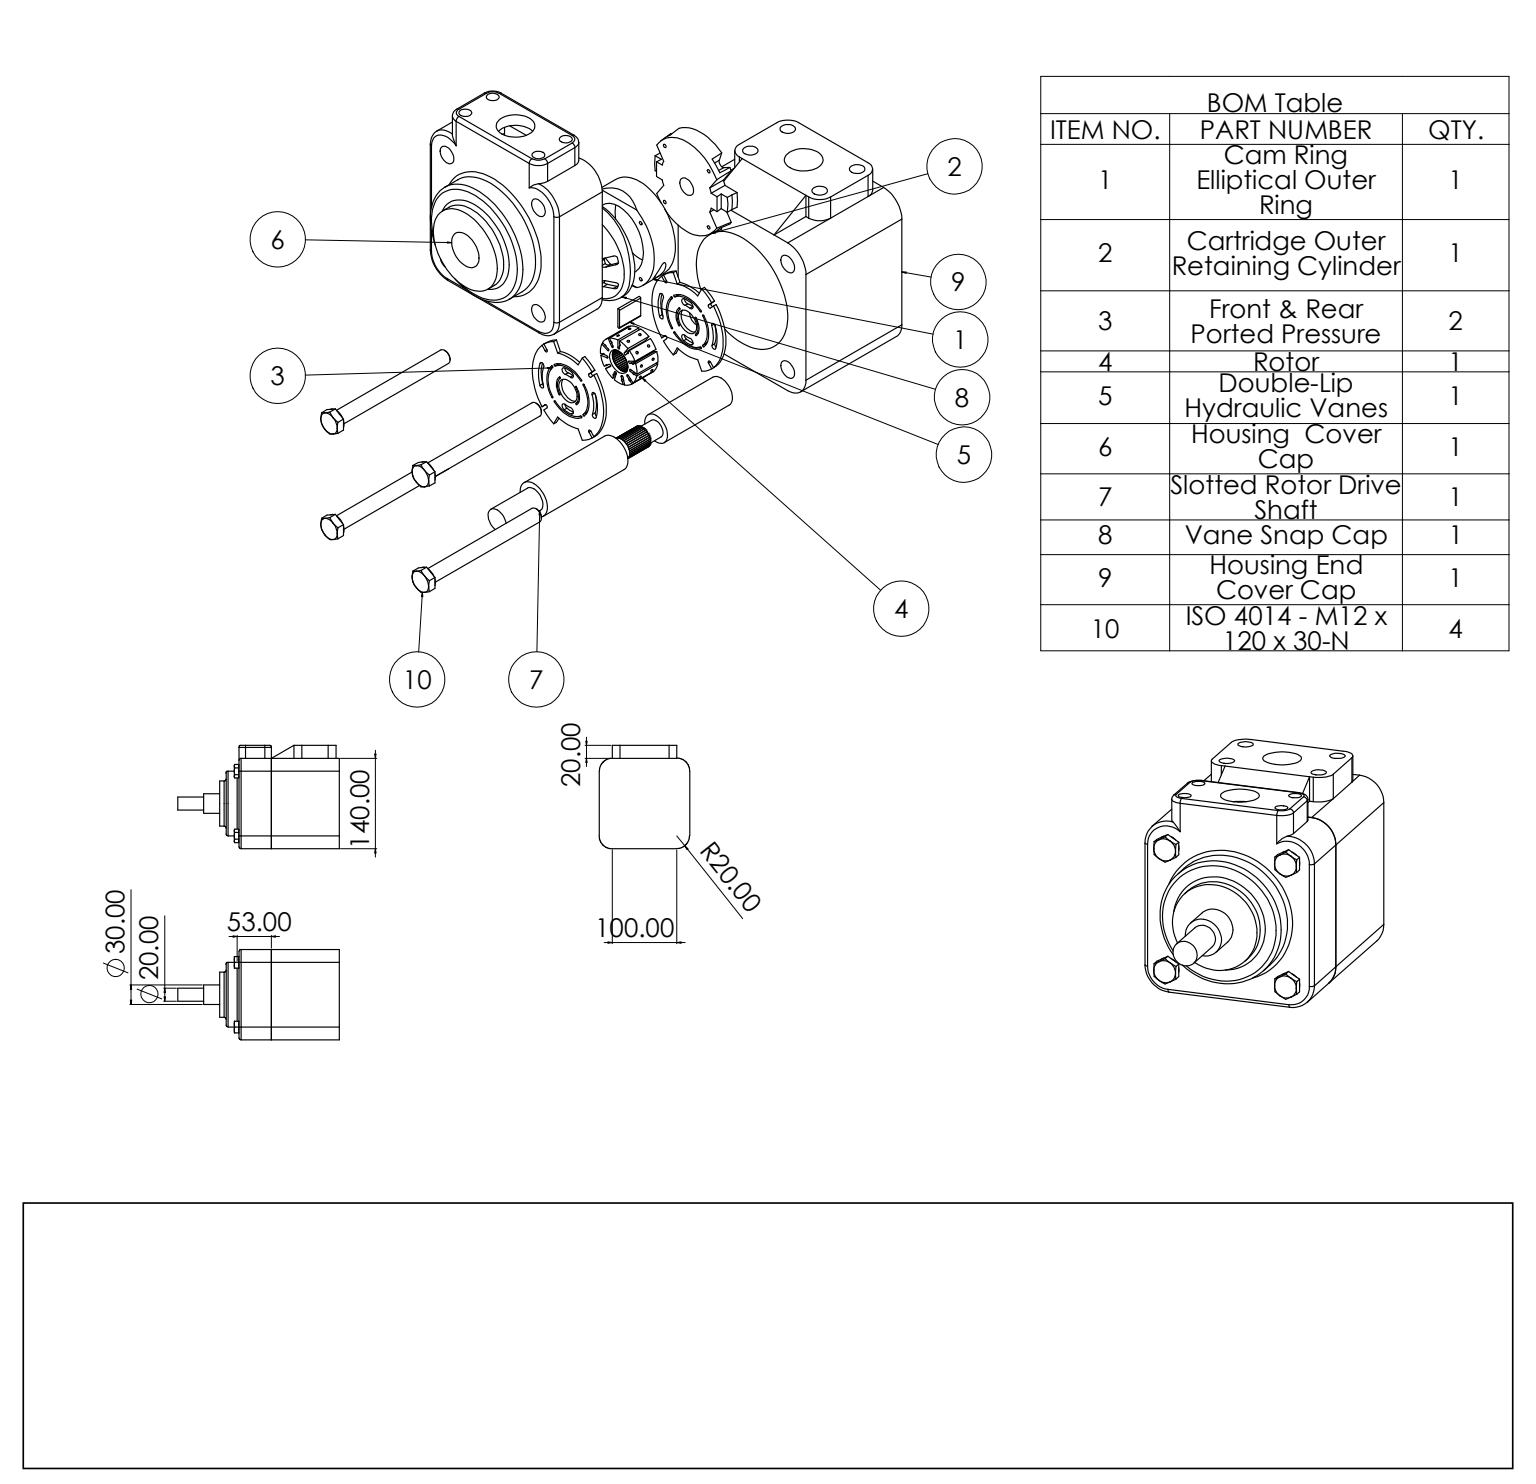
ISO-10303-21;
HEADER;
FILE_DESCRIPTION (('STEP AP214'),
    '1' );
FILE_NAME ('MAS-342',
    '2026-10-18T20:16:25',
    ( '' ),
    ( '' ),
    'SwSTEP 2.0',
    'SolidWorks 2025',
    '' );
FILE_SCHEMA (( 'AUTOMOTIVE_DESIGN' ));
ENDSEC;

DATA;
#1 = FACE_OUTER_BOUND ( 'NONE', #19385, .T. ) ;
#2 = DIRECTION ( 'NONE',  ( 0.000000000000000000, 0.000000000000000000, -1.000000000000000000 ) ) ;
#3 = CARTESIAN_POINT ( 'NONE',  ( 37.16608720827707657, 51.86186943028246787, 12.49999999999999112 ) ) ;
#4 = AXIS2_PLACEMENT_3D ( 'NONE', #28751, #28908, #7543 ) ;
#5 = CARTESIAN_POINT ( 'NONE',  ( -18.15804816958924306, -34.11099862341368549, 27.50000000000000000 ) ) ;
#6 = ADVANCED_FACE ( 'NONE', ( #26858 ), #19364, .F. ) ;
#7 = CARTESIAN_POINT ( 'NONE',  ( -10.18506332983503881, -29.04537757311073065, 24.50000000000000000 ) ) ;
#8 = EDGE_LOOP ( 'NONE', ( #14143, #4167, #13185, #29281 ) ) ;
#9 = CARTESIAN_POINT ( 'NONE',  ( -8.101746394734353984, -38.49011865887880646, 34.49999999999998579 ) ) ;
#10 = DIRECTION ( 'NONE',  ( 1.000000000000000000, 0.000000000000000000, 0.000000000000000000 ) ) ;
#11 = AXIS2_PLACEMENT_3D ( 'NONE', #21550, #14547, #24043 ) ;
#12 = DIRECTION ( 'NONE',  ( 1.000000000000000000, 0.000000000000000000, 0.000000000000000000 ) ) ;
#13 = EDGE_LOOP ( 'NONE', ( #16874, #3981 ) ) ;
#14 = CARTESIAN_POINT ( 'NONE',  ( 0.000000000000000000, 0.000000000000000000, 12.49999999999998401 ) ) ;
#15 = ORIENTED_EDGE ( 'NONE', *, *, #5581, .T. ) ;
#16 = CARTESIAN_POINT ( 'NONE',  ( 6.437793815610356241, -6.974883619896809606, 1.500000000000001332 ) ) ;
#17 = CARTESIAN_POINT ( 'NONE',  ( -9.060903275275968838, 42.96476308719554993, -16.50000000000000000 ) ) ;
#18 = VERTEX_POINT ( 'NONE', #24496 ) ;
#19 = CARTESIAN_POINT ( 'NONE',  ( 24.39344986792568903, -29.07448411189255211, 27.50000000000001066 ) ) ;
#20 = EDGE_CURVE ( 'NONE', #8430, #1741, #30742, .T. ) ;
#21 = CARTESIAN_POINT ( 'NONE',  ( -49.99999999999955236, -4.926614671774132148E-13, 82.49999999999998579 ) ) ;
#22 = EDGE_CURVE ( 'NONE', #25287, #29372, #18804, .T. ) ;
#23 = LINE ( 'NONE', #9535, #4037 ) ;
#24 = CARTESIAN_POINT ( 'NONE',  ( 0.3552109633508558351, -3.484997970623677332, -9.000000000000000000 ) ) ;
#25 = AXIS2_PLACEMENT_3D ( 'NONE', #902, #17278, #15225 ) ;
#26 = CARTESIAN_POINT ( 'NONE',  ( 30.75232512042845556, -9.966982604840845639, 1.500000000000000000 ) ) ;
#27 = ADVANCED_FACE ( 'NONE', ( #781 ), #12350, .T. ) ;
#28 = FACE_OUTER_BOUND ( 'NONE', #21455, .T. ) ;
#29 = ORIENTED_EDGE ( 'NONE', *, *, #10327, .T. ) ;
#30 = EDGE_CURVE ( 'NONE', #13253, #5262, #636, .T. ) ;
#31 = DIRECTION ( 'NONE',  ( 0.000000000000000000, 0.000000000000000000, 1.000000000000000000 ) ) ;
#32 = CARTESIAN_POINT ( 'NONE',  ( -20.65888525914364493, -38.75220717792906555, -19.50000000000000355 ) ) ;
#33 = CARTESIAN_POINT ( 'NONE',  ( -3.912171961292007616, -8.637616862297829101, 1.500000000000001332 ) ) ;
#34 = VERTEX_POINT ( 'NONE', #489 ) ;
#35 = EDGE_CURVE ( 'NONE', #21045, #27073, #21273, .T. ) ;
#36 = DIRECTION ( 'NONE',  ( -0.000000000000000000, -0.000000000000000000, 1.000000000000000000 ) ) ;
#37 = CARTESIAN_POINT ( 'NONE',  ( -14.84326473672822821, -8.425446036094903945, 20.06253562465620632 ) ) ;
#39 = EDGE_CURVE ( 'NONE', #26631, #4645, #16306, .T. ) ;
#38 = CARTESIAN_POINT ( 'NONE',  ( 0.000000000000000000, 0.000000000000000000, 1.500000000000001332 ) ) ;
#40 = CARTESIAN_POINT ( 'NONE',  ( 4.967306913940536361, 16.28142803850090203, 6.973843882838223429 ) ) ;
#41 = CARTESIAN_POINT ( 'NONE',  ( 39.83602371821015709, 11.57901747687536265, -19.50000000000000355 ) ) ;
#42 = EDGE_CURVE ( 'NONE', #19602, #22873, #7666, .T. ) ;
#43 = ORIENTED_EDGE ( 'NONE', *, *, #8838, .F. ) ;
#44 = LINE ( 'NONE', #17187, #10483 ) ;
#45 = EDGE_CURVE ( 'NONE', #5916, #3823, #10340, .T. ) ;
#46 = CARTESIAN_POINT ( 'NONE',  ( -24.03057240117690441, -26.57182937991348481, 26.54355021145563143 ) ) ;
#47 = CARTESIAN_POINT ( 'NONE',  ( 36.14613918203227172, 16.01870328439765601, 34.83083827288849221 ) ) ;
#48 = CARTESIAN_POINT ( 'NONE',  ( -6.228680293130167911, 19.00574304797303782, 5.679672709359373073 ) ) ;
#49 = ORIENTED_EDGE ( 'NONE', *, *, #24996, .T. ) ;
#50 = AXIS2_PLACEMENT_3D ( 'NONE', #18602, #5013, #4398 ) ;
#51 = CARTESIAN_POINT ( 'NONE',  ( 6.812559277181973627, -5.881244434206257310, 21.50000000000000000 ) ) ;
#52 = VERTEX_POINT ( 'NONE', #10007 ) ;
#53 = DIRECTION ( 'NONE',  ( 0.8412535328311813165, -0.5406408174555974444, 0.000000000000000000 ) ) ;
#54 = DIRECTION ( 'NONE',  ( 0.000000000000000000, 0.000000000000000000, 1.000000000000000000 ) ) ;
#55 = ORIENTED_EDGE ( 'NONE', *, *, #18763, .T. ) ;
#56 = ORIENTED_EDGE ( 'NONE', *, *, #27505, .T. ) ;
#57 = DIRECTION ( 'NONE',  ( -0.000000000000000000, -0.000000000000000000, 1.000000000000000000 ) ) ;
#58 =( REPRESENTATION_RELATIONSHIP ('NONE','NONE', #19885, #12322 ) REPRESENTATION_RELATIONSHIP_WITH_TRANSFORMATION ( #695 )SHAPE_REPRESENTATION_RELATIONSHIP( ) );
#59 = ORIENTED_EDGE ( 'NONE', *, *, #6132, .F. ) ;
#60 = ORIENTED_EDGE ( 'NONE', *, *, #10139, .T. ) ;
#61 = CARTESIAN_POINT ( 'NONE',  ( -0.02177409673011774377, -17.02558975896787885, 19.96783386855779341 ) ) ;
#62 = ADVANCED_FACE ( 'NONE', ( #24650 ), #17167, .F. ) ;
#63 = EDGE_CURVE ( 'NONE', #25705, #14162, #9332, .T. ) ;
#64 = CARTESIAN_POINT ( 'NONE',  ( -9.983339604393949074, -17.35078046477759983, 7.441806358946449151 ) ) ;
#65 = FACE_OUTER_BOUND ( 'NONE', #13496, .T. ) ;
#66 = CARTESIAN_POINT ( 'NONE',  ( 1.363408835038997458, -19.97112866468682668, 19.47783254395485031 ) ) ;
#67 = ORIENTED_EDGE ( 'NONE', *, *, #8805, .T. ) ;
#68 = EDGE_CURVE ( 'NONE', #8257, #20089, #6832, .T. ) ;
#69 = CARTESIAN_POINT ( 'NONE',  ( 6.899999999999999467, 5.196152422706624030, 9.000000000000001776 ) ) ;
#70 = CARTESIAN_POINT ( 'NONE',  ( 0.000000000000000000, 13.00000000000001421, 1.500000000000001332 ) ) ;
#71 = CARTESIAN_POINT ( 'NONE',  ( 14.24237608451263171, 14.06627278277045257, 19.69140814234746273 ) ) ;
#72 = LINE ( 'NONE', #9585, #22578 ) ;
#73 = ORIENTED_EDGE ( 'NONE', *, *, #24989, .F. ) ;
#74 = AXIS2_PLACEMENT_3D ( 'NONE', #21270, #28002, #15999 ) ;
#75 = DIRECTION ( 'NONE',  ( 0.000000000000000000, 0.000000000000000000, 1.000000000000000000 ) ) ;
#76 = CARTESIAN_POINT ( 'NONE',  ( -17.59891439103365585, -9.538503746949022144, 6.672349528511551497 ) ) ;
#77 = CARTESIAN_POINT ( 'NONE',  ( -13.11527592942575282, -10.04126165406389326, 1.500000000000000000 ) ) ;
#78 = DIRECTION ( 'NONE',  ( -1.000000000000000000, 0.000000000000000000, 0.000000000000000000 ) ) ;
#79 = CARTESIAN_POINT ( 'NONE',  ( 0.000000000000000000, 0.000000000000000000, 9.000000000000000000 ) ) ;
#80 = EDGE_CURVE ( 'NONE', #24431, #1715, #12846, .T. ) ;
#81 = CARTESIAN_POINT ( 'NONE',  ( -1.073881485057447405, -0.9711784013058452070, 1.500000000000000000 ) ) ;
#82 = CARTESIAN_POINT ( 'NONE',  ( 6.900000000000000355, 0.000000000000000000, 0.000000000000000000 ) ) ;
#83 = EDGE_LOOP ( 'NONE', ( #20575, #9372 ) ) ;
#84 = ORIENTED_EDGE ( 'NONE', *, *, #27745, .T. ) ;
#85 = CARTESIAN_POINT ( 'NONE',  ( -37.98493438988125348, -11.12428508575252728, -1.500000000000000000 ) ) ;
#86 = DIRECTION ( 'NONE',  ( 0.000000000000000000, 0.000000000000000000, -1.000000000000000000 ) ) ;
#88 = DIRECTION ( 'NONE',  ( 1.000000000000000000, 0.000000000000000000, 0.000000000000000000 ) ) ;
#87 = VECTOR ( 'NONE', #19138, 1000.000000000000000 ) ;
#89 = ORIENTED_EDGE ( 'NONE', *, *, #20188, .F. ) ;
#90 = CARTESIAN_POINT ( 'NONE',  ( 15.47797589786116923, -7.092492006142040673, 19.96783386855779341 ) ) ;
#91 = CARTESIAN_POINT ( 'NONE',  ( 6.171684994647412381, 19.04275422834224685, 6.211014596808754007 ) ) ;
#92 = EDGE_CURVE ( 'NONE', #21118, #30725, #17328, .T. ) ;
#93 = ORIENTED_EDGE ( 'NONE', *, *, #3486, .F. ) ;
#94 = DIRECTION ( 'NONE',  ( 1.000000000000000000, 0.000000000000000000, 0.000000000000000000 ) ) ;
#95 = CARTESIAN_POINT ( 'NONE',  ( 11.67645754117908830, 12.46194352177089293, 6.892848776733236704 ) ) ;
#96 = EDGE_CURVE ( 'NONE', #21713, #6692, #24023, .T. ) ;
#97 = FACE_OUTER_BOUND ( 'NONE', #28084, .T. ) ;
#98 = CARTESIAN_POINT ( 'NONE',  ( -37.93368909164158254, 9.961195697873989729, 34.97277436636965575 ) ) ;
#99 = ORIENTED_EDGE ( 'NONE', *, *, #3233, .T. ) ;
#100 = CARTESIAN_POINT ( 'NONE',  ( 0.000000000000000000, 0.000000000000000000, 1.500000000000001332 ) ) ;
#101 = CARTESIAN_POINT ( 'NONE',  ( 0.000000000000000000, 0.000000000000000000, -87.50000000000000000 ) ) ;
#102 = CARTESIAN_POINT ( 'NONE',  ( 22.58267429318970443, -26.57182937991349903, 26.54355021145563143 ) ) ;
#103 = ORIENTED_EDGE ( 'NONE', *, *, #23860, .T. ) ;
#104 = CARTESIAN_POINT ( 'NONE',  ( -18.38748676655956515, -7.913428453147655084, 6.018569869498933578 ) ) ;
#105 = CARTESIAN_POINT ( 'NONE',  ( 14.46116907065692736, 13.81605838820130394, 7.454606537396340826 ) ) ;
#106 = CARTESIAN_POINT ( 'NONE',  ( 0.06889080212831104333, -17.02733034922398758, 5.940635272151477686 ) ) ;
#107 = CYLINDRICAL_SURFACE ( 'NONE', #23715, 10.00000000000003375 ) ;
#108 = LINE ( 'NONE', #21001, #12544 ) ;
#109 = CARTESIAN_POINT ( 'NONE',  ( -19.94989956810792009, 1.646935350084928418, 19.89182036555910571 ) ) ;
#110 = DIRECTION ( 'NONE',  ( 0.000000000000000000, 1.000000000000000000, 0.000000000000000000 ) ) ;
#111 = ORIENTED_EDGE ( 'NONE', *, *, #4642, .T. ) ;
#112 = CARTESIAN_POINT ( 'NONE',  ( 11.47892014274828654, -16.39977715623752275, 20.25542030744407640 ) ) ;
#113 = CIRCLE ( 'NONE', #24448, 0.7500000000000007772 ) ;
#114 = CARTESIAN_POINT ( 'NONE',  ( 57.49999999999998579, -50.00000000000000000, 97.07879600563551037 ) ) ;
#115 = VERTEX_POINT ( 'NONE', #22003 ) ;
#116 = EDGE_LOOP ( 'NONE', ( #16345, #15698, #26338, #11828 ) ) ;
#117 = CARTESIAN_POINT ( 'NONE',  ( 4.695984468547702129, 19.44110619659980799, 20.15039051365864253 ) ) ;
#118 = CARTESIAN_POINT ( 'NONE',  ( -12.19297718786180695, 48.49133510641088662, -63.75033992389879245 ) ) ;
#119 = VERTEX_POINT ( 'NONE', #15443 ) ;
#120 = FACE_OUTER_BOUND ( 'NONE', #29698, .T. ) ;
#121 = VECTOR ( 'NONE', #17231, 1000.000000000000000 ) ;
#122 = CARTESIAN_POINT ( 'NONE',  ( -10.72135862580927146, -16.90494006806149940, 7.632642797338977658 ) ) ;
#123 = ORIENTED_EDGE ( 'NONE', *, *, #26128, .F. ) ;
#124 = AXIS2_PLACEMENT_3D ( 'NONE', #18042, #3695, #8540 ) ;
#125 = CARTESIAN_POINT ( 'NONE',  ( 18.71580048965418541, -7.100988023106708624, 19.03762469184452755 ) ) ;
#126 = CARTESIAN_POINT ( 'NONE',  ( 16.55849529797290032, 4.179294809495488039, 19.14333282897057842 ) ) ;
#127 = EDGE_CURVE ( 'NONE', #8705, #8129, #11228, .T. ) ;
#128 = CARTESIAN_POINT ( 'NONE',  ( 0.000000000000000000, -2.435693370351110282E-15, 21.50000000000000355 ) ) ;
#129 = ORIENTED_EDGE ( 'NONE', *, *, #25599, .F. ) ;
#130 = EDGE_CURVE ( 'NONE', #28271, #10764, #20221, .T. ) ;
#131 = CARTESIAN_POINT ( 'NONE',  ( 23.21352257770656635, -10.78826658734920052, 45.15942333309103418 ) ) ;
#132 = ORIENTED_EDGE ( 'NONE', *, *, #23307, .F. ) ;
#133 = ORIENTED_EDGE ( 'NONE', *, *, #19082, .T. ) ;
#134 = CARTESIAN_POINT ( 'NONE',  ( 7.706848733600953238, 5.524309650260795124, 1.500000000000001332 ) ) ;
#135 = CARTESIAN_POINT ( 'NONE',  ( -12.90456292687989759, 11.10871050118981529, 20.05479082170252525 ) ) ;
#136 = CARTESIAN_POINT ( 'NONE',  ( -9.972083266784119715, -17.35726207598482773, 18.56793045041961321 ) ) ;
#137 = CARTESIAN_POINT ( 'NONE',  ( -15.05112753842527162, -8.020416455032004066, 20.34789198813115263 ) ) ;
#138 = AXIS2_PLACEMENT_3D ( 'NONE', #523, #22041, #27196 ) ;
#139 = CARTESIAN_POINT ( 'NONE',  ( 1.767905995611233072, -16.98559759804142288, 19.61324152429826739 ) ) ;
#140 = CARTESIAN_POINT ( 'NONE',  ( 16.82202058066696537, 2.664153601443035146, 18.49267272388512140 ) ) ;
#141 = ORIENTED_EDGE ( 'NONE', *, *, #9150, .T. ) ;
#142 = AXIS2_PLACEMENT_3D ( 'NONE', #29835, #3468, #10482 ) ;
#143 = CARTESIAN_POINT ( 'NONE',  ( 11.01999061743883956, -16.71182566173002826, 7.652108011868850035 ) ) ;
#144 = CARTESIAN_POINT ( 'NONE',  ( 8.480328572437745294, -4.608906612435629491, 21.50000000000000000 ) ) ;
#145 = LINE ( 'NONE', #9510, #21267 ) ;
#146 = ORIENTED_EDGE ( 'NONE', *, *, #2958, .F. ) ;
#147 = LINE ( 'NONE', #19489, #17289 ) ;
#148 = CARTESIAN_POINT ( 'NONE',  ( -37.16608720827707657, -65.00000000000000000, 57.49999999999999289 ) ) ;
#149 = CARTESIAN_POINT ( 'NONE',  ( 1.000000000000008438, 13.00000000000001421, 1.500000000000001332 ) ) ;
#150 = CARTESIAN_POINT ( 'NONE',  ( 2.878478920843521749, -0.8451976705243363641, 24.50000000000000000 ) ) ;
#151 = CARTESIAN_POINT ( 'NONE',  ( 12.00212711880201510, 12.12705342296112221, 7.545655578832108468 ) ) ;
#152 = CARTESIAN_POINT ( 'NONE',  ( 8.099999999999999645, 0.000000000000000000, 0.000000000000000000 ) ) ;
#153 = CARTESIAN_POINT ( 'NONE',  ( -5.488535287689156661, 19.23255048776057308, 5.775318986477953054 ) ) ;
#154 = VERTEX_POINT ( 'NONE', #22460 ) ;
#155 = CARTESIAN_POINT ( 'NONE',  ( -7.108788511070779137, -38.72574257930638453, 34.49999999999999289 ) ) ;
#156 = DIRECTION ( 'NONE',  ( -0.000000000000000000, 0.000000000000000000, 1.000000000000000000 ) ) ;
#157 = ORIENTED_EDGE ( 'NONE', *, *, #6998, .F. ) ;
#158 = DIRECTION ( 'NONE',  ( 1.000000000000000000, 0.000000000000000000, 0.000000000000000000 ) ) ;
#159 = VECTOR ( 'NONE', #18850, 1000.000000000000000 ) ;
#160 = VERTEX_POINT ( 'NONE', #4060 ) ;
#161 = CARTESIAN_POINT ( 'NONE',  ( 16.17271416092067682, -5.480318835022405466, 6.995624166085161910 ) ) ;
#162 = AXIS2_PLACEMENT_3D ( 'NONE', #23397, #25742, #23542 ) ;
#163 = DIRECTION ( 'NONE',  ( 1.000000000000000000, 0.000000000000000000, -0.000000000000000000 ) ) ;
#164 = DIRECTION ( 'NONE',  ( 1.000000000000000000, -0.000000000000000000, 0.000000000000000000 ) ) ;
#165 = VERTEX_POINT ( 'NONE', #8736 ) ;
#166 = CARTESIAN_POINT ( 'NONE',  ( 22.55938241427807256, 30.80590877286595841, 27.50000000000000355 ) ) ;
#167 = DIRECTION ( 'NONE',  ( 1.000000000000000000, 0.000000000000000000, 0.000000000000000000 ) ) ;
#168 = LINE ( 'NONE', #19198, #17487 ) ;
#169 = CARTESIAN_POINT ( 'NONE',  ( 32.24119435725080507, -26.76047165977712794, -16.50000600000000262 ) ) ;
#170 = DIRECTION ( 'NONE',  ( -0.000000000000000000, -0.000000000000000000, 1.000000000000000000 ) ) ;
#171 = CARTESIAN_POINT ( 'NONE',  ( -30.03865005752669148, 15.52610542268208604, 41.18623755349101856 ) ) ;
#172 = ORIENTED_EDGE ( 'NONE', *, *, #2713, .T. ) ;
#173 = DIRECTION ( 'NONE',  ( 0.000000000000000000, 0.000000000000000000, 1.000000000000000000 ) ) ;
#174 = VECTOR ( 'NONE', #2091, 1000.000000000000000 ) ;
#175 = CARTESIAN_POINT ( 'NONE',  ( -10.64374042650075403, -42.96126232887726815, -19.50000000000000355 ) ) ;
#176 = CARTESIAN_POINT ( 'NONE',  ( 39.70095622563236049, 7.028748154183632302, -13.16666434799647689 ) ) ;
#177 = ORIENTED_EDGE ( 'NONE', *, *, #24246, .F. ) ;
#178 = DIRECTION ( 'NONE',  ( 1.000000000000000000, 0.000000000000000000, 0.000000000000000000 ) ) ;
#179 = CIRCLE ( 'NONE', #30097, 0.5999999999999998668 ) ;
#180 = DIRECTION ( 'NONE',  ( 1.000000000000000000, 0.000000000000000000, 0.000000000000000000 ) ) ;
#181 = CARTESIAN_POINT ( 'NONE',  ( 3.993622308618880901, 8.159193615868410632, 21.50000000000000000 ) ) ;
#182 = AXIS2_PLACEMENT_3D ( 'NONE', #29243, #7886, #17394 ) ;
#183 = CARTESIAN_POINT ( 'NONE',  ( 4.641725321133337800, 16.38498716464899019, 5.848946451764561516 ) ) ;
#184 = CARTESIAN_POINT ( 'NONE',  ( -35.76344986165604212, -22.29344514668547461, -19.50000000000000355 ) ) ;
#185 = ORIENTED_EDGE ( 'NONE', *, *, #19570, .F. ) ;
#186 = SURFACE_STYLE_USAGE ( .BOTH. , #19677 ) ;
#187 = EDGE_CURVE ( 'NONE', #14088, #4162, #7585, .T. ) ;
#188 = CARTESIAN_POINT ( 'NONE',  ( 27.51850911855329329, 30.14776422306135117, 30.03356538881464743 ) ) ;
#189 = EDGE_CURVE ( 'NONE', #1099, #580, #18256, .T. ) ;
#190 = DIRECTION ( 'NONE',  ( -0.6707505147970024284, 0.7416830501633134842, 0.000000000000000000 ) ) ;
#191 = VERTEX_POINT ( 'NONE', #3449 ) ;
#192 = EDGE_CURVE ( 'NONE', #26671, #20986, #30262, .T. ) ;
#193 = CARTESIAN_POINT ( 'NONE',  ( 7.392982946727082449, -5.278755796068694828, -1.500000000000002442 ) ) ;
#194 = VERTEX_POINT ( 'NONE', #13123 ) ;
#195 = DIRECTION ( 'NONE',  ( 0.000000000000000000, 0.000000000000000000, 1.000000000000000000 ) ) ;
#196 = CARTESIAN_POINT ( 'NONE',  ( 39.99999999999998579, 87.00000000000001421, 12.49999999999999112 ) ) ;
#197 = ORIENTED_EDGE ( 'NONE', *, *, #29811, .T. ) ;
#198 = ADVANCED_FACE ( 'NONE', ( #25436 ), #29650, .F. ) ;
#199 = ORIENTED_EDGE ( 'NONE', *, *, #12643, .T. ) ;
#200 = CARTESIAN_POINT ( 'NONE',  ( -9.658933677579515376, -17.51307076256854600, 6.392525840300335105 ) ) ;
#201 = EDGE_CURVE ( 'NONE', #20672, #10252, #28885, .T. ) ;
#202 = PRODUCT_DEFINITION_SHAPE ( 'NONE', 'NONE',  #30865 ) ;
#203 = VERTEX_POINT ( 'NONE', #17802 ) ;
#204 = ORIENTED_EDGE ( 'NONE', *, *, #13604, .T. ) ;
#205 = CARTESIAN_POINT ( 'NONE',  ( -0.1973194101962232605, -20.01708124257648791, 20.19668224736330941 ) ) ;
#206 = CIRCLE ( 'NONE', #4196, 0.7441270634457181066 ) ;
#207 = EDGE_CURVE ( 'NONE', #23407, #26039, #29815, .T. ) ;
#208 = DIRECTION ( 'NONE',  ( 0.000000000000000000, 0.000000000000000000, -1.000000000000000000 ) ) ;
#209 = CARTESIAN_POINT ( 'NONE',  ( 4.045242219987651211, 16.55840560649980731, 18.34798005863078885 ) ) ;
#210 = EDGE_CURVE ( 'NONE', #17431, #24948, #5944, .T. ) ;
#211 = CARTESIAN_POINT ( 'NONE',  ( 0.8978415369256412815, -19.99755156235223552, 18.50655187082627862 ) ) ;
#212 = EDGE_LOOP ( 'NONE', ( #3421, #739, #13868, #11454 ) ) ;
#213 = CARTESIAN_POINT ( 'NONE',  ( -19.54426622602688113, -37.07991288358296345, -1.499999999999999778 ) ) ;
#214 = EDGE_CURVE ( 'NONE', #13827, #7727, #27159, .T. ) ;
#215 = CARTESIAN_POINT ( 'NONE',  ( 24.35970437652574105, 13.37404834226503958, 47.21042702067963859 ) ) ;
#216 = FACE_OUTER_BOUND ( 'NONE', #25286, .T. ) ;
#217 = CARTESIAN_POINT ( 'NONE',  ( 19.49999999999992539, 1.626584906615178899E-14, 62.49999999999999289 ) ) ;
#218 = ORIENTED_EDGE ( 'NONE', *, *, #11268, .F. ) ;
#219 = CARTESIAN_POINT ( 'NONE',  ( 50.00000000000045475, -4.865382331816764069E-13, 79.49999999999998579 ) ) ;
#220 = FACE_OUTER_BOUND ( 'NONE', #17515, .T. ) ;
#221 = CARTESIAN_POINT ( 'NONE',  ( -6.449126838413862473, 15.81136745782587383, 6.995624166085161910 ) ) ;
#222 = DIRECTION ( 'NONE',  ( 0.000000000000000000, -1.132880637372608986E-16, 1.000000000000000000 ) ) ;
#223 = CARTESIAN_POINT ( 'NONE',  ( 0.1482032042127262861, 2.204400401860216796, 9.000000000000001776 ) ) ;
#224 = B_SPLINE_CURVE_WITH_KNOTS ( 'NONE', 3,
 ( #24253, #10067, #7738, #5394 ),
 .UNSPECIFIED., .F., .F.,
 ( 4, 4 ),
 ( 2.143643656977390230E-07, 0.003421830178490235883 ),
 .UNSPECIFIED. ) ;
#225 = CARTESIAN_POINT ( 'NONE',  ( -18.38748676655957937, -7.913428453147655084, 18.71435384576123440 ) ) ;
#226 = CARTESIAN_POINT ( 'NONE',  ( 4.770489558936219510E-15, -42.50000000000000000, -1.500000000000000000 ) ) ;
#227 = ORIENTED_EDGE ( 'NONE', *, *, #29230, .T. ) ;
#228 = VERTEX_POINT ( 'NONE', #15599 ) ;
#229 = DIRECTION ( 'NONE',  ( -0.000000000000000000, -0.000000000000000000, -1.000000000000000000 ) ) ;
#230 = AXIS2_PLACEMENT_3D ( 'NONE', #30774, #53, #30611 ) ;
#231 = CARTESIAN_POINT ( 'NONE',  ( 32.74775157611827581, 27.21557300921217859, -19.50000000000000355 ) ) ;
#232 = EDGE_CURVE ( 'NONE', #24670, #7391, #17304, .T. ) ;
#233 = DIRECTION ( 'NONE',  ( -0.000000000000000000, -0.000000000000000000, 1.000000000000000000 ) ) ;
#234 = ADVANCED_FACE ( 'NONE', ( #15282 ), #1429, .T. ) ;
#235 = CARTESIAN_POINT ( 'NONE',  ( 11.21631477658334042, -16.55933310271405645, 20.34789198813115618 ) ) ;
#236 = ORIENTED_EDGE ( 'NONE', *, *, #10906, .T. ) ;
#237 = SHAPE_DEFINITION_REPRESENTATION ( #26098, #10307 ) ;
#238 = EDGE_CURVE ( 'NONE', #14629, #10409, #29758, .T. ) ;
#239 = CARTESIAN_POINT ( 'NONE',  ( 18.21588581002257001, -8.300927319590597264, 18.39701043959520987 ) ) ;
#240 = CARTESIAN_POINT ( 'NONE',  ( 5.984782097461514461, 19.10229623552459088, 5.940635272151477686 ) ) ;
#241 = EDGE_LOOP ( 'NONE', ( #4483, #26412, #12849, #13561 ) ) ;
#242 = DIRECTION ( 'NONE',  ( 0.000000000000000000, 0.000000000000000000, 1.000000000000000000 ) ) ;
#243 = ADVANCED_FACE ( 'NONE', ( #23525 ), #20886, .F. ) ;
#244 = CIRCLE ( 'NONE', #26653, 0.7441270634457198829 ) ;
#245 = CARTESIAN_POINT ( 'NONE',  ( -0.4564504349075055867, 9.471281197126600659, 13.00000000000000178 ) ) ;
#246 = CARTESIAN_POINT ( 'NONE',  ( -7.856594496258223259, -4.390207617113929039, -1.500000000000002220 ) ) ;
#247 = CARTESIAN_POINT ( 'NONE',  ( -36.79585557548701757, 7.262324983800692912, 37.49999999996946087 ) ) ;
#248 = ORIENTED_EDGE ( 'NONE', *, *, #13418, .T. ) ;
#249 = EDGE_CURVE ( 'NONE', #25840, #22179, #829, .T. ) ;
#250 = CARTESIAN_POINT ( 'NONE',  ( 0.000000000000000000, 0.000000000000000000, 21.50000000000000000 ) ) ;
#251 = EDGE_CURVE ( 'NONE', #24781, #12321, #29562, .T. ) ;
#252 = LINE ( 'NONE', #7437, #4085 ) ;
#253 = CARTESIAN_POINT ( 'NONE',  ( 11.29353189506152511, 42.33618545487009754, -16.50000000000000355 ) ) ;
#254 = VERTEX_POINT ( 'NONE', #21492 ) ;
#255 = CARTESIAN_POINT ( 'NONE',  ( -18.32589276785170185, -8.054604467211150975, 7.429667576816606278 ) ) ;
#256 = AXIS2_PLACEMENT_3D ( 'NONE', #17662, #8160, #8483 ) ;
#257 = DIRECTION ( 'NONE',  ( 0.000000000000000000, 0.000000000000000000, 1.000000000000000000 ) ) ;
#258 = PLANE ( 'NONE',  #5321 ) ;
#259 = CARTESIAN_POINT ( 'NONE',  ( -8.268028093133393597, -3.763133143576407047, 13.22130136205108819 ) ) ;
#260 = DIRECTION ( 'NONE',  ( -0.000000000000000000, 1.132880637372608986E-16, -1.000000000000000000 ) ) ;
#261 = PLANE ( 'NONE',  #7575 ) ;
#262 = CARTESIAN_POINT ( 'NONE',  ( 37.01111991330344608, -13.41299137855487977, 15.98316150592440543 ) ) ;
#263 = DIRECTION ( 'NONE',  ( 0.000000000000000000, 0.000000000000000000, -1.000000000000000000 ) ) ;
#264 = ORIENTED_EDGE ( 'NONE', *, *, #13066, .T. ) ;
#265 = EDGE_CURVE ( 'NONE', #30031, #12516, #9139, .T. ) ;
#266 = EDGE_CURVE ( 'NONE', #6035, #4843, #28573, .T. ) ;
#267 = DIRECTION ( 'NONE',  ( 1.000000000000000000, 0.000000000000000000, 0.000000000000000000 ) ) ;
#268 = CARTESIAN_POINT ( 'NONE',  ( 0.000000000000000000, 1.102182119232617714E-15, -9.000000000000000000 ) ) ;
#269 = ORIENTED_EDGE ( 'NONE', *, *, #9974, .T. ) ;
#270 = ORIENTED_EDGE ( 'NONE', *, *, #22948, .T. ) ;
#271 = LINE ( 'NONE', #18686, #17607 ) ;
#272 = CARTESIAN_POINT ( 'NONE',  ( -14.80496105867816503, 47.75796600471949205, -57.46067695234416561 ) ) ;
#273 = ORIENTED_EDGE ( 'NONE', *, *, #3850, .F. ) ;
#274 = DIRECTION ( 'NONE',  ( -0.000000000000000000, 0.000000000000000000, 1.000000000000000000 ) ) ;
#275 = CIRCLE ( 'NONE', #26685, 10.00000000000003197 ) ;
#276 = FACE_BOUND ( 'NONE', #21490, .T. ) ;
#277 = ORIENTED_EDGE ( 'NONE', *, *, #12266, .F. ) ;
#278 = CARTESIAN_POINT ( 'NONE',  ( 18.65245237681030588, -7.265846841151810231, 19.97651184436794125 ) ) ;
#279 = CARTESIAN_POINT ( 'NONE',  ( 16.55484456677775640, 4.196195780087080607, 19.25672174529527325 ) ) ;
#280 = LINE ( 'NONE', #9800, #11506 ) ;
#281 = VERTEX_POINT ( 'NONE', #19019 ) ;
#282 = DIRECTION ( 'NONE',  ( -0.000000000000000000, -0.000000000000000000, -1.000000000000000000 ) ) ;
#283 = VECTOR ( 'NONE', #6940, 1000.000000000000000 ) ;
#284 = ORIENTED_EDGE ( 'NONE', *, *, #16662, .T. ) ;
#285 = CARTESIAN_POINT ( 'NONE',  ( 31.61046531718064045, -26.43913157134468861, -9.833326303308560057 ) ) ;
#286 = CARTESIAN_POINT ( 'NONE',  ( -14.75808792347767628, 13.52460813173914467, 18.90679857307105749 ) ) ;
#287 = CARTESIAN_POINT ( 'NONE',  ( -7.919226493207297324, -15.11997014267743289, 18.64703902303423178 ) ) ;
#288 = AXIS2_PLACEMENT_3D ( 'NONE', #22323, #7993, #29353 ) ;
#289 = CARTESIAN_POINT ( 'NONE',  ( -32.19782014694307293, -14.25394737442115733, 39.78814634291943264 ) ) ;
#290 = CYLINDRICAL_SURFACE ( 'NONE', #21952, 0.7500000000000006661 ) ;
#291 = PLANE ( 'NONE',  #12367 ) ;
#292 = ORIENTED_EDGE ( 'NONE', *, *, #27712, .F. ) ;
#293 = EDGE_CURVE ( 'NONE', #13653, #26600, #10904, .T. ) ;
#294 = CARTESIAN_POINT ( 'NONE',  ( -19.73562743738982306, 3.350138464993962284, 18.80699882434806369 ) ) ;
#295 = CARTESIAN_POINT ( 'NONE',  ( 25.24511578250132260, -28.23443549260979779, 34.49999999999999289 ) ) ;
#296 = VECTOR ( 'NONE', #25590, 1000.000000000000000 ) ;
#297 = CARTESIAN_POINT ( 'NONE',  ( 14.88222593340886668, 13.36111339922579866, 20.34789198813115263 ) ) ;
#298 = CYLINDRICAL_SURFACE ( 'NONE', #9820, 0.7500000000000004441 ) ;
#299 = ORIENTED_EDGE ( 'NONE', *, *, #13066, .F. ) ;
#300 = ORIENTED_EDGE ( 'NONE', *, *, #15085, .F. ) ;
#301 = CARTESIAN_POINT ( 'NONE',  ( 39.52380524535330153, 7.028748154198969367, -6.500000000000000888 ) ) ;
#302 = DIRECTION ( 'NONE',  ( -0.8412535328311813165, 0.5406408174555974444, 0.000000000000000000 ) ) ;
#303 = DIRECTION ( 'NONE',  ( 0.9329908884337535513, 0.3598999890241665334, 0.000000000000000000 ) ) ;
#304 = CARTESIAN_POINT ( 'NONE',  ( -5.119216485953539397, 16.24645747311530641, 7.557577766377196582 ) ) ;
#305 = CARTESIAN_POINT ( 'NONE',  ( -6.437683520590124608, 6.962021646281596254, 21.50000000000000000 ) ) ;
#306 = CARTESIAN_POINT ( 'NONE',  ( -19.18576292979354392, -22.55620591602727742, 1.500000000000001332 ) ) ;
#307 = ORIENTED_EDGE ( 'NONE', *, *, #24204, .F. ) ;
#308 = ORIENTED_EDGE ( 'NONE', *, *, #27638, .F. ) ;
#309 = CARTESIAN_POINT ( 'NONE',  ( -8.593763153356288598, -38.36129777999322954, 34.49999999999998579 ) ) ;
#310 = CARTESIAN_POINT ( 'NONE',  ( -4.668110441710642711, -19.44758969394387194, 24.50000000000000000 ) ) ;
#311 = CARTESIAN_POINT ( 'NONE',  ( 7.028330626922776325, 10.93629592680536966, 24.50000000000000000 ) ) ;
#312 = ORIENTED_EDGE ( 'NONE', *, *, #28685, .F. ) ;
#313 = AXIS2_PLACEMENT_3D ( 'NONE', #7814, #17164, #27009 ) ;
#314 = CARTESIAN_POINT ( 'NONE',  ( 8.637616862297841536, -3.912171961291982747, 13.00000000000000178 ) ) ;
#315 = VERTEX_POINT ( 'NONE', #30412 ) ;
#316 = CARTESIAN_POINT ( 'NONE',  ( 16.17688602565676348, -5.469326772727310271, 6.341840715582230281 ) ) ;
#317 = AXIS2_PLACEMENT_3D ( 'NONE', #8530, #7913, #10548 ) ;
#318 = CARTESIAN_POINT ( 'NONE',  ( 0.7836604620899298990, -17.02735026737547841, 18.34798005863078885 ) ) ;
#319 = VECTOR ( 'NONE', #818, 1000.000000000000000 ) ;
#320 = DIRECTION ( 'NONE',  ( -1.000000000000000000, 0.000000000000000000, 0.000000000000000000 ) ) ;
#321 = VERTEX_POINT ( 'NONE', #30556 ) ;
#322 = CYLINDRICAL_SURFACE ( 'NONE', #25724, 20.32284676574538906 ) ;
#323 = LINE ( 'NONE', #5317, #8177 ) ;
#324 = DIRECTION ( 'NONE',  ( 1.000000000000000000, 0.000000000000000000, 0.000000000000000000 ) ) ;
#325 = DIRECTION ( 'NONE',  ( 1.000000000000000000, 0.000000000000000000, 0.000000000000000000 ) ) ;
#326 = VECTOR ( 'NONE', #28352, 1000.000000000000000 ) ;
#327 = DIRECTION ( 'NONE',  ( 1.000000000000000000, 0.000000000000000000, 0.000000000000000000 ) ) ;
#328 = CYLINDRICAL_SURFACE ( 'NONE', #23812, 9.482273699623480212 ) ;
#329 = EDGE_LOOP ( 'NONE', ( #2074, #5797, #19024, #28874 ) ) ;
#330 = DIRECTION ( 'NONE',  ( 0.000000000000000000, 1.000000000000000000, -0.000000000000000000 ) ) ;
#331 = AXIS2_PLACEMENT_3D ( 'NONE', #19612, #5728, #15222 ) ;
#332 = EDGE_CURVE ( 'NONE', #21638, #2008, #29122, .T. ) ;
#333 = CARTESIAN_POINT ( 'NONE',  ( -39.00000000000000000, 5.563236990218665134, -1.500000000000000000 ) ) ;
#334 = DIRECTION ( 'NONE',  ( 1.000000000000000000, 0.000000000000000000, 0.000000000000000000 ) ) ;
#335 = ORIENTED_EDGE ( 'NONE', *, *, #27473, .T. ) ;
#336 = CARTESIAN_POINT ( 'NONE',  ( 16.91972452348793610, -3.442972353390052920, 1.500000000000000000 ) ) ;
#337 = VECTOR ( 'NONE', #30659, 1000.000000000000000 ) ;
#338 = CARTESIAN_POINT ( 'NONE',  ( 37.49999999999997158, 1.387778780781445676E-14, 37.50000000000000000 ) ) ;
#339 = FACE_OUTER_BOUND ( 'NONE', #26193, .T. ) ;
#340 = CIRCLE ( 'NONE', #26766, 5.000000000000004441 ) ;
#341 = CARTESIAN_POINT ( 'NONE',  ( 5.015798959889809616, 16.26549279019889127, 6.519181285484532573 ) ) ;
#342 = CARTESIAN_POINT ( 'NONE',  ( -19.64114023396061981, 37.13592150528867109, -1.500000000000000000 ) ) ;
#343 = DIRECTION ( 'NONE',  ( -0.000000000000000000, -0.000000000000000000, 1.000000000000000000 ) ) ;
#344 = CARTESIAN_POINT ( 'NONE',  ( 30.96653510607171711, 25.84892707844779736, 34.59766498189470241 ) ) ;
#345 = CARTESIAN_POINT ( 'NONE',  ( 19.63503467057051566, 3.804509661152916333, 7.454606537396342603 ) ) ;
#346 = VERTEX_POINT ( 'NONE', #26975 ) ;
#347 = CARTESIAN_POINT ( 'NONE',  ( 33.67904611720809527, -24.24635140547922418, -14.83330431372250935 ) ) ;
#348 = ORIENTED_EDGE ( 'NONE', *, *, #25359, .F. ) ;
#349 = AXIS2_PLACEMENT_3D ( 'NONE', #29658, #10628, #8296 ) ;
#350 = DIRECTION ( 'NONE',  ( 1.000000000000000000, -0.000000000000000000, 0.000000000000000000 ) ) ;
#351 = FACE_OUTER_BOUND ( 'NONE', #19038, .T. ) ;
#352 = EDGE_LOOP ( 'NONE', ( #24327, #26757, #11753, #27954 ) ) ;
#353 = VERTEX_POINT ( 'NONE', #24142 ) ;
#354 = CARTESIAN_POINT ( 'NONE',  ( -10.51513057463695233, -17.01270198993486460, 7.652108011868850035 ) ) ;
#355 = ORIENTED_EDGE ( 'NONE', *, *, #15805, .F. ) ;
#356 = CIRCLE ( 'NONE', #4344, 0.7500000000000006661 ) ;
#357 = VERTEX_POINT ( 'NONE', #453 ) ;
#358 = ORIENTED_EDGE ( 'NONE', *, *, #1752, .T. ) ;
#359 = CARTESIAN_POINT ( 'NONE',  ( -0.2073672225646059353, -17.02047435233534145, 19.56050940960062690 ) ) ;
#360 = AXIS2_PLACEMENT_3D ( 'NONE', #13665, #18184, #22851 ) ;
#361 = CARTESIAN_POINT ( 'NONE',  ( -23.13350093726293366, 11.03024450687078861, 49.37167574286524996 ) ) ;
#362 = CARTESIAN_POINT ( 'NONE',  ( -7.796062812047482637, -15.18940472835275202, 6.131018562779544823 ) ) ;
#363 = DIRECTION ( 'NONE',  ( -0.000000000000000000, -0.000000000000000000, 1.000000000000000000 ) ) ;
#364 = CARTESIAN_POINT ( 'NONE',  ( 1.771654956907828593, -16.98531529776322202, 19.58863275299554019 ) ) ;
#365 = ORIENTED_EDGE ( 'NONE', *, *, #16572, .F. ) ;
#366 = EDGE_CURVE ( 'NONE', #13283, #3383, #19165, .T. ) ;
#367 = CARTESIAN_POINT ( 'NONE',  ( 18.44250036706182883, -7.738792361249056562, 5.679672709359370408 ) ) ;
#368 = FACE_OUTER_BOUND ( 'NONE', #3082, .T. ) ;
#369 = CARTESIAN_POINT ( 'NONE',  ( 12.30438418247798538, 11.79938075381829066, 18.34838970509067479 ) ) ;
#370 = FACE_OUTER_BOUND ( 'NONE', #17110, .T. ) ;
#371 = AXIS2_PLACEMENT_3D ( 'NONE', #8358, #11002, #3982 ) ;
#372 = EDGE_LOOP ( 'NONE', ( #10343, #19396, #30364, #16527 ) ) ;
#373 = CIRCLE ( 'NONE', #4356, 0.9999999999999983347 ) ;
#374 = CIRCLE ( 'NONE', #21296, 0.7441270634457181066 ) ;
#375 = DIRECTION ( 'NONE',  ( 0.000000000000000000, 0.000000000000000000, -1.000000000000000000 ) ) ;
#376 = EDGE_CURVE ( 'NONE', #10212, #10205, #7649, .T. ) ;
#377 = CARTESIAN_POINT ( 'NONE',  ( -18.02600256144196322, -8.705149951716492751, 5.652605728828375753 ) ) ;
#378 = CARTESIAN_POINT ( 'NONE',  ( -6.670428619809865900, 18.87372120578243795, 5.951255046771932733 ) ) ;
#379 = CARTESIAN_POINT ( 'NONE',  ( -19.93457197822652205, 1.617270501065028565, 7.161525567826883432 ) ) ;
#380 = DIRECTION ( 'NONE',  ( 0.000000000000000000, 0.000000000000000000, 1.000000000000000000 ) ) ;
#381 = EDGE_CURVE ( 'NONE', #9423, #9573, #2631, .T. ) ;
#382 = CARTESIAN_POINT ( 'NONE',  ( -5.544451647051928944, 16.11829164193971664, 20.34789198813115263 ) ) ;
#383 = LINE ( 'NONE', #24396, #15077 ) ;
#384 = VECTOR ( 'NONE', #1530, 1000.000000000000000 ) ;
#385 = EDGE_LOOP ( 'NONE', ( #18527, #8717, #10000, #7620 ) ) ;
#386 = VERTEX_POINT ( 'NONE', #5599 ) ;
#387 = AXIS2_PLACEMENT_3D ( 'NONE', #10424, #20235, #11043 ) ;
#388 = FACE_OUTER_BOUND ( 'NONE', #26241, .T. ) ;
#389 = CARTESIAN_POINT ( 'NONE',  ( -5.000852292258041842, 19.36469665082833913, 19.47728749465736797 ) ) ;
#390 = CARTESIAN_POINT ( 'NONE',  ( 4.510281037539698445E-13, -4.926614671774132148E-13, 82.49999999999998579 ) ) ;
#391 = DIRECTION ( 'NONE',  ( 0.000000000000000000, 0.000000000000000000, 1.000000000000000000 ) ) ;
#392 = ORIENTED_EDGE ( 'NONE', *, *, #26901, .T. ) ;
#393 = PRODUCT_CONTEXT ( 'NONE', #13759, 'mechanical' ) ;
#394 = DIRECTION ( 'NONE',  ( 1.000000000000000000, 0.000000000000000000, -0.000000000000000000 ) ) ;
#395 = EDGE_CURVE ( 'NONE', #119, #19467, #10261, .T. ) ;
#396 = CYLINDRICAL_SURFACE ( 'NONE', #20666, 0.7500000000000006661 ) ;
#397 = ADVANCED_FACE ( 'NONE', ( #26495 ), #10383, .T. ) ;
#398 = ORIENTED_EDGE ( 'NONE', *, *, #13211, .T. ) ;
#399 = CARTESIAN_POINT ( 'NONE',  ( 5.016833900951455760, 16.26516650762552629, 19.45164628100866722 ) ) ;
#400 = AXIS2_PLACEMENT_3D ( 'NONE', #13486, #9091, #27970 ) ;
#401 = CARTESIAN_POINT ( 'NONE',  ( -33.78553954455730235, -24.40792764007751359, -16.50000000000000000 ) ) ;
#402 = VECTOR ( 'NONE', #2368, 1000.000000000000114 ) ;
#403 = CARTESIAN_POINT ( 'NONE',  ( 29.61203839202722676, 15.40012917324034092, 41.62281023987512185 ) ) ;
#404 = CARTESIAN_POINT ( 'NONE',  ( -34.20659985760524080, -15.57190080006868271, 37.50000000004849454 ) ) ;
#405 = ORIENTED_EDGE ( 'NONE', *, *, #28102, .T. ) ;
#406 = LINE ( 'NONE', #14743, #17330 ) ;
#407 = LINE ( 'NONE', #9924, #2084 ) ;
#408 = DIRECTION ( 'NONE',  ( -1.000000000000000000, 0.000000000000000000, 0.000000000000000000 ) ) ;
#409 = ORIENTED_EDGE ( 'NONE', *, *, #20131, .F. ) ;
#410 = CARTESIAN_POINT ( 'NONE',  ( -18.36135251343596764, -7.973951480934441172, 7.359006845440219102 ) ) ;
#411 = DIRECTION ( 'NONE',  ( 1.000000000000000000, 0.000000000000000000, 0.000000000000000000 ) ) ;
#412 = EDGE_CURVE ( 'NONE', #8092, #2167, #25816, .T. ) ;
#413 = CARTESIAN_POINT ( 'NONE',  ( 14.20332585465778941, 14.08077620357340720, 6.919864475265769421 ) ) ;
#414 = EDGE_CURVE ( 'NONE', #2072, #12805, #10900, .T. ) ;
#415 = CARTESIAN_POINT ( 'NONE',  ( -0.08542884365699662808, -20.01766063302414622, 5.749228751562096562 ) ) ;
#416 = FACE_OUTER_BOUND ( 'NONE', #4200, .T. ) ;
#417 = DIRECTION ( 'NONE',  ( 0.000000000000000000, -0.6368814469962913449, -0.7709617516270896864 ) ) ;
#418 = CARTESIAN_POINT ( 'NONE',  ( 37.99999999999999289, 70.00000000000000000, -40.50000000000000711 ) ) ;
#419 = CARTESIAN_POINT ( 'NONE',  ( -0.6237340761795794331, 8.999114229549594057, -3.621320343559650379 ) ) ;
#420 = ORIENTED_EDGE ( 'NONE', *, *, #14601, .T. ) ;
#421 = AXIS2_PLACEMENT_3D ( 'NONE', #28483, #11956, #16009 ) ;
#422 = ADVANCED_FACE ( 'NONE', ( #3565 ), #20954, .T. ) ;
#423 = AXIS2_PLACEMENT_3D ( 'NONE', #5251, #14749, #10546 ) ;
#424 = CARTESIAN_POINT ( 'NONE',  ( -7.869584159753960861, 10.39565510934976977, 1.500000000000001332 ) ) ;
#425 = CARTESIAN_POINT ( 'NONE',  ( 5.041560023644209743, 19.35451993181656860, 7.626218077512944227 ) ) ;
#426 = CIRCLE ( 'NONE', #4407, 0.7500000000000006661 ) ;
#427 = ORIENTED_EDGE ( 'NONE', *, *, #26367, .F. ) ;
#428 = ORIENTED_EDGE ( 'NONE', *, *, #24835, .F. ) ;
#429 = EDGE_CURVE ( 'NONE', #25490, #7103, #10636, .T. ) ;
#430 = CARTESIAN_POINT ( 'NONE',  ( -5.881244434206279514, -6.812559277181949646, -3.621320343559650379 ) ) ;
#431 = EDGE_CURVE ( 'NONE', #20799, #28201, #20243, .T. ) ;
#432 = PLANE ( 'NONE',  #5430 ) ;
#433 =( LENGTH_UNIT ( ) NAMED_UNIT ( * ) SI_UNIT ( .MILLI., .METRE. ) );
#434 = EDGE_LOOP ( 'NONE', ( #12928, #30003 ) ) ;
#435 = CARTESIAN_POINT ( 'NONE',  ( 15.37106698384762993, 12.82394120857654052, 20.05479082170252525 ) ) ;
#436 = EDGE_CURVE ( 'NONE', #11277, #20672, #12935, .T. ) ;
#437 = CARTESIAN_POINT ( 'NONE',  ( -11.28665222577991578, -16.53262428680031704, 6.211014596808754007 ) ) ;
#438 = VERTEX_POINT ( 'NONE', #18642 ) ;
#439 = CARTESIAN_POINT ( 'NONE',  ( 18.73437065802030332, -7.051821425362959417, 19.25672174529527325 ) ) ;
#440 = CARTESIAN_POINT ( 'NONE',  ( -15.42727847259664564, 12.72856271945105178, 20.34789198813115263 ) ) ;
#441 = CARTESIAN_POINT ( 'NONE',  ( -26.81381729043377504, 6.366069288663346093, 47.44085139292785414 ) ) ;
#442 = ORIENTED_EDGE ( 'NONE', *, *, #12082, .T. ) ;
#443 = DIRECTION ( 'NONE',  ( -0.000000000000000000, -0.000000000000000000, 1.000000000000000000 ) ) ;
#444 = ORIENTED_EDGE ( 'NONE', *, *, #11235, .F. ) ;
#445 = CARTESIAN_POINT ( 'NONE',  ( -50.00000000000000000, -50.00000000000000000, 97.07879600563551037 ) ) ;
#446 = AXIS2_PLACEMENT_3D ( 'NONE', #2104, #16459, #7100 ) ;
#447 = CIRCLE ( 'NONE', #17897, 9.000000000000000000 ) ;
#448 = ORIENTED_EDGE ( 'NONE', *, *, #24131, .T. ) ;
#449 = ADVANCED_FACE ( 'NONE', ( #17752 ), #28148, .F. ) ;
#450 = EDGE_CURVE ( 'NONE', #9427, #25685, #22270, .T. ) ;
#451 = CARTESIAN_POINT ( 'NONE',  ( 5.060094141397912360, 42.14075867279367316, 28.87075318537527835 ) ) ;
#452 = CARTESIAN_POINT ( 'NONE',  ( -6.485206790418931888, 15.79815780198024910, 19.58863275299554019 ) ) ;
#453 = CARTESIAN_POINT ( 'NONE',  ( -10.51100883930069863, -17.01524884273342053, 5.652196082369965069 ) ) ;
#454 = VECTOR ( 'NONE', #3159, 1000.000000000000000 ) ;
#455 = EDGE_CURVE ( 'NONE', #752, #3032, #6774, .T. ) ;
#456 = CARTESIAN_POINT ( 'NONE',  ( -7.857295329535767259, -15.15488436941561368, 18.73743063545763121 ) ) ;
#457 = CARTESIAN_POINT ( 'NONE',  ( -37.32236259411956780, 12.59516552021271885, 31.74041422182562755 ) ) ;
#458 = CARTESIAN_POINT ( 'NONE',  ( 11.23874228076938664, -11.06161525231356713, 24.50000000000000000 ) ) ;
#459 = CYLINDRICAL_SURFACE ( 'NONE', #7899, 0.7499999999999988898 ) ;
#460 = ORIENTED_EDGE ( 'NONE', *, *, #757, .T. ) ;
#461 = CARTESIAN_POINT ( 'NONE',  ( 9.833055564703258256, -13.92194044488497440, 5.651989602109218858 ) ) ;
#462 = CIRCLE ( 'NONE', #19386, 9.000000000000000000 ) ;
#463 = CARTESIAN_POINT ( 'NONE',  ( -28.06941827521502475, 29.50589912660750969, 12.07342606168410093 ) ) ;
#464 = CARTESIAN_POINT ( 'NONE',  ( -13.42620032052775692, 10.50496109755573748, 7.652108011868850035 ) ) ;
#465 = DIRECTION ( 'NONE',  ( 0.000000000000000000, -1.132880637372608986E-16, 1.000000000000000000 ) ) ;
#466 = VERTEX_POINT ( 'NONE', #10733 ) ;
#467 = ORIENTED_EDGE ( 'NONE', *, *, #5596, .F. ) ;
#468 = CYLINDRICAL_SURFACE ( 'NONE', #18787, 2.898871837527149165 ) ;
#469 = CARTESIAN_POINT ( 'NONE',  ( 8.752572334588121450, -2.431858781452763019, 13.22130136205108819 ) ) ;
#470 = CARTESIAN_POINT ( 'NONE',  ( 18.71829317531096137, -7.044536951825319804, 19.48477075383301482 ) ) ;
#471 = DIRECTION ( 'NONE',  ( -0.8910248307962437275, 0.4539545692076742966, 0.000000000000000000 ) ) ;
#472 = CARTESIAN_POINT ( 'NONE',  ( 7.856594496258195726, 4.390207617113981442, -3.621320343559650379 ) ) ;
#473 = ORIENTED_EDGE ( 'NONE', *, *, #21967, .F. ) ;
#474 = FACE_OUTER_BOUND ( 'NONE', #14568, .T. ) ;
#475 = PLANE ( 'NONE',  #11721 ) ;
#476 = CARTESIAN_POINT ( 'NONE',  ( 19.74251403343738076, 3.198927889078825970, 18.34798005863226678 ) ) ;
#477 = VERTEX_POINT ( 'NONE', #3410 ) ;
#478 = DIRECTION ( 'NONE',  ( 0.000000000000000000, 0.000000000000000000, 1.000000000000000000 ) ) ;
#479 = VERTEX_POINT ( 'NONE', #10583 ) ;
#480 = ADVANCED_FACE ( 'NONE', ( #29613 ), #1231, .F. ) ;
#481 = CYLINDRICAL_SURFACE ( 'NONE', #1478, 0.6002263538043648428 ) ;
#482 = EDGE_CURVE ( 'NONE', #4513, #14016, #6055, .T. ) ;
#483 = ADVANCED_FACE ( 'NONE', ( #14572 ), #23758, .T. ) ;
#484 = LINE ( 'NONE', #7511, #24812 ) ;
#485 = LINE ( 'NONE', #28719, #30455 ) ;
#486 = ORIENTED_EDGE ( 'NONE', *, *, #11751, .F. ) ;
#487 = CARTESIAN_POINT ( 'NONE',  ( 0.7220001660362483920, 9.454746441592963180, 21.50000000000000000 ) ) ;
#488 = CARTESIAN_POINT ( 'NONE',  ( -2.431858781452794993, -8.752572334588114344, 13.22130136205108641 ) ) ;
#489 = CARTESIAN_POINT ( 'NONE',  ( -7.749586724479453181, -2.959227181723774525, 21.50000000000000000 ) ) ;
#490 = CARTESIAN_POINT ( 'NONE',  ( 34.70577939417254498, 10.49309206032065944, 34.49999999999999289 ) ) ;
#491 = LINE ( 'NONE', #29032, #2354 ) ;
#492 = CARTESIAN_POINT ( 'NONE',  ( 30.03792366816882975, 15.52577997660843145, 41.18702913624200335 ) ) ;
#493 = ORIENTED_EDGE ( 'NONE', *, *, #4835, .T. ) ;
#494 = FACE_OUTER_BOUND ( 'NONE', #15914, .T. ) ;
#495 = CIRCLE ( 'NONE', #13480, 0.7500000000000006661 ) ;
#496 = CARTESIAN_POINT ( 'NONE',  ( -10.64374042650306862, 42.96126232887723972, -19.50000000000000355 ) ) ;
#497 = CARTESIAN_POINT ( 'NONE',  ( -1.000000000000008438, 19.97498435543819539, 24.50000000000000000 ) ) ;
#498 = VERTEX_POINT ( 'NONE', #7558 ) ;
#499 = CARTESIAN_POINT ( 'NONE',  ( -15.13309390500916862, -7.848982836665745921, 20.34789198813115263 ) ) ;
#500 = FACE_OUTER_BOUND ( 'NONE', #7541, .T. ) ;
#501 = CARTESIAN_POINT ( 'NONE',  ( -24.35970437652574105, -13.37404834226503070, 47.21042702067970254 ) ) ;
#502 = AXIS2_PLACEMENT_3D ( 'NONE', #13971, #30353, #16313 ) ;
#503 = CARTESIAN_POINT ( 'NONE',  ( -5.105024945673440229, 42.22604126506271172, -1.500000000000000000 ) ) ;
#504 = CARTESIAN_POINT ( 'NONE',  ( 3.196529495465388226, 8.413215745755008967, 21.50000000000000000 ) ) ;
#505 = CARTESIAN_POINT ( 'NONE',  ( 34.07302093592694803, 20.85404585400097233, 34.70738523996037372 ) ) ;
#506 = FACE_OUTER_BOUND ( 'NONE', #20914, .T. ) ;
#507 = ORIENTED_EDGE ( 'NONE', *, *, #26727, .T. ) ;
#508 = CARTESIAN_POINT ( 'NONE',  ( 0.000000000000000000, 7.794228634059944483, -4.500000000000004441 ) ) ;
#509 = VERTEX_POINT ( 'NONE', #21581 ) ;
#510 = CARTESIAN_POINT ( 'NONE',  ( -33.78553954455730235, -24.40792764007751359, -16.50000000000000000 ) ) ;
#511 = CARTESIAN_POINT ( 'NONE',  ( 0.8038475772933696417, 10.39230484541327471, -1.336447385876663028E-16 ) ) ;
#512 = ORIENTED_EDGE ( 'NONE', *, *, #14149, .F. ) ;
#513 = EDGE_LOOP ( 'NONE', ( #8393, #2746, #22053, #19738 ) ) ;
#514 = CARTESIAN_POINT ( 'NONE',  ( 9.216505592218814158, -7.781333699927420966, -1.500000000000000000 ) ) ;
#515 = CIRCLE ( 'NONE', #3019, 9.482273699623480212 ) ;
#516 = ORIENTED_EDGE ( 'NONE', *, *, #6379, .T. ) ;
#517 = ORIENTED_EDGE ( 'NONE', *, *, #25356, .F. ) ;
#518 = FACE_OUTER_BOUND ( 'NONE', #7310, .T. ) ;
#519 = CARTESIAN_POINT ( 'NONE',  ( -10.95918588188520282, 37.64010906258869227, 34.49999999999998579 ) ) ;
#520 = CARTESIAN_POINT ( 'NONE',  ( 3.993622308618881789, 8.159193615868410632, 13.22130136205108997 ) ) ;
#521 = ORIENTED_EDGE ( 'NONE', *, *, #17753, .F. ) ;
#522 = CARTESIAN_POINT ( 'NONE',  ( -24.03057240117690441, -26.57182937991348481, -6.499999999999999112 ) ) ;
#523 = CARTESIAN_POINT ( 'NONE',  ( 24.44496207165490276, 7.595930209050162141, -16.55003854064094426 ) ) ;
#524 = CARTESIAN_POINT ( 'NONE',  ( 14.19872765237045442, 14.11031447301239972, 19.36813350477385143 ) ) ;
#525 = DIRECTION ( 'NONE',  ( -0.000000000000000000, -0.000000000000000000, 1.000000000000000000 ) ) ;
#526 = VERTEX_POINT ( 'NONE', #217 ) ;
#527 = DIRECTION ( 'NONE',  ( -1.000000000000000000, 0.000000000000000000, -0.000000000000000000 ) ) ;
#528 = FACE_OUTER_BOUND ( 'NONE', #3439, .T. ) ;
#529 = CARTESIAN_POINT ( 'NONE',  ( -6.227270323482350101, 15.89124769393590952, 7.366751648393900176 ) ) ;
#530 = CARTESIAN_POINT ( 'NONE',  ( -19.85983307072121917, 2.367331911061644867, 7.652108011868850923 ) ) ;
#531 = CARTESIAN_POINT ( 'NONE',  ( -18.41388790264795361, -7.851569931599773788, 18.80699882434806369 ) ) ;
#532 = AXIS2_PLACEMENT_3D ( 'NONE', #23516, #28832, #23662 ) ;
#533 = PLANE ( 'NONE',  #14075 ) ;
#534 = ORIENTED_EDGE ( 'NONE', *, *, #649, .F. ) ;
#535 = EDGE_LOOP ( 'NONE', ( #1765, #22234, #5440, #4015 ) ) ;
#536 = CARTESIAN_POINT ( 'NONE',  ( 7.856594496258195726, 4.390207617113981442, 21.50000000000000000 ) ) ;
#537 = CARTESIAN_POINT ( 'NONE',  ( -5.971396161871752817, 19.08775596758252036, 20.34789198813115263 ) ) ;
#538 = CARTESIAN_POINT ( 'NONE',  ( -14.93957691572895818, 13.32381478560234456, 7.429667576816606278 ) ) ;
#539 = CARTESIAN_POINT ( 'NONE',  ( 0.7788148816922453310, -17.02744011591805062, 7.652108011868850923 ) ) ;
#540 = VERTEX_POINT ( 'NONE', #28613 ) ;
#541 = APPLICATION_PROTOCOL_DEFINITION ( 'draft international standard', 'automotive_design', 1998, #5195 ) ;
#542 = CARTESIAN_POINT ( 'NONE',  ( 18.26182835180409825, -8.199456719779961489, 18.36582235739946611 ) ) ;
#543 = CARTESIAN_POINT ( 'NONE',  ( -3.914781618004754105, -8.197313248159934673, 13.22130136205108641 ) ) ;
#544 = VERTEX_POINT ( 'NONE', #30627 ) ;
#545 = CARTESIAN_POINT ( 'NONE',  ( 5.278755796068665518, 7.392982946727100213, 13.22130136205108819 ) ) ;
#546 = CARTESIAN_POINT ( 'NONE',  ( -33.57242512144540569, -24.08458161880429316, -13.16663720046962816 ) ) ;
#547 = CARTESIAN_POINT ( 'NONE',  ( -42.49999999999998579, -50.00000000000000000, -87.50000000000000000 ) ) ;
#548 = CARTESIAN_POINT ( 'NONE',  ( -32.31395967786516366, -23.80510233529698993, 30.69444703814347264 ) ) ;
#549 = VERTEX_POINT ( 'NONE', #2245 ) ;
#550 = CARTESIAN_POINT ( 'NONE',  ( -18.04156136322729864, -8.631457789788587576, 5.652196082369963293 ) ) ;
#551 = EDGE_CURVE ( 'NONE', #10953, #254, #7134, .T. ) ;
#552 = ADVANCED_FACE ( 'NONE', ( #7235 ), #23923, .F. ) ;
#553 = CIRCLE ( 'NONE', #9509, 9.482273699623480212 ) ;
#554 = CARTESIAN_POINT ( 'NONE',  ( 4.608906612435600181, 7.730328572437758616, 1.500000000000001332 ) ) ;
#555 = FACE_OUTER_BOUND ( 'NONE', #28008, .T. ) ;
#556 = ORIENTED_EDGE ( 'NONE', *, *, #19301, .T. ) ;
#557 = DIRECTION ( 'NONE',  ( 0.000000000000000000, -1.132880637372608986E-16, 1.000000000000000000 ) ) ;
#558 = LINE ( 'NONE', #12121, #27803 ) ;
#559 = FACE_BOUND ( 'NONE', #17141, .T. ) ;
#560 = CARTESIAN_POINT ( 'NONE',  ( -0.2365265214052943432, -17.01953242238517916, 6.641371103590088865 ) ) ;
#561 = CARTESIAN_POINT ( 'NONE',  ( -17.20435420003449423, -1.463329469628170898, -0.6213203435596476032 ) ) ;
#562 = DIRECTION ( 'NONE',  ( 0.000000000000000000, 0.000000000000000000, 1.000000000000000000 ) ) ;
#563 = CARTESIAN_POINT ( 'NONE',  ( -50.00000000000000000, 50.00000000000000000, 12.49999999999999112 ) ) ;
#564 = DIRECTION ( 'NONE',  ( -0.000000000000000000, 1.132880637372608986E-16, -1.000000000000000000 ) ) ;
#565 = ORIENTED_EDGE ( 'NONE', *, *, #7868, .T. ) ;
#566 = AXIS2_PLACEMENT_3D ( 'NONE', #22892, #22733, #8869 ) ;
#567 = DIRECTION ( 'NONE',  ( -0.000000000000000000, -0.000000000000000000, -1.000000000000000000 ) ) ;
#568 = LINE ( 'NONE', #26949, #28027 ) ;
#569 = ORIENTED_EDGE ( 'NONE', *, *, #16803, .T. ) ;
#570 = ORIENTED_EDGE ( 'NONE', *, *, #6962, .T. ) ;
#571 = CARTESIAN_POINT ( 'NONE',  ( 25.47847050916411504, 26.57182937991349903, -6.499999999999999112 ) ) ;
#572 = CARTESIAN_POINT ( 'NONE',  ( -14.87817005273856985, 47.73513060975979982, -56.97185882095643450 ) ) ;
#573 = ORIENTED_EDGE ( 'NONE', *, *, #29979, .F. ) ;
#574 = ADVANCED_BREP_SHAPE_REPRESENTATION ( '', ( #2768, #7396 ), #910 ) ;
#575 = EDGE_CURVE ( 'NONE', #3557, #18473, #9892, .T. ) ;
#576 = CIRCLE ( 'NONE', #3574, 0.7500000000000006661 ) ;
#577 = CARTESIAN_POINT ( 'NONE',  ( 12.83215063165194891, 11.19227874472585782, 20.05479082170252525 ) ) ;
#578 = EDGE_CURVE ( 'NONE', #11969, #7607, #20097, .T. ) ;
#579 = CARTESIAN_POINT ( 'NONE',  ( -11.35279153858833112, -16.48728705952963480, 6.864725433338323413 ) ) ;
#580 = VERTEX_POINT ( 'NONE', #9273 ) ;
#581 = CARTESIAN_POINT ( 'NONE',  ( 18.72830449397920560, -7.068013160879066170, 19.14333282897057842 ) ) ;
#582 = DIRECTION ( 'NONE',  ( -1.000000000000000000, 0.000000000000000000, 0.000000000000000000 ) ) ;
#583 = DIRECTION ( 'NONE',  ( -0.000000000000000000, -0.000000000000000000, 1.000000000000000000 ) ) ;
#584 = VERTEX_POINT ( 'NONE', #5059 ) ;
#585 = DIRECTION ( 'NONE',  ( 0.000000000000000000, 0.000000000000000000, -1.000000000000000000 ) ) ;
#586 = ADVANCED_FACE ( 'NONE', ( #19241 ), #28765, .F. ) ;
#587 = EDGE_CURVE ( 'NONE', #12561, #19716, #26583, .T. ) ;
#588 = AXIS2_PLACEMENT_3D ( 'NONE', #26078, #13640, #11903 ) ;
#589 = ORIENTED_EDGE ( 'NONE', *, *, #10348, .F. ) ;
#590 = EDGE_CURVE ( 'NONE', #23467, #4066, #18123, .T. ) ;
#591 = CARTESIAN_POINT ( 'NONE',  ( 35.02974205252522211, 18.72736911740413746, 31.20071108243496738 ) ) ;
#592 = CARTESIAN_POINT ( 'NONE',  ( -6.227270323482350989, 15.89124769393590597, 20.06253562465620632 ) ) ;
#593 = CARTESIAN_POINT ( 'NONE',  ( -14.83674576813424295, 13.43848929326658492, 18.71435384576123440 ) ) ;
#594 = CIRCLE ( 'NONE', #15544, 9.084132297865673777 ) ;
#595 = ADVANCED_FACE ( 'NONE', ( #370 ), #16451, .F. ) ;
#596 = CARTESIAN_POINT ( 'NONE',  ( -13.00999358272542494, -0.8602714556717691030, 24.50000000000000000 ) ) ;
#597 = ADVANCED_FACE ( 'NONE', ( #17058 ), #18881, .F. ) ;
#598 = CARTESIAN_POINT ( 'NONE',  ( -19.51604255644980412, 36.82188910226315670, 29.35984054749004102 ) ) ;
#599 = CARTESIAN_POINT ( 'NONE',  ( -16.96556290498877573, 1.647560670993253540, 5.652196082368482699 ) ) ;
#600 = PLANE ( 'NONE',  #26319 ) ;
#601 = ORIENTED_EDGE ( 'NONE', *, *, #19478, .T. ) ;
#603 = B_SPLINE_CURVE_WITH_KNOTS ( 'NONE', 3,
 ( #9449, #13968, #2105, #21117 ),
 .UNSPECIFIED., .F., .F.,
 ( 4, 4 ),
 ( 0.002976194933398900420, 0.003711256114093792156 ),
 .UNSPECIFIED. ) ;
#602 = CARTESIAN_POINT ( 'NONE',  ( 11.02326084422093189, -16.70928013427648651, 5.657991946698900598 ) ) ;
#604 = CARTESIAN_POINT ( 'NONE',  ( 0.000000000000000000, -1.324687536737320328E-14, 29.43090101791767665 ) ) ;
#605 = CARTESIAN_POINT ( 'NONE',  ( 9.013259606643902799, -14.43917691233135869, 6.782064869129510676 ) ) ;
#606 = VERTEX_POINT ( 'NONE', #11765 ) ;
#607 = ORIENTED_EDGE ( 'NONE', *, *, #11130, .F. ) ;
#608 = CARTESIAN_POINT ( 'NONE',  ( 0.000000000000000000, -2.435693370351110282E-15, 21.50000000000000355 ) ) ;
#609 = CARTESIAN_POINT ( 'NONE',  ( 10.58932223943305573, -16.96688107778387078, 5.849008070840548079 ) ) ;
#610 = AXIS2_PLACEMENT_3D ( 'NONE', #14293, #4786, #30528 ) ;
#611 = LINE ( 'NONE', #7792, #3910 ) ;
#612 = CARTESIAN_POINT ( 'NONE',  ( -15.57738559309033022, -6.860713375568460393, 6.714907520933425467 ) ) ;
#613 = CARTESIAN_POINT ( 'NONE',  ( -4.100931858250860707, -19.90478481566557534, 1.500000000000000000 ) ) ;
#614 = ADVANCED_FACE ( 'NONE', ( #28465 ), #16596, .F. ) ;
#615 = CARTESIAN_POINT ( 'NONE',  ( 1.000000000000008438, 13.00000000000001421, 1.500000000000001332 ) ) ;
#616 = ORIENTED_EDGE ( 'NONE', *, *, #19676, .F. ) ;
#617 = EDGE_CURVE ( 'NONE', #17587, #16446, #72, .T. ) ;
#618 = CARTESIAN_POINT ( 'NONE',  ( 0.000000000000000000, 0.000000000000000000, 0.000000000000000000 ) ) ;
#619 = CARTESIAN_POINT ( 'NONE',  ( -17.67829152986844932, -9.353438168054493573, 18.73377938172347612 ) ) ;
#620 = EDGE_CURVE ( 'NONE', #21542, #7918, #19871, .T. ) ;
#621 = CARTESIAN_POINT ( 'NONE',  ( 19.77852387640474419, 3.085824932809442700, 5.657991946698900598 ) ) ;
#622 = ORIENTED_EDGE ( 'NONE', *, *, #14546, .F. ) ;
#623 = CARTESIAN_POINT ( 'NONE',  ( 15.53918631077679002, 12.61944498292910488, 6.420335371522007506 ) ) ;
#624 = VERTEX_POINT ( 'NONE', #8174 ) ;
#625 = CARTESIAN_POINT ( 'NONE',  ( 16.02044690728356002, -5.868896442471958963, 7.500147780736496017 ) ) ;
#626 = ADVANCED_FACE ( 'NONE', ( #10658 ), #17680, .F. ) ;
#627 = FACE_OUTER_BOUND ( 'NONE', #19855, .T. ) ;
#628 = CARTESIAN_POINT ( 'NONE',  ( -38.00000000000000711, 80.00000000000000000, 47.91742430504431383 ) ) ;
#629 = ORIENTED_EDGE ( 'NONE', *, *, #8754, .F. ) ;
#630 = VECTOR ( 'NONE', #11453, 1000.000000000000000 ) ;
#631 = VECTOR ( 'NONE', #12349, 1000.000000000000000 ) ;
#632 = ADVANCED_FACE ( 'NONE', ( #17214 ), #5675, .F. ) ;
#633 = LINE ( 'NONE', #12185, #27245 ) ;
#634 = AXIS2_PLACEMENT_3D ( 'NONE', #23126, #15969, #13490 ) ;
#635 = DIRECTION ( 'NONE',  ( -0.000000000000000000, -1.000000000000000000, -0.000000000000000000 ) ) ;
#636 = LINE ( 'NONE', #3142, #22778 ) ;
#637 = CARTESIAN_POINT ( 'NONE',  ( -0.9307681286967850465, 9.436481611552762772, 21.50000000000000000 ) ) ;
#638 = B_SPLINE_CURVE_WITH_KNOTS ( 'NONE', 3,
 ( #10726, #17744, #5592, #22265, #17916, #1379, #29923, #19940, #29760, #20545, #30064, #27580, #15559, #5738, #25226, #3871, #15086, #13394, #22884, #24604 ),
 .UNSPECIFIED., .F., .F.,
 ( 4, 2, 2, 2, 2, 2, 2, 2, 2, 4 ),
 ( 0.000000000000000000, 0.06250000000000163758, 0.1250000000000032752, 0.1875000000000049127, 0.2187500000000050793, 0.2500000000000052180, 0.3125000000000038858, 0.3750000000000024980, 0.4375000000000011657, 0.4999999999999999445 ),
 .UNSPECIFIED. ) ;
#639 = CARTESIAN_POINT ( 'NONE',  ( -34.70577939417217550, -10.49309206032214270, 34.49999999999999289 ) ) ;
#640 = DIRECTION ( 'NONE',  ( 1.000000000000000000, 0.000000000000000000, 4.565061778886335400E-17 ) ) ;
#641 = CARTESIAN_POINT ( 'NONE',  ( 33.50775388423620882, 10.82565592554877121, 39.78708271175815270 ) ) ;
#642 = ORIENTED_EDGE ( 'NONE', *, *, #3488, .T. ) ;
#643 = CARTESIAN_POINT ( 'NONE',  ( 26.12638453225886792, 6.310846377660611850, 48.12226976367801257 ) ) ;
#644 = CARTESIAN_POINT ( 'NONE',  ( -13.66451197432776965, 10.21236830578559918, 18.44527579819791185 ) ) ;
#645 = CARTESIAN_POINT ( 'NONE',  ( -26.80246859415415273, 7.028748154183637631, -1.499999999999999556 ) ) ;
#646 = ORIENTED_EDGE ( 'NONE', *, *, #6616, .F. ) ;
#647 = CARTESIAN_POINT ( 'NONE',  ( 30.67761959283033235, -26.24282937179839337, 17.43639551542309718 ) ) ;
#648 = CARTESIAN_POINT ( 'NONE',  ( -37.16608720827707657, 51.86186943028246787, 57.49999999999999289 ) ) ;
#649 = EDGE_CURVE ( 'NONE', #21864, #12141, #26737, .T. ) ;
#650 = CARTESIAN_POINT ( 'NONE',  ( 0.000000000000000000, 12.49999999999999289, -16.50000000000000000 ) ) ;
#651 = CARTESIAN_POINT ( 'NONE',  ( 8.499586724479435418, 2.959227181723830036, 21.50000000000000000 ) ) ;
#652 = EDGE_CURVE ( 'NONE', #15421, #2309, #4171, .T. ) ;
#653 = CARTESIAN_POINT ( 'NONE',  ( -39.00000000000000000, 5.563236990218665134, -1.500000000000000000 ) ) ;
#654 = CARTESIAN_POINT ( 'NONE',  ( -23.21352257770656990, 10.78826658734919519, 45.15942333309111234 ) ) ;
#655 = AXIS2_PLACEMENT_3D ( 'NONE', #16975, #24609, #740 ) ;
#656 = DIRECTION ( 'NONE',  ( -0.000000000000000000, 1.000000000000000000, -0.000000000000000000 ) ) ;
#658 = CIRCLE ( 'NONE', #6650, 0.7500000000000006661 ) ;
#657 = LINE ( 'NONE', #10172, #27987 ) ;
#659 = ORIENTED_EDGE ( 'NONE', *, *, #21172, .T. ) ;
#660 = FACE_OUTER_BOUND ( 'NONE', #25257, .T. ) ;
#661 = ORIENTED_EDGE ( 'NONE', *, *, #1590, .T. ) ;
#662 = LINE ( 'NONE', #10032, #18671 ) ;
#663 = CARTESIAN_POINT ( 'NONE',  ( -43.34097750826428097, -11.89502811014147987, -1.500000000000000444 ) ) ;
#664 = ORIENTED_EDGE ( 'NONE', *, *, #18976, .F. ) ;
#665 = ORIENTED_EDGE ( 'NONE', *, *, #13448, .F. ) ;
#666 = CARTESIAN_POINT ( 'NONE',  ( -17.26937953831790651, 14.36006998371489551, -1.500000000000000000 ) ) ;
#667 = EDGE_LOOP ( 'NONE', ( #2923, #26532 ) ) ;
#668 = ORIENTED_EDGE ( 'NONE', *, *, #12074, .F. ) ;
#669 = EDGE_LOOP ( 'NONE', ( #23306, #14404 ) ) ;
#670 = CARTESIAN_POINT ( 'NONE',  ( 0.7453234696411419336, -17.02803278171227674, 18.34777357837151968 ) ) ;
#671 = DIRECTION ( 'NONE',  ( 0.000000000000000000, 0.000000000000000000, -1.000000000000000000 ) ) ;
#672 = DIRECTION ( 'NONE',  ( 0.000000000000000000, 0.000000000000000000, 1.000000000000000000 ) ) ;
#673 = AXIS2_PLACEMENT_3D ( 'NONE', #16914, #18794, #7091 ) ;
#674 = CARTESIAN_POINT ( 'NONE',  ( -35.78636641679163688, 16.94032250535760653, 17.18098098232441018 ) ) ;
#675 = DIRECTION ( 'NONE',  ( 0.000000000000000000, 0.000000000000000000, 1.000000000000000000 ) ) ;
#676 = ORIENTED_EDGE ( 'NONE', *, *, #21813, .T. ) ;
#677 = DIRECTION ( 'NONE',  ( 0.000000000000000000, 1.000000000000000000, 0.000000000000000000 ) ) ;
#678 = CARTESIAN_POINT ( 'NONE',  ( 8.884323311075775109, 1.438332125858202692, 1.500000000000001332 ) ) ;
#679 = CARTESIAN_POINT ( 'NONE',  ( 14.74830145734719089, 13.53506178006322891, 20.32367522806703874 ) ) ;
#680 = DIRECTION ( 'NONE',  ( 1.000000000000000000, 0.000000000000000000, -0.000000000000000000 ) ) ;
#681 = VERTEX_POINT ( 'NONE', #999 ) ;
#682 = LINE ( 'NONE', #19245, #27844 ) ;
#683 = DIRECTION ( 'NONE',  ( 1.000000000000000000, 0.000000000000000000, -0.000000000000000000 ) ) ;
#684 = CARTESIAN_POINT ( 'NONE',  ( -6.938992678473721476, 18.77645360485809789, 6.560937769032974209 ) ) ;
#685 = CARTESIAN_POINT ( 'NONE',  ( 11.39819190923272707, -16.45610177916887551, 5.704143890883081269 ) ) ;
#686 = FACE_OUTER_BOUND ( 'NONE', #13708, .T. ) ;
#687 = CARTESIAN_POINT ( 'NONE',  ( 69.99999999999998579, 50.00000000000000000, 12.49999999999999112 ) ) ;
#688 = EDGE_LOOP ( 'NONE', ( #7959, #30091, #6151, #14785 ) ) ;
#689 = ORIENTED_EDGE ( 'NONE', *, *, #21785, .F. ) ;
#690 = LINE ( 'NONE', #10519, #25476 ) ;
#691 = ADVANCED_FACE ( 'NONE', ( #10356 ), #20168, .F. ) ;
#692 = CARTESIAN_POINT ( 'NONE',  ( -14.74940038399478581, 13.53421240139457815, 7.080843742048788414 ) ) ;
#693 = CARTESIAN_POINT ( 'NONE',  ( 35.00000000000000000, 90.00000000000001421, -22.50000000000002487 ) ) ;
#694 = EDGE_LOOP ( 'NONE', ( #14179, #5997 ) ) ;
#695 = ITEM_DEFINED_TRANSFORMATION ( 'NONE', 'NONE', #421,  #7396 ) ;
#696 = DIRECTION ( 'NONE',  ( -0.9096319953545185522, 0.4154150130018859355, 0.000000000000000000 ) ) ;
#697 = CARTESIAN_POINT ( 'NONE',  ( 4.045241160018716364, 16.55840174602107595, 5.652196082367002106 ) ) ;
#698 = AXIS2_PLACEMENT_3D ( 'NONE', #25372, #25055, #15689 ) ;
#699 = VERTEX_POINT ( 'NONE', #22362 ) ;
#700 = B_SPLINE_CURVE_WITH_KNOTS ( 'NONE', 3,
 ( #539, #9908, #28941, #10375, #29405, #8043, #19573, #24706, #22379, #17544, #10211, #12880, #15348, #17078, #3348, #1015, #7576, #26756, #29090, #24878 ),
 .UNSPECIFIED., .F., .F.,
 ( 4, 2, 2, 2, 2, 2, 2, 2, 2, 4 ),
 ( 0.000000000000000000, 0.06249999999999977102, 0.1249999999999995420, 0.1874999999999993061, 0.2187499999999992228, 0.2499999999999990841, 0.3124999999999992228, 0.3749999999999993894, 0.4374999999999995559, 0.4999999999999997224 ),
 .UNSPECIFIED. ) ;
#701 = CARTESIAN_POINT ( 'NONE',  ( -1.073881485057738949, 0.9711784013061123266, -1.500000000000000000 ) ) ;
#702 = FACE_OUTER_BOUND ( 'NONE', #5275, .T. ) ;
#703 = CARTESIAN_POINT ( 'NONE',  ( 26.36764545593177544, -31.31467416275353344, -1.500000000000000000 ) ) ;
#704 = CARTESIAN_POINT ( 'NONE',  ( -23.18616900178304974, -34.18096212676299217, 29.62072393548881877 ) ) ;
#705 = ORIENTED_EDGE ( 'NONE', *, *, #22488, .F. ) ;
#706 = CARTESIAN_POINT ( 'NONE',  ( 24.03057240117691862, -26.57182937991349903, 1.500000000000000000 ) ) ;
#707 = PLANE ( 'NONE',  #25288 ) ;
#708 = DIRECTION ( 'NONE',  ( 1.000000000000000000, 0.000000000000000000, 0.000000000000000000 ) ) ;
#709 = ORIENTED_EDGE ( 'NONE', *, *, #2670, .T. ) ;
#710 = CARTESIAN_POINT ( 'NONE',  ( 0.8750451464062524165, 9.041888939645138734, 13.22130136205108997 ) ) ;
#711 = B_SPLINE_SURFACE_WITH_KNOTS ( 'NONE', 3, 1, ( 
 ( #29500, #24966 ),
 ( #10153, #22316 ),
 ( #12970, #26861 ),
 ( #19658, #19825 ),
 ( #29347, #17492 ),
 ( #14986, #8137 ),
 ( #24498, #17804 ),
 ( #8288, #19982 ),
 ( #27013, #3144 ),
 ( #22160, #10468 ),
 ( #22462, #1109 ),
 ( #3602, #784 ),
 ( #13124, #18259 ),
 ( #11231, #13728 ),
 ( #25438, #4063 ),
 ( #25586, #13590 ),
 ( #6246, #3761 ),
 ( #8739, #20888 ),
 ( #1268, #1716 ),
 ( #28075, #25729 ),
 ( #13882, #4358 ),
 ( #11397, #10776 ),
 ( #4204, #20290 ),
 ( #29817, #23067 ),
 ( #8905, #23219 ),
 ( #1579, #27470 ),
 ( #11086, #8459 ),
 ( #17959, #22774 ),
 ( #15601, #25119 ),
 ( #18429, #1873 ),
 ( #8599, #18107 ),
 ( #30107, #3924 ),
 ( #27622, #15755 ),
 ( #25276, #20582 ) ),
 .UNSPECIFIED., .F., .F., .F.,
 ( 4, 2, 2, 2, 2, 2, 2, 2, 2, 2, 2, 2, 2, 2, 2, 2, 4 ),
 ( 2, 2 ),
 ( 0.000000000000000000, 0.06250000000000008327, 0.1250000000000001388, 0.1875000000000001943, 0.2500000000000002220, 0.3125000000000002220, 0.3750000000000002776, 0.4375000000000002776, 0.5000000000000003331, 0.5625000000000003331, 0.6250000000000002220, 0.6875000000000002220, 0.7500000000000002220, 0.8125000000000002220, 0.8750000000000001110, 0.9375000000000001110, 1.000000000000000000 ),
 ( 0.000000000000000000, 1.000000000000000000 ),
 .UNSPECIFIED. ) ;
#712 = DIRECTION ( 'NONE',  ( 0.000000000000000000, -0.000000000000000000, 1.000000000000000000 ) ) ;
#713 = CARTESIAN_POINT ( 'NONE',  ( 0.000000000000000000, 0.000000000000000000, -87.50000000000000000 ) ) ;
#714 = LINE ( 'NONE', #29114, #23280 ) ;
#715 = VECTOR ( 'NONE', #27913, 1000.000000000000000 ) ;
#716 = CARTESIAN_POINT ( 'NONE',  ( 32.98805937973595093, -22.67054169308931222, 8.000000000000003553 ) ) ;
#717 = DIRECTION ( 'NONE',  ( -0.000000000000000000, -0.000000000000000000, -1.000000000000000000 ) ) ;
#718 = ORIENTED_EDGE ( 'NONE', *, *, #23326, .F. ) ;
#719 = DIRECTION ( 'NONE',  ( -1.000000000000000000, 1.224646799147308341E-16, 0.000000000000000000 ) ) ;
#720 = CARTESIAN_POINT ( 'NONE',  ( 5.296161872597630271, 19.28602264385381204, 7.652108011868850035 ) ) ;
#721 = ADVANCED_FACE ( 'NONE', ( #3498 ), #3184, .T. ) ;
#722 = EDGE_LOOP ( 'NONE', ( #5355, #17765, #14254, #19084 ) ) ;
#723 = ORIENTED_EDGE ( 'NONE', *, *, #19288, .F. ) ;
#724 = DIRECTION ( 'NONE',  ( -1.000000000000000000, 0.000000000000000000, 0.000000000000000000 ) ) ;
#725 = CARTESIAN_POINT ( 'NONE',  ( -1.687027447297492211, -8.840471615930066918, 1.500000000000001332 ) ) ;
#726 = ORIENTED_EDGE ( 'NONE', *, *, #23506, .T. ) ;
#727 = CARTESIAN_POINT ( 'NONE',  ( -1.248051566150084613, -39.49999999999997158, 27.49999999999999289 ) ) ;
#728 = CARTESIAN_POINT ( 'NONE',  ( 15.04472583903954153, 13.20536594261729491, 18.36582235739946611 ) ) ;
#729 = ORIENTED_EDGE ( 'NONE', *, *, #10664, .F. ) ;
#730 = PLANE ( 'NONE',  #331 ) ;
#731 = PLANE ( 'NONE',  #2299 ) ;
#732 = CARTESIAN_POINT ( 'NONE',  ( 40.35867887216814864, 4.697862823546318012, -16.50000000000000000 ) ) ;
#733 =( BOUNDED_CURVE ( )  B_SPLINE_CURVE ( 3, ( #29605, #26969, #8239, #8560 ),
 .UNSPECIFIED., .F., .T. ) 
 B_SPLINE_CURVE_WITH_KNOTS ( ( 4, 4 ),
 ( 3.955359442064654285, 5.469418518704724619 ),
 .UNSPECIFIED. ) 
 CURVE ( )  GEOMETRIC_REPRESENTATION_ITEM ( )  RATIONAL_B_SPLINE_CURVE ( ( 1.000000000000000000, 0.8179194830933629312, 0.8179194830933629312, 1.000000000000000000 ) ) 
 REPRESENTATION_ITEM ( '' )  );
#734 = ORIENTED_EDGE ( 'NONE', *, *, #10715, .F. ) ;
#735 = CARTESIAN_POINT ( 'NONE',  ( -4.163336342344337027E-14, 1.387778780781445676E-14, 24.50000000000000000 ) ) ;
#736 = AXIS2_PLACEMENT_3D ( 'NONE', #3166, #5043, #14695 ) ;
#737 = ORIENTED_EDGE ( 'NONE', *, *, #28020, .T. ) ;
#738 = CARTESIAN_POINT ( 'NONE',  ( 0.000000000000000000, 39.50000000000000000, 27.50000000000000355 ) ) ;
#739 = ORIENTED_EDGE ( 'NONE', *, *, #127, .T. ) ;
#740 = DIRECTION ( 'NONE',  ( 0.000000000000000000, 0.000000000000000000, -1.000000000000000000 ) ) ;
#741 = CARTESIAN_POINT ( 'NONE',  ( 16.55484456677776706, 4.196195780087079719, 6.560937769032974209 ) ) ;
#742 = CARTESIAN_POINT ( 'NONE',  ( -6.974883619896829146, -5.687793815610328707, 21.50000000000000000 ) ) ;
#743 = DIRECTION ( 'NONE',  ( 0.000000000000000000, -1.132880637372608986E-16, 1.000000000000000000 ) ) ;
#744 = CARTESIAN_POINT ( 'NONE',  ( -27.80440265630350538, 29.80991922482741785, 30.06891749665959779 ) ) ;
#745 = CARTESIAN_POINT ( 'NONE',  ( 77.99999999999998579, 42.50000000000000711, 27.50000000000000711 ) ) ;
#746 = FACE_OUTER_BOUND ( 'NONE', #4867, .T. ) ;
#747 = ORIENTED_EDGE ( 'NONE', *, *, #23123, .T. ) ;
#748 = CARTESIAN_POINT ( 'NONE',  ( 9.027514758752763768, -14.43064536408543219, 6.864725433338323413 ) ) ;
#749 = CARTESIAN_POINT ( 'NONE',  ( 27.81206575847386375, -25.09777039261014053, 34.50000000000000711 ) ) ;
#750 = FACE_OUTER_BOUND ( 'NONE', #9838, .T. ) ;
#751 = ADVANCED_FACE ( 'NONE', ( #22199 ), #1146, .F. ) ;
#752 = VERTEX_POINT ( 'NONE', #835 ) ;
#753 = ORIENTED_EDGE ( 'NONE', *, *, #1735, .F. ) ;
#754 = AXIS2_PLACEMENT_3D ( 'NONE', #13903, #20910, #9218 ) ;
#755 = DIRECTION ( 'NONE',  ( -0.9096319953545185522, 0.4154150130018859355, 0.000000000000000000 ) ) ;
#756 = DIRECTION ( 'NONE',  ( 0.000000000000000000, 0.000000000000000000, -1.000000000000000000 ) ) ;
#757 = EDGE_CURVE ( 'NONE', #25122, #2838, #4153, .T. ) ;
#758 = DIRECTION ( 'NONE',  ( 0.000000000000000000, 0.000000000000000000, -1.000000000000000000 ) ) ;
#759 = ORIENTED_EDGE ( 'NONE', *, *, #25056, .T. ) ;
#760 = CARTESIAN_POINT ( 'NONE',  ( 12.35846533491531041, 11.73919094685904696, 7.652108011868850923 ) ) ;
#761 = CARTESIAN_POINT ( 'NONE',  ( -67.00000000000000000, -50.00000000000000000, 62.49999999999999289 ) ) ;
#762 = CARTESIAN_POINT ( 'NONE',  ( -31.45274955327688460, -26.35877938677512233, -8.166661938620272565 ) ) ;
#763 = ORIENTED_EDGE ( 'NONE', *, *, #27893, .T. ) ;
#764 = CARTESIAN_POINT ( 'NONE',  ( -9.636724589035640776, -17.52522580332708557, 19.48477075383299706 ) ) ;
#765 = ADVANCED_FACE ( 'NONE', ( #29389 ), #24224, .F. ) ;
#766 = PRESENTATION_LAYER_ASSIGNMENT (  '', '', ( #27682 ) ) ;
#767 = DIRECTION ( 'NONE',  ( 0.000000000000000000, 1.132880637372608986E-16, -1.000000000000000000 ) ) ;
#768 = FACE_OUTER_BOUND ( 'NONE', #4197, .T. ) ;
#769 = ORIENTED_EDGE ( 'NONE', *, *, #21940, .F. ) ;
#770 = EDGE_CURVE ( 'NONE', #13440, #321, #29228, .T. ) ;
#771 = CARTESIAN_POINT ( 'NONE',  ( 12.95659581195171484, 11.04149104205339782, 7.080843742048788414 ) ) ;
#772 = EDGE_LOOP ( 'NONE', ( #4852, #18862, #30452, #1067 ) ) ;
#773 = CARTESIAN_POINT ( 'NONE',  ( 18.72830449397920560, -7.068013160879066170, 6.447548852708279377 ) ) ;
#774 = PRODUCT_DEFINITION_CONTEXT ( 'detailed design', #23710, 'design' ) ;
#775 = CARTESIAN_POINT ( 'NONE',  ( 13.93942108199810193, -16.65122935894600076, 1.500000000000000000 ) ) ;
#776 = CARTESIAN_POINT ( 'NONE',  ( 24.35970437652574105, 13.37404834226503958, -16.55003854064094426 ) ) ;
#777 = ORIENTED_EDGE ( 'NONE', *, *, #17280, .T. ) ;
#778 = VECTOR ( 'NONE', #21130, 1000.000000000000000 ) ;
#779 = CARTESIAN_POINT ( 'NONE',  ( 49.75074519532149964, 69.99854282640310998, 54.74199497519533253 ) ) ;
#780 = CARTESIAN_POINT ( 'NONE',  ( -8.743977807160097981, -3.668292057955969021, 1.500000000000001332 ) ) ;
#781 = FACE_OUTER_BOUND ( 'NONE', #26889, .T. ) ;
#782 = CARTESIAN_POINT ( 'NONE',  ( -24.03057240117690441, -26.57182937991348481, 1.500000000000001332 ) ) ;
#783 = CIRCLE ( 'NONE', #24698, 0.7500000000000003331 ) ;
#784 = CARTESIAN_POINT ( 'NONE',  ( -31.18890335284658732, 19.89223002944919116, 27.50000000000001066 ) ) ;
#785 = CARTESIAN_POINT ( 'NONE',  ( 9.085188746210622668, -14.39608436040015960, 19.77662771831109367 ) ) ;
#786 = CARTESIAN_POINT ( 'NONE',  ( 30.86161751192252822, 15.46691422980913266, 40.47962024281689963 ) ) ;
#787 = ADVANCED_FACE ( 'NONE', ( #2872, #12396, #22043, #15022, #21896, #10048 ), #19557, .T. ) ;
#788 = EDGE_LOOP ( 'NONE', ( #7005, #12290, #10451, #7760 ) ) ;
#789 = EDGE_CURVE ( 'NONE', #27491, #28009, #15615, .T. ) ;
#790 = CARTESIAN_POINT ( 'NONE',  ( 26.58938213246210580, 6.321715805855840031, 47.66948656093867243 ) ) ;
#791 = ADVANCED_FACE ( 'NONE', ( #25481 ), #27968, .F. ) ;
#792 = CARTESIAN_POINT ( 'NONE',  ( 4.336808689942017736E-16, 42.50000000000000000, -1.500000000000000000 ) ) ;
#793 = CIRCLE ( 'NONE', #3294, 2.061368542273053883 ) ;
#794 = CARTESIAN_POINT ( 'NONE',  ( 46.83962869229247872, 69.75107682583961832, 59.80789731659786668 ) ) ;
#795 = ADVANCED_FACE ( 'NONE', ( #1471 ), #25006, .F. ) ;
#796 = ORIENTED_EDGE ( 'NONE', *, *, #17613, .F. ) ;
#797 = CARTESIAN_POINT ( 'NONE',  ( 0.000000000000000000, 0.000000000000000000, -1.500000000000000000 ) ) ;
#798 = DIRECTION ( 'NONE',  ( -0.000000000000000000, 1.132880637372608986E-16, -1.000000000000000000 ) ) ;
#799 = EDGE_CURVE ( 'NONE', #24988, #12790, #28615, .T. ) ;
#800 = FACE_OUTER_BOUND ( 'NONE', #27813, .T. ) ;
#801 = CARTESIAN_POINT ( 'NONE',  ( -4.163336342344337027E-14, -1.387778780781445676E-14, 1.500000000000000000 ) ) ;
#802 = CARTESIAN_POINT ( 'NONE',  ( 10.11202017158399968, 41.14070756921128691, -1.500000000000000000 ) ) ;
#803 = EDGE_CURVE ( 'NONE', #26662, #24952, #7407, .T. ) ;
#804 = FACE_OUTER_BOUND ( 'NONE', #18026, .T. ) ;
#805 = AXIS2_PLACEMENT_3D ( 'NONE', #19527, #29041, #19830 ) ;
#806 = CARTESIAN_POINT ( 'NONE',  ( 0.000000000000000000, -14.99999999999997158, -40.00000000000000711 ) ) ;
#807 = EDGE_CURVE ( 'NONE', #6797, #17083, #20091, .T. ) ;
#808 = DIRECTION ( 'NONE',  ( -0.000000000000000000, 1.132880637372608986E-16, -1.000000000000000000 ) ) ;
#809 = ORIENTED_EDGE ( 'NONE', *, *, #12803, .T. ) ;
#810 = AXIS2_PLACEMENT_3D ( 'NONE', #29533, #8170, #12389 ) ;
#811 = VECTOR ( 'NONE', #29749, 1000.000000000000000 ) ;
#812 = CARTESIAN_POINT ( 'NONE',  ( 32.82330813384209023, -22.94799032726822929, -1.500000000000000000 ) ) ;
#813 = CARTESIAN_POINT ( 'NONE',  ( 32.98805937973593672, 0.000000000000000000, 18.00000000000000000 ) ) ;
#814 = CARTESIAN_POINT ( 'NONE',  ( 32.51029041841470502, 26.37763988598561937, -16.50000000000000000 ) ) ;
#815 =( REPRESENTATION_RELATIONSHIP ('NONE','NONE', #19885, #16871 ) REPRESENTATION_RELATIONSHIP_WITH_TRANSFORMATION ( #16768 )SHAPE_REPRESENTATION_RELATIONSHIP( ) );
#816 = EDGE_LOOP ( 'NONE', ( #10122, #28506 ) ) ;
#817 = ORIENTED_EDGE ( 'NONE', *, *, #19707, .F. ) ;
#818 = DIRECTION ( 'NONE',  ( 1.000000000000000000, 0.000000000000000000, -1.369518533665900312E-16 ) ) ;
#819 = AXIS2_PLACEMENT_3D ( 'NONE', #4409, #15801, #25484 ) ;
#820 = EDGE_LOOP ( 'NONE', ( #21441, #11766, #4890, #26992 ) ) ;
#821 = CARTESIAN_POINT ( 'NONE',  ( 0.000000000000000000, 0.000000000000000000, -1.500000000000000000 ) ) ;
#822 = CIRCLE ( 'NONE', #25229, 3.000000000000002665 ) ;
#823 = EDGE_CURVE ( 'NONE', #12314, #11064, #25600, .T. ) ;
#824 = CARTESIAN_POINT ( 'NONE',  ( -15.61095767114878541, 35.65786817450091206, 34.50000000000000000 ) ) ;
#825 = CARTESIAN_POINT ( 'NONE',  ( 0.000000000000000000, 0.000000000000000000, 21.50000000000000000 ) ) ;
#826 = CARTESIAN_POINT ( 'NONE',  ( -37.62287076735433544, 11.19774653192125591, 14.88367311033162821 ) ) ;
#827 = AXIS2_PLACEMENT_3D ( 'NONE', #20012, #14867, #17674 ) ;
#828 = CARTESIAN_POINT ( 'NONE',  ( -20.71335220384823117, 27.86167394782616213, -16.50000600000000262 ) ) ;
#829 = B_SPLINE_CURVE_WITH_KNOTS ( 'NONE', 3,
 ( #14168, #27929, #2173, #18565, #16516, #23839, #2018, #21343, #6847, #30856, #9500, #11688, #18868, #16207, #16370, #4814, #25727, #4355, #28382, #13880 ),
 .UNSPECIFIED., .F., .F.,
 ( 4, 2, 2, 2, 2, 2, 2, 2, 2, 4 ),
 ( 0.000000000000000000, 0.06250000000000092981, 0.1250000000000018596, 0.1875000000000027756, 0.2187500000000024980, 0.2500000000000022204, 0.3125000000000016653, 0.3750000000000010547, 0.4375000000000004996, 0.4999999999999998890 ),
 .UNSPECIFIED. ) ;
#830 = EDGE_LOOP ( 'NONE', ( #15023, #29937 ) ) ;
#831 = CIRCLE ( 'NONE', #11309, 7.500000000000007105 ) ;
#832 = CARTESIAN_POINT ( 'NONE',  ( 10.50506478158603230, 13.32952022457704544, -0.6213203435596476032 ) ) ;
#833 = CARTESIAN_POINT ( 'NONE',  ( -7.075845757273814415E-16, 65.00000000000000000, 15.49999999999998757 ) ) ;
#834 = CARTESIAN_POINT ( 'NONE',  ( 12.35846532919128116, 11.73919094318043221, 20.34789198813115263 ) ) ;
#835 = CARTESIAN_POINT ( 'NONE',  ( -33.16313691975489064, 7.028748154183637631, -1.500000000000000000 ) ) ;
#836 = EDGE_CURVE ( 'NONE', #12567, #28720, #7238, .T. ) ;
#837 = EDGE_LOOP ( 'NONE', ( #26502, #26520, #16395, #29491 ) ) ;
#838 = EDGE_CURVE ( 'NONE', #18044, #17963, #995, .T. ) ;
#839 = VECTOR ( 'NONE', #15202, 1000.000000000000000 ) ;
#840 = AXIS2_PLACEMENT_3D ( 'NONE', #28772, #2576, #21589 ) ;
#841 = CARTESIAN_POINT ( 'NONE',  ( -17.99620775894062064, -8.766556869501982874, 7.643931100913408550 ) ) ;
#842 = LINE ( 'NONE', #3035, #21019 ) ;
#843 = CARTESIAN_POINT ( 'NONE',  ( 10.52132926683980685, -13.44281371605820752, 6.041646659195333058 ) ) ;
#844 = CARTESIAN_POINT ( 'NONE',  ( 5.105024945674004222, 42.22604126506330857, -1.500000000000000000 ) ) ;
#845 = DIRECTION ( 'NONE',  ( 1.000000000000000000, 0.000000000000000000, 0.000000000000000000 ) ) ;
#846 = VECTOR ( 'NONE', #2060, 1000.000000000000000 ) ;
#847 = ORIENTED_EDGE ( 'NONE', *, *, #7863, .T. ) ;
#848 = ORIENTED_EDGE ( 'NONE', *, *, #26955, .T. ) ;
#849 = CARTESIAN_POINT ( 'NONE',  ( -23.21352257770656990, -10.78826658734919519, 45.15942333309109813 ) ) ;
#850 = CARTESIAN_POINT ( 'NONE',  ( -1.438332125858111432, 8.884323311075791096, 1.500000000000001332 ) ) ;
#851 = CARTESIAN_POINT ( 'NONE',  ( -14.94322542805485554, 13.31996107294430765, 5.862424720655265098 ) ) ;
#852 = PLANE ( 'NONE',  #17635 ) ;
#853 = ORIENTED_EDGE ( 'NONE', *, *, #25955, .F. ) ;
#854 = DIRECTION ( 'NONE',  ( 1.000000000000000000, 0.000000000000000000, 0.000000000000000000 ) ) ;
#855 = CIRCLE ( 'NONE', #18782, 1.447898107987198646 ) ;
#856 = CYLINDRICAL_SURFACE ( 'NONE', #7221, 0.7499999999999997780 ) ;
#857 = VECTOR ( 'NONE', #15365, 1000.000000000000000 ) ;
#858 = ORIENTED_EDGE ( 'NONE', *, *, #7497, .F. ) ;
#859 = CARTESIAN_POINT ( 'NONE',  ( 37.99999999999999289, 90.00000000000001421, -34.50000000000000000 ) ) ;
#860 = VECTOR ( 'NONE', #3364, 1000.000000000000000 ) ;
#861 = CARTESIAN_POINT ( 'NONE',  ( 1.000000000000008438, 13.00000000000001421, 43.10779406592839536 ) ) ;
#862 = CARTESIAN_POINT ( 'NONE',  ( -34.80856967755993736, -19.21184172954434999, 31.15481810886020497 ) ) ;
#863 = VERTEX_POINT ( 'NONE', #2675 ) ;
#864 = DIRECTION ( 'NONE',  ( -1.000000000000000000, 0.000000000000000000, 0.000000000000000000 ) ) ;
#865 = EDGE_CURVE ( 'NONE', #4126, #15180, #12302, .T. ) ;
#866 = CARTESIAN_POINT ( 'NONE',  ( 0.3518703668723790479, -19.99690444156084013, 20.34789198813115263 ) ) ;
#867 = VECTOR ( 'NONE', #15137, 1000.000000000000000 ) ;
#868 = EDGE_CURVE ( 'NONE', #29154, #3530, #21387, .T. ) ;
#869 = DIRECTION ( 'NONE',  ( 0.000000000000000000, -0.000000000000000000, 1.000000000000000000 ) ) ;
#870 = CARTESIAN_POINT ( 'NONE',  ( -19.71440049134194084, 3.368233808196385404, 18.84056766331481825 ) ) ;
#871 = AXIS2_PLACEMENT_3D ( 'NONE', #23570, #30756, #18919 ) ;
#872 = ORIENTED_EDGE ( 'NONE', *, *, #18796, .T. ) ;
#873 = DIRECTION ( 'NONE',  ( 0.000000000000000000, 0.000000000000000000, 1.000000000000000000 ) ) ;
#874 = FILL_AREA_STYLE_COLOUR ( '', #12747 ) ;
#875 = VECTOR ( 'NONE', #3921, 1000.000000000000000 ) ;
#876 = CARTESIAN_POINT ( 'NONE',  ( 8.419710366748642372, 7.777014463793876509, 1.500000000000000000 ) ) ;
#877 = AXIS2_PLACEMENT_3D ( 'NONE', #2661, #478, #28713 ) ;
#878 = DIRECTION ( 'NONE',  ( -1.000000000000000000, -0.000000000000000000, -0.000000000000000000 ) ) ;
#879 = PLANE ( 'NONE',  #17324 ) ;
#880 = CARTESIAN_POINT ( 'NONE',  ( -8.268028093133395373, -3.763133143576407935, 21.50000000000000000 ) ) ;
#881 = DIRECTION ( 'NONE',  ( -1.000000000000000000, 0.000000000000000000, 0.000000000000000000 ) ) ;
#882 = ORIENTED_EDGE ( 'NONE', *, *, #25559, .F. ) ;
#883 = CARTESIAN_POINT ( 'NONE',  ( 7.730328572437743517, -4.608906612435629491, 1.500000000000001332 ) ) ;
#884 = AXIS2_PLACEMENT_3D ( 'NONE', #30746, #18912, #29927 ) ;
#885 = DIRECTION ( 'NONE',  ( -0.8412535328311804284, 0.5406408174555987767, 0.000000000000000000 ) ) ;
#886 = VERTEX_POINT ( 'NONE', #23419 ) ;
#887 = EDGE_LOOP ( 'NONE', ( #3868, #22327 ) ) ;
#888 = CARTESIAN_POINT ( 'NONE',  ( -12.17697269691152329, 40.41958668078866879, 21.44088211123782983 ) ) ;
#889 = VECTOR ( 'NONE', #15046, 1000.000000000000000 ) ;
#890 = CARTESIAN_POINT ( 'NONE',  ( 8.884323311075775109, 1.438332125858202692, -1.500000000000001776 ) ) ;
#891 =( LENGTH_UNIT ( ) NAMED_UNIT ( * ) SI_UNIT ( .MILLI., .METRE. ) );
#892 = AXIS2_PLACEMENT_3D ( 'NONE', #11854, #12161, #21660 ) ;
#893 = CARTESIAN_POINT ( 'NONE',  ( 9.634323311075775109, 1.438332125858202692, 1.500000000000001332 ) ) ;
#894 = CIRCLE ( 'NONE', #1872, 0.7500000000000006661 ) ;
#895 = CARTESIAN_POINT ( 'NONE',  ( 14.97043017101258577, 13.28903844302880266, 18.35377592296120497 ) ) ;
#896 = B_SPLINE_CURVE_WITH_KNOTS ( 'NONE', 3,
 ( #27424, #24449, #15392, #24916, #17910, #27106, #10419, #1219, #17442, #15223, #5729, #19935, #10719, #3089, #7769, #29600, #22103, #29450 ),
 .UNSPECIFIED., .F., .F.,
 ( 4, 2, 2, 2, 2, 2, 2, 2, 4 ),
 ( 0.003174295595554312618, 0.003570702171545548417, 0.003967108747536783782, 0.004363515323528019581, 0.004759921899519255380, 0.005156328475510491179, 0.005552735051501726977, 0.005949141627492962776, 0.006345548203484198575 ),
 .UNSPECIFIED. ) ;
#897 = VERTEX_POINT ( 'NONE', #21221 ) ;
#898 = EDGE_LOOP ( 'NONE', ( #12196, #14932, #9204, #16861 ) ) ;
#899 = CARTESIAN_POINT ( 'NONE',  ( 15.98415658701446773, -5.958736450466529000, 20.25542030744407640 ) ) ;
#900 = CARTESIAN_POINT ( 'NONE',  ( 16.68770897235364714, 3.522277800415037685, 20.29915277494337644 ) ) ;
#901 = CIRCLE ( 'NONE', #26810, 0.7499999999999997780 ) ;
#902 = CARTESIAN_POINT ( 'NONE',  ( -4.163336342344337027E-14, -1.387778780781445676E-14, 1.500000000000000000 ) ) ;
#903 = ORIENTED_EDGE ( 'NONE', *, *, #17740, .F. ) ;
#904 = CIRCLE ( 'NONE', #7825, 9.482273699623480212 ) ;
#905 = CARTESIAN_POINT ( 'NONE',  ( -37.99999999999999289, 209.2686044187655909, -34.49999999999999289 ) ) ;
#906 = CARTESIAN_POINT ( 'NONE',  ( 27.03074382657074537, 6.449748410230989215, -16.55003854064094426 ) ) ;
#907 = EDGE_CURVE ( 'NONE', #20436, #24781, #5018, .T. ) ;
#908 = ORIENTED_EDGE ( 'NONE', *, *, #23214, .F. ) ;
#909 = CARTESIAN_POINT ( 'NONE',  ( 22.58267429318971864, 26.57182937991349903, 26.54355021145562787 ) ) ;
#910 =( GEOMETRIC_REPRESENTATION_CONTEXT ( 3 ) GLOBAL_UNCERTAINTY_ASSIGNED_CONTEXT ( ( #13624 ) ) GLOBAL_UNIT_ASSIGNED_CONTEXT ( ( #14769, #3081, #22254 ) ) REPRESENTATION_CONTEXT ( 'NONE', 'WORKASPACE' ) );
#911 = CARTESIAN_POINT ( 'NONE',  ( 31.45274955338841494, -26.35877938683194088, -8.166661939779828572 ) ) ;
#912 = B_SPLINE_SURFACE_WITH_KNOTS ( 'NONE', 3, 1, ( 
 ( #20892, #1721 ),
 ( #25123, #18111 ),
 ( #30417, #8743 ),
 ( #8909, #16074 ),
 ( #27626, #4067 ),
 ( #9055, #4210 ),
 ( #8463, #13733 ),
 ( #23223, #11236 ),
 ( #22779, #13284 ),
 ( #18433, #10949 ),
 ( #17965, #27323 ),
 ( #6250, #1583 ),
 ( #15450, #27934 ),
 ( #27474, #6562 ),
 ( #1877, #13128 ),
 ( #2491, #21500 ),
 ( #14491, #28223 ),
 ( #28389, #7014 ),
 ( #30705, #26190 ),
 ( #294, #21040 ),
 ( #9355, #7330 ),
 ( #6855, #16840 ),
 ( #2640, #30562 ),
 ( #25890, #19171 ),
 ( #23680, #21832 ),
 ( #16216, #18713 ),
 ( #28692, #2023 ),
 ( #12159, #28538 ),
 ( #6701, #11852 ),
 ( #4821, #23533 ),
 ( #16375, #4519 ) ),
 .UNSPECIFIED., .F., .F., .F.,
 ( 4, 3, 3, 3, 3, 3, 3, 3, 3, 3, 4 ),
 ( 2, 2 ),
 ( 0.000000000000000000, 0.05425176834609614362, 0.1085332949128348518, 0.1623767749169379715, 0.2157504826133058717, 0.2688657508888169789, 0.3218907763505471364, 0.3749548578363334772, 0.4282048033836237666, 0.4818374082110496448, 0.4999999999131650164 ),
 ( 0.000000000000000000, 1.000000000000000000 ),
 .UNSPECIFIED. ) ;
#913 = CARTESIAN_POINT ( 'NONE',  ( 19.59419491516168321, 4.095680178559270246, 7.098451512883313441 ) ) ;
#914 = CARTESIAN_POINT ( 'NONE',  ( -15.07239450771860056, 13.17334274624126422, 18.44501272782439827 ) ) ;
#915 = AXIS2_PLACEMENT_3D ( 'NONE', #16296, #11613, #18792 ) ;
#916 = AXIS2_PLACEMENT_3D ( 'NONE', #10436, #27126, #12313 ) ;
#917 = CARTESIAN_POINT ( 'NONE',  ( -7.809214384344184801, -15.18204291278971496, 19.89182036555910571 ) ) ;
#918 = CARTESIAN_POINT ( 'NONE',  ( -38.56714466680799802, -6.442804806652034699, 32.09716166004417914 ) ) ;
#919 = DIRECTION ( 'NONE',  ( 0.000000000000000000, 1.000000000000000000, 0.000000000000000000 ) ) ;
#920 = FACE_OUTER_BOUND ( 'NONE', #25459, .T. ) ;
#921 = ORIENTED_EDGE ( 'NONE', *, *, #28797, .F. ) ;
#922 = CARTESIAN_POINT ( 'NONE',  ( 9.054000795813635705, -14.41483084819681615, 6.310736198168394928 ) ) ;
#923 = CARTESIAN_POINT ( 'NONE',  ( -29.80493885133978083, 27.41358096823880786, 9.131458560479140729 ) ) ;
#924 = AXIS2_PLACEMENT_3D ( 'NONE', #17670, #19692, #8017 ) ;
#925 = CARTESIAN_POINT ( 'NONE',  ( 12.86767874445214055, -1.850092897552706894, 1.500000000000001332 ) ) ;
#926 = ORIENTED_EDGE ( 'NONE', *, *, #14035, .F. ) ;
#927 = ORIENTED_EDGE ( 'NONE', *, *, #27710, .F. ) ;
#928 = DIRECTION ( 'NONE',  ( 0.000000000000000000, 1.000000000000000000, 0.000000000000000000 ) ) ;
#929 = LINE ( 'NONE', #17619, #19604 ) ;
#930 = DIRECTION ( 'NONE',  ( -0.000000000000000000, -0.000000000000000000, -1.000000000000000000 ) ) ;
#931 = ORIENTED_EDGE ( 'NONE', *, *, #11263, .T. ) ;
#932 = LINE ( 'NONE', #24944, #23092 ) ;
#933 = DIRECTION ( 'NONE',  ( 1.000000000000000000, 0.000000000000000000, 0.000000000000000000 ) ) ;
#934 = CARTESIAN_POINT ( 'NONE',  ( 6.237549684377459158, 19.00251437819605371, 6.913388067999410858 ) ) ;
#935 = PRODUCT_DEFINITION_FORMATION_WITH_SPECIFIED_SOURCE ( 'ANY', '', #4681, .NOT_KNOWN. ) ;
#936 = EDGE_LOOP ( 'NONE', ( #6511, #6269, #30437, #7742 ) ) ;
#937 = AXIS2_PLACEMENT_3D ( 'NONE', #4742, #527, #19100 ) ;
#938 = DIRECTION ( 'NONE',  ( -1.000000000000000000, 0.000000000000000000, 0.000000000000000000 ) ) ;
#939 = CIRCLE ( 'NONE', #18392, 15.00000000000003375 ) ;
#940 = CARTESIAN_POINT ( 'NONE',  ( -5.881244434206279514, -6.812559277181949646, 1.500000000000001332 ) ) ;
#941 = AXIS2_PLACEMENT_3D ( 'NONE', #27026, #2189, #4376 ) ;
#942 = EDGE_CURVE ( 'NONE', #28122, #2953, #17667, .T. ) ;
#943 = CARTESIAN_POINT ( 'NONE',  ( 19.84141769772507402, 2.653416696629036675, 7.500898271101006820 ) ) ;
#944 = ORIENTED_EDGE ( 'NONE', *, *, #30481, .F. ) ;
#945 = DIRECTION ( 'NONE',  ( -1.000000000000000000, 0.000000000000000000, 0.000000000000000000 ) ) ;
#946 = VERTEX_POINT ( 'NONE', #18914 ) ;
#947 = CARTESIAN_POINT ( 'NONE',  ( 10.18506332983505303, 29.04537757311072710, 24.50000000000000000 ) ) ;
#948 = CARTESIAN_POINT ( 'NONE',  ( 31.89304216768362821, -14.79375299452194170, 35.60059606544044186 ) ) ;
#949 = CIRCLE ( 'NONE', #4929, 0.7500000000000003331 ) ;
#950 = VERTEX_POINT ( 'NONE', #12191 ) ;
#951 = ADVANCED_FACE ( 'NONE', ( #21689 ), #328, .F. ) ;
#952 = CARTESIAN_POINT ( 'NONE',  ( 4.316117848019423775, 19.54676362458759087, 6.672349528511551497 ) ) ;
#953 = EDGE_CURVE ( 'NONE', #29550, #14341, #3391, .T. ) ;
#954 = CARTESIAN_POINT ( 'NONE',  ( 24.44496207165490276, 7.595930209050162141, 49.40206402021032517 ) ) ;
#955 = CARTESIAN_POINT ( 'NONE',  ( -4.163336342344337027E-14, -1.387778780781445676E-14, -1.500000000000000000 ) ) ;
#956 = CARTESIAN_POINT ( 'NONE',  ( 16.53285166946374929, 35.10262665635723778, 34.50000000000000000 ) ) ;
#957 = B_SPLINE_CURVE_WITH_KNOTS ( 'NONE', 3,
 ( #20118, #27608, #5770, #27144, #14969, #24482, #12648, #27299, #19967, #764, #10288, #19803, #8121, #29331, #15263, #7972, #17476, #17627 ),
 .UNSPECIFIED., .F., .F.,
 ( 4, 2, 2, 2, 2, 2, 2, 2, 4 ),
 ( 0.000000000000000000, 0.0003967869494442840357, 0.0007935738988885680713, 0.001190360848332851999, 0.001587147797777136143, 0.001983934747221420287, 0.002380721696665703997, 0.002777508646109988141, 0.003174295595554272285 ),
 .UNSPECIFIED. ) ;
#958 = CARTESIAN_POINT ( 'NONE',  ( -15.57266529552203416, -38.96488032230103471, 1.500000000000000000 ) ) ;
#959 = CARTESIAN_POINT ( 'NONE',  ( 10.26079415706018771, -17.18817258638080148, 19.45164628100866722 ) ) ;
#960 = CARTESIAN_POINT ( 'NONE',  ( 30.74147208807243103, 15.49548351932574874, 40.57409041152969564 ) ) ;
#961 = ORIENTED_EDGE ( 'NONE', *, *, #13499, .F. ) ;
#962 = DIRECTION ( 'NONE',  ( 1.000000000000000000, 0.000000000000000000, 0.000000000000000000 ) ) ;
#963 = VECTOR ( 'NONE', #30345, 1000.000000000000000 ) ;
#964 = CARTESIAN_POINT ( 'NONE',  ( -13.78503626495110446, 10.05991541429405522, 18.56793045041961321 ) ) ;
#965 = CARTESIAN_POINT ( 'NONE',  ( 33.50775388423620882, 10.82565592554877121, 35.54444202463886882 ) ) ;
#966 = CARTESIAN_POINT ( 'NONE',  ( -13.00999358272542494, -0.8602714556717691030, 24.50000000000000000 ) ) ;
#967 = ORIENTED_EDGE ( 'NONE', *, *, #11204, .F. ) ;
#968 = EDGE_CURVE ( 'NONE', #15364, #12485, #28729, .T. ) ;
#969 = CARTESIAN_POINT ( 'NONE',  ( 30.16810946264573445, -26.93506237724814412, 17.13185035612489315 ) ) ;
#970 = CARTESIAN_POINT ( 'NONE',  ( -16.96496224101209194, 1.652369717150043549, 20.34789198813115263 ) ) ;
#971 = CARTESIAN_POINT ( 'NONE',  ( 12.69259498021937382, 11.35795912679306063, 7.526951045817046548 ) ) ;
#972 = DIRECTION ( 'NONE',  ( 0.000000000000000000, 0.000000000000000000, 1.000000000000000000 ) ) ;
#973 = CARTESIAN_POINT ( 'NONE',  ( -17.26937953831790651, 14.36006998371489551, 1.500000000000000000 ) ) ;
#974 = VECTOR ( 'NONE', #27914, 1000.000000000000000 ) ;
#975 = CARTESIAN_POINT ( 'NONE',  ( 77.99999999999998579, -42.50000000000001421, 27.50000000000000711 ) ) ;
#976 = CARTESIAN_POINT ( 'NONE',  ( 7.864568376310370645, 41.74085412114251881, 28.90542812248210325 ) ) ;
#977 = VERTEX_POINT ( 'NONE', #7367 ) ;
#978 = ADVANCED_FACE ( 'NONE', ( #28 ), #7045, .T. ) ;
#979 = CARTESIAN_POINT ( 'NONE',  ( 26.12638453225886792, 6.310846377660614515, 43.87962907655873579 ) ) ;
#980 = CARTESIAN_POINT ( 'NONE',  ( 37.99999999999999289, 80.00000000000000000, 0.000000000000000000 ) ) ;
#981 = DIRECTION ( 'NONE',  ( -0.8910248307962436165, -0.4539545692076747407, -0.000000000000000000 ) ) ;
#982 = ORIENTED_EDGE ( 'NONE', *, *, #8425, .T. ) ;
#983 = EDGE_CURVE ( 'NONE', #14509, #24952, #16713, .T. ) ;
#984 = VERTEX_POINT ( 'NONE', #21071 ) ;
#985 = EDGE_CURVE ( 'NONE', #23990, #4772, #30594, .T. ) ;
#986 = CARTESIAN_POINT ( 'NONE',  ( -11.46182693247433804, -1.387778780781445676E-14, 1.500000000000000000 ) ) ;
#987 = ORIENTED_EDGE ( 'NONE', *, *, #11268, .T. ) ;
#988 = DIRECTION ( 'NONE',  ( -0.000000000000000000, -0.000000000000000000, -1.000000000000000000 ) ) ;
#989 = CARTESIAN_POINT ( 'NONE',  ( -33.70208146031188789, 13.89198562565741923, 34.49999999999999289 ) ) ;
#990 = EDGE_CURVE ( 'NONE', #6958, #27304, #16554, .T. ) ;
#991 = LINE ( 'NONE', #7551, #25468 ) ;
#992 = CARTESIAN_POINT ( 'NONE',  ( -33.31304828179383293, 22.10896115714093924, 8.000000000000005329 ) ) ;
#993 = AXIS2_PLACEMENT_3D ( 'NONE', #30844, #28672, #23658 ) ;
#995 = B_SPLINE_CURVE_WITH_KNOTS ( 'NONE', 3,
 ( #11129, #20628, #30146, #15962, #30750, #9393, #21536, #24028, #23883, #14206, #14058, #171, #16252, #4861 ),
 .UNSPECIFIED., .F., .F.,
 ( 4, 2, 2, 2, 2, 2, 4 ),
 ( 2.111077618484504239E-07, 0.0004668847438969890226, 0.0009335583800321295943, 0.001400232016167270166, 0.001866905652302410738, 0.002800252924572703590, 0.003733600196842996443 ),
 .UNSPECIFIED. ) ;
#994 = CARTESIAN_POINT ( 'NONE',  ( -23.17581250239728519, -34.50630206824673252, 1.499999999999999778 ) ) ;
#996 = DIRECTION ( 'NONE',  ( -1.000000000000000000, 0.000000000000000000, 0.000000000000000000 ) ) ;
#997 = LINE ( 'NONE', #10507, #28045 ) ;
#998 = CARTESIAN_POINT ( 'NONE',  ( 1.121436987360518778, -17.01878714021720285, 5.704143890883081269 ) ) ;
#999 = CARTESIAN_POINT ( 'NONE',  ( -5.971396161871753705, 19.08775596758252391, 7.652108011868850035 ) ) ;
#1000 = EDGE_CURVE ( 'NONE', #203, #4677, #25923, .T. ) ;
#1001 = VERTEX_POINT ( 'NONE', #4552 ) ;
#1002 = EDGE_CURVE ( 'NONE', #25635, #16019, #6828, .T. ) ;
#1003 = CARTESIAN_POINT ( 'NONE',  ( -9.310272263096074141, -14.25176022191445036, 18.90679857307105749 ) ) ;
#1004 = DIRECTION ( 'NONE',  ( 0.000000000000000000, 0.000000000000000000, 1.000000000000000000 ) ) ;
#1005 = CARTESIAN_POINT ( 'NONE',  ( -5.615427697021304176, 16.09608755218563303, 7.652108011868850035 ) ) ;
#1006 = EDGE_CURVE ( 'NONE', #20257, #22873, #4629, .T. ) ;
#1007 = CARTESIAN_POINT ( 'NONE',  ( 10.65192122195201740, -13.34697535456212236, 6.341840715582230281 ) ) ;
#1008 = DIRECTION ( 'NONE',  ( 0.000000000000000000, 1.000000000000000000, -0.000000000000000000 ) ) ;
#1009 = CARTESIAN_POINT ( 'NONE',  ( -15.34307810681595896, 12.82926163924266660, 20.34789198813115263 ) ) ;
#1010 = ORIENTED_EDGE ( 'NONE', *, *, #24861, .F. ) ;
#1011 = ORIENTED_EDGE ( 'NONE', *, *, #6998, .T. ) ;
#1012 = CARTESIAN_POINT ( 'NONE',  ( -4.622016212553093695, -12.19167610014704906, 1.500000000000001332 ) ) ;
#1013 = CARTESIAN_POINT ( 'NONE',  ( -39.83602371821029919, -11.57901747687044924, -19.50000000000000355 ) ) ;
#1014 = CARTESIAN_POINT ( 'NONE',  ( -13.30790957887532677, 10.64596135573641789, 5.657991946698900598 ) ) ;
#1015 = CARTESIAN_POINT ( 'NONE',  ( 0.1624814966347698231, -17.02900520012292773, 5.848946451764563292 ) ) ;
#1016 = ORIENTED_EDGE ( 'NONE', *, *, #28061, .F. ) ;
#1017 = AXIS2_PLACEMENT_3D ( 'NONE', #1740, #20609, #28248 ) ;
#1018 = CYLINDRICAL_SURFACE ( 'NONE', #7276, 9.482273699623480212 ) ;
#1019 = LINE ( 'NONE', #10529, #11195 ) ;
#1020 = ADVANCED_FACE ( 'NONE', ( #2831 ), #21857, .F. ) ;
#1021 = ORIENTED_EDGE ( 'NONE', *, *, #620, .T. ) ;
#1022 = CARTESIAN_POINT ( 'NONE',  ( 5.069257791428380955, -7.538175180318438251, -1.500000000000002665 ) ) ;
#1023 = EDGE_CURVE ( 'NONE', #4256, #10933, #14676, .T. ) ;
#1024 = LINE ( 'NONE', #9918, #9861 ) ;
#1025 = EDGE_CURVE ( 'NONE', #30101, #30448, #12431, .T. ) ;
#1026 = CARTESIAN_POINT ( 'NONE',  ( -28.50858587296695745, -29.13344744256045615, 30.13847653714394070 ) ) ;
#1027 = ORIENTED_EDGE ( 'NONE', *, *, #5345, .F. ) ;
#1028 = CYLINDRICAL_SURFACE ( 'NONE', #9384, 0.7441270634457198829 ) ;
#1029 = EDGE_CURVE ( 'NONE', #14253, #23209, #26965, .T. ) ;
#1030 = CARTESIAN_POINT ( 'NONE',  ( 39.99999999999998579, 90.00000000000001421, 22.49999999999999289 ) ) ;
#1031 = DIRECTION ( 'NONE',  ( -0.9329908884337535513, 0.3598999890241665334, 0.000000000000000000 ) ) ;
#1032 = CARTESIAN_POINT ( 'NONE',  ( -2.185336383880142730, 8.817355867515834333, -1.500000000000000666 ) ) ;
#1033 = VERTEX_POINT ( 'NONE', #5324 ) ;
#1034 = CARTESIAN_POINT ( 'NONE',  ( 39.99999999999998579, 90.00000000000001421, 52.49999999999999289 ) ) ;
#1035 = DIRECTION ( 'NONE',  ( -0.000000000000000000, 0.000000000000000000, -1.000000000000000000 ) ) ;
#1036 = EDGE_CURVE ( 'NONE', #3590, #15421, #14834, .T. ) ;
#1037 = DIRECTION ( 'NONE',  ( -1.000000000000000000, 0.000000000000000000, 0.000000000000000000 ) ) ;
#1038 = B_SPLINE_CURVE_WITH_KNOTS ( 'NONE', 3,
 ( #18272, #27795, #6420, #16082, #4219, #6712, #9365, #28701, #30717, #14183 ),
 .UNSPECIFIED., .F., .F.,
 ( 4, 2, 2, 2, 4 ),
 ( 0.000000000000000000, 0.005347349928980100683, 0.01069469985796020657, 0.01604204978694031072, 0.02138939971592041661 ),
 .UNSPECIFIED. ) ;
#1039 = CIRCLE ( 'NONE', #2525, 19.49999999999996447 ) ;
#1040 = B_SPLINE_CURVE_WITH_KNOTS ( 'NONE', 3,
 ( #16024, #18829, #21137, #6657, #4166, #1985, #30215, #28346, #16174, #11647, #6973, #9156, #11797, #18669, #13992, #27731, #11507, #18382 ),
 .UNSPECIFIED., .F., .F.,
 ( 4, 2, 2, 2, 2, 2, 2, 2, 4 ),
 ( 0.003174295595554314786, 0.003570702171545546248, 0.003967108747536777710, 0.004363515323528009172, 0.004759921899519240635, 0.005156328475510472097, 0.005552735051501703559, 0.005949141627492935021, 0.006345548203484166483 ),
 .UNSPECIFIED. ) ;
#1041 = CARTESIAN_POINT ( 'NONE',  ( -43.34097750826428097, -11.89502811014148342, -1.500000000000000444 ) ) ;
#1042 = DIRECTION ( 'NONE',  ( -0.000000000000000000, -1.000000000000000000, -0.000000000000000000 ) ) ;
#1043 = CARTESIAN_POINT ( 'NONE',  ( -34.99999999999933920, 0.000000000000000000, 92.49999999999998579 ) ) ;
#1044 = DIRECTION ( 'NONE',  ( 0.000000000000000000, 0.000000000000000000, 1.000000000000000000 ) ) ;
#1045 = EDGE_LOOP ( 'NONE', ( #21010, #23392 ) ) ;
#1046 = DIRECTION ( 'NONE',  ( -0.000000000000000000, -0.000000000000000000, -1.000000000000000000 ) ) ;
#1047 = CARTESIAN_POINT ( 'NONE',  ( 4.307942169702170254, 19.53053083060024164, 6.523620417364449864 ) ) ;
#1048 = VERTEX_POINT ( 'NONE', #5486 ) ;
#1049 = ORIENTED_EDGE ( 'NONE', *, *, #3733, .T. ) ;
#1050 = CARTESIAN_POINT ( 'NONE',  ( 0.3567158762617958501, -19.99681059701335073, 5.652196082369963293 ) ) ;
#1051 = FACE_OUTER_BOUND ( 'NONE', #29406, .T. ) ;
#1052 = EDGE_CURVE ( 'NONE', #4045, #16098, #4383, .T. ) ;
#1053 = CARTESIAN_POINT ( 'NONE',  ( -9.159357180470966142, 49.16077613269642654, -66.91880493524543283 ) ) ;
#1054 =( NAMED_UNIT ( * ) PLANE_ANGLE_UNIT ( ) SI_UNIT ( $, .RADIAN. ) );
#1055 = ADVANCED_FACE ( 'NONE', ( #7822 ), #17334, .F. ) ;
#1056 = DIRECTION ( 'NONE',  ( 1.000000000000000000, 0.000000000000000000, -0.000000000000000000 ) ) ;
#1057 = CARTESIAN_POINT ( 'NONE',  ( 15.43499236066653779, -3.229500095980124996, -0.6213203435596476032 ) ) ;
#1058 = EDGE_LOOP ( 'NONE', ( #9791, #10369, #20213, #24260 ) ) ;
#1059 = ORIENTED_EDGE ( 'NONE', *, *, #26955, .F. ) ;
#1060 = CARTESIAN_POINT ( 'NONE',  ( -16.88948989945504664, 2.193765388987378717, 7.500898271101006820 ) ) ;
#1061 = TOROIDAL_SURFACE ( 'NONE', #28508, 47.00000000000000000, 3.000000000000000000 ) ;
#1062 = LINE ( 'NONE', #25066, #29718 ) ;
#1063 = AXIS2_PLACEMENT_3D ( 'NONE', #16979, #17133, #5749 ) ;
#1064 = LINE ( 'NONE', #19936, #27451 ) ;
#1065 = ORIENTED_EDGE ( 'NONE', *, *, #20188, .T. ) ;
#1066 = CARTESIAN_POINT ( 'NONE',  ( -5.419526071899103847, 16.15737324489262150, 20.34789198813115974 ) ) ;
#1067 = ORIENTED_EDGE ( 'NONE', *, *, #3732, .F. ) ;
#1068 = FACE_OUTER_BOUND ( 'NONE', #20155, .T. ) ;
#1069 = ORIENTED_EDGE ( 'NONE', *, *, #15299, .F. ) ;
#1070 = FILL_AREA_STYLE ('',( #3405 ) ) ;
#1071 = CARTESIAN_POINT ( 'NONE',  ( 25.56256718580103637, -32.12586005794658206, 29.82918954436054193 ) ) ;
#1072 = CARTESIAN_POINT ( 'NONE',  ( 19.66823596311669675, 3.724077645907917677, 7.500147780736496017 ) ) ;
#1073 = CARTESIAN_POINT ( 'NONE',  ( -28.79137815760242702, -9.331429872129930914, 1.500000000000000000 ) ) ;
#1074 = LINE ( 'NONE', #29616, #14019 ) ;
#1075 = CARTESIAN_POINT ( 'NONE',  ( -9.228184491630887720, -14.30775539772383098, 7.267659094423555288 ) ) ;
#1076 = FACE_BOUND ( 'NONE', #3866, .T. ) ;
#1077 = EDGE_LOOP ( 'NONE', ( #13664, #21788, #28119, #28909 ) ) ;
#1078 = CARTESIAN_POINT ( 'NONE',  ( 15.57266529552203416, -38.96488032230103471, -1.500000000000000000 ) ) ;
#1079 = CARTESIAN_POINT ( 'NONE',  ( 11.83189508704695392, -16.14673651688228873, 18.82680253904184298 ) ) ;
#1080 = AXIS2_PLACEMENT_3D ( 'NONE', #18598, #6587, #14049 ) ;
#1081 = CARTESIAN_POINT ( 'NONE',  ( 0.000000000000000000, 13.00000000000001421, 43.10779406592839536 ) ) ;
#1082 = ORIENTED_EDGE ( 'NONE', *, *, #23253, .T. ) ;
#1083 = ORIENTED_EDGE ( 'NONE', *, *, #14308, .T. ) ;
#1084 = CARTESIAN_POINT ( 'NONE',  ( -8.728722367416567707, 2.516121109503271835, -1.500000000000001554 ) ) ;
#1085 = FACE_OUTER_BOUND ( 'NONE', #15743, .T. ) ;
#1086 = CARTESIAN_POINT ( 'NONE',  ( 49.99999999999998579, -50.00000000000000000, 12.49999999999999112 ) ) ;
#1087 = ORIENTED_EDGE ( 'NONE', *, *, #30330, .F. ) ;
#1088 = CYLINDRICAL_SURFACE ( 'NONE', #4116, 1.000000000000007772 ) ;
#1089 = EDGE_CURVE ( 'NONE', #3823, #5916, #13380, .T. ) ;
#1090 = DIRECTION ( 'NONE',  ( -0.000000000000000000, -0.000000000000000000, -1.000000000000000000 ) ) ;
#1091 = ADVANCED_FACE ( 'NONE', ( #18261 ), #27781, .F. ) ;
#1092 = CARTESIAN_POINT ( 'NONE',  ( 6.236311564447694522, 19.00292092786887110, 6.386539667786099272 ) ) ;
#1093 = ORIENTED_EDGE ( 'NONE', *, *, #990, .F. ) ;
#1094 = VECTOR ( 'NONE', #9657, 1000.000000000000000 ) ;
#1095 = B_SPLINE_CURVE_WITH_KNOTS ( 'NONE', 3,
 ( #4359, #13883, #26037, #23676 ),
 .UNSPECIFIED., .F., .F.,
 ( 4, 4 ),
 ( 0.000000000000000000, 0.1536962897835600916 ),
 .UNSPECIFIED. ) ;
#1096 = CARTESIAN_POINT ( 'NONE',  ( 8.099999999999999645, 0.000000000000000000, 0.000000000000000000 ) ) ;
#1097 = CARTESIAN_POINT ( 'NONE',  ( 14.29853178503251954, 14.00938365128603280, 6.131018562779544823 ) ) ;
#1098 = CARTESIAN_POINT ( 'NONE',  ( 16.87995935610571507, 2.188012981718273853, 6.641371103590088865 ) ) ;
#1099 = VERTEX_POINT ( 'NONE', #8461 ) ;
#1100 = CARTESIAN_POINT ( 'NONE',  ( 16.09518941752841670, 6.251081041772567737, -0.6213203435596476032 ) ) ;
#1101 = ORIENTED_EDGE ( 'NONE', *, *, #29627, .F. ) ;
#1102 = CARTESIAN_POINT ( 'NONE',  ( -13.38160118231794371, 10.55829203257429860, 18.34798005863078885 ) ) ;
#1103 = CARTESIAN_POINT ( 'NONE',  ( -33.01877980957529957, 12.12572312222180493, 39.84356070656661331 ) ) ;
#1104 = CIRCLE ( 'NONE', #15024, 9.084132297865673777 ) ;
#1105 = VERTEX_POINT ( 'NONE', #15603 ) ;
#1106 = DIRECTION ( 'NONE',  ( -1.000000000000000000, 0.000000000000000000, 0.000000000000000000 ) ) ;
#1107 = DIRECTION ( 'NONE',  ( 0.000000000000000000, 0.000000000000000000, -1.000000000000000000 ) ) ;
#1108 = DIRECTION ( 'NONE',  ( 1.000000000000000000, 0.000000000000000000, 0.000000000000000000 ) ) ;
#1109 = CARTESIAN_POINT ( 'NONE',  ( -28.55068628633582861, 24.19494186940698199, 27.50000000000001066 ) ) ;
#1110 = CARTESIAN_POINT ( 'NONE',  ( 6.899999999999999467, 10.39230484541327471, 0.000000000000000000 ) ) ;
#1111 = CARTESIAN_POINT ( 'NONE',  ( 29.15452456067735199, 29.11038375076175555, -6.500000000000000888 ) ) ;
#1112 = EDGE_LOOP ( 'NONE', ( #7316, #18014, #2350, #6079, #17115, #6493 ) ) ;
#1113 = AXIS2_PLACEMENT_3D ( 'NONE', #20021, #3967, #25158 ) ;
#1114 = DIRECTION ( 'NONE',  ( -1.000000000000000000, 0.000000000000000000, 0.000000000000000000 ) ) ;
#1115 = CARTESIAN_POINT ( 'NONE',  ( -19.64114023396061981, 37.13592150528867109, -1.500000000000000000 ) ) ;
#1116 = FACE_OUTER_BOUND ( 'NONE', #26170, .T. ) ;
#1117 = LINE ( 'NONE', #9899, #29855 ) ;
#1118 = ORIENTED_EDGE ( 'NONE', *, *, #29975, .T. ) ;
#1119 = CARTESIAN_POINT ( 'NONE',  ( 29.78864511397301484, -27.43196031439082461, 9.154089586762928832 ) ) ;
#1120 = CARTESIAN_POINT ( 'NONE',  ( -41.02681369128806210, 65.11862996399604242, 62.46341648537969604 ) ) ;
#1121 = CARTESIAN_POINT ( 'NONE',  ( -14.93932203929705871, 13.29757777824903897, 20.14992337338002670 ) ) ;
#1122 = DIRECTION ( 'NONE',  ( 1.000000000000000000, 0.000000000000000000, 0.000000000000000000 ) ) ;
#1123 = CARTESIAN_POINT ( 'NONE',  ( 24.03057240117691862, -26.57182937991349903, -1.500000000000000000 ) ) ;
#1124 = DIRECTION ( 'NONE',  ( -0.000000000000000000, 1.132880637372608986E-16, -1.000000000000000000 ) ) ;
#1125 = CARTESIAN_POINT ( 'NONE',  ( 13.29126524260693998, 35.08562276291469573, 37.49999999993516298 ) ) ;
#1126 = ORIENTED_EDGE ( 'NONE', *, *, #17165, .T. ) ;
#1127 = CARTESIAN_POINT ( 'NONE',  ( 24.44496207165490276, 7.595930209050162141, 45.15942333309104129 ) ) ;
#1128 = DIRECTION ( 'NONE',  ( -0.000000000000000000, -0.000000000000000000, 1.000000000000000000 ) ) ;
#1129 = DIRECTION ( 'NONE',  ( 1.000000000000000000, 0.000000000000000000, 0.000000000000000000 ) ) ;
#1130 = VERTEX_POINT ( 'NONE', #6559 ) ;
#1131 = AXIS2_PLACEMENT_3D ( 'NONE', #15422, #3582, #8431 ) ;
#1132 = AXIS2_PLACEMENT_3D ( 'NONE', #11394, #25726, #23672 ) ;
#1133 = ORIENTED_EDGE ( 'NONE', *, *, #18687, .F. ) ;
#1134 = DIRECTION ( 'NONE',  ( 1.000000000000000000, 0.000000000000000000, 0.000000000000000000 ) ) ;
#1135 = VECTOR ( 'NONE', #24120, 1000.000000000000000 ) ;
#1136 = CARTESIAN_POINT ( 'NONE',  ( -19.94474618696874302, 1.485631111656367853, 19.48477075383299706 ) ) ;
#1137 = EDGE_LOOP ( 'NONE', ( #14626, #9572, #10175, #26189 ) ) ;
#1138 = CARTESIAN_POINT ( 'NONE',  ( -24.03057240117691862, -26.57182937991349903, 1.500000000000000000 ) ) ;
#1139 = CARTESIAN_POINT ( 'NONE',  ( 13.00588823433103158, 48.28207767711727882, -62.53610571320827916 ) ) ;
#1140 = CARTESIAN_POINT ( 'NONE',  ( 10.18506332983505303, 29.04537757311072710, 1.500000000000000000 ) ) ;
#1141 = CARTESIAN_POINT ( 'NONE',  ( -34.21431199717225979, 20.40874709909905604, 8.143388502677929353 ) ) ;
#1142 = DIRECTION ( 'NONE',  ( 0.000000000000000000, 0.000000000000000000, 1.000000000000000000 ) ) ;
#1143 = CARTESIAN_POINT ( 'NONE',  ( 6.899999999999999467, 9.000000000000000000, 0.000000000000000000 ) ) ;
#1144 = FACE_OUTER_BOUND ( 'NONE', #21557, .T. ) ;
#1145 = CARTESIAN_POINT ( 'NONE',  ( 14.84769773172387985, 13.42619037096054591, 20.34789198813115263 ) ) ;
#1146 = CYLINDRICAL_SURFACE ( 'NONE', #13138, 0.7441270634457181066 ) ;
#1147 = VERTEX_POINT ( 'NONE', #6092 ) ;
#1148 = CARTESIAN_POINT ( 'NONE',  ( -11.13550902248300467, -16.63501148641496030, 20.05479082170252525 ) ) ;
#1149 = CARTESIAN_POINT ( 'NONE',  ( -17.77905984561984098, -9.199004478715986366, 7.441806358946449151 ) ) ;
#1150 = CARTESIAN_POINT ( 'NONE',  ( -5.423201226159623189, 16.15625638772824502, 5.651492010659114662 ) ) ;
#1151 = AXIS2_PLACEMENT_3D ( 'NONE', #10819, #20330, #13767 ) ;
#1152 = CARTESIAN_POINT ( 'NONE',  ( 11.93399590641349306, -16.07127689286907213, 6.447548852708279377 ) ) ;
#1153 = EDGE_CURVE ( 'NONE', #11716, #4151, #9442, .T. ) ;
#1154 = ADVANCED_FACE ( 'NONE', ( #1718 ), #25121, .F. ) ;
#1155 = AXIS2_PLACEMENT_3D ( 'NONE', #1770, #15808, #13644 ) ;
#1156 = CARTESIAN_POINT ( 'NONE',  ( -35.76344986165608475, 22.29344514668535027, -19.50000000000000355 ) ) ;
#1157 = DIRECTION ( 'NONE',  ( -1.000000000000000000, 0.000000000000000000, 0.000000000000000000 ) ) ;
#1158 = ORIENTED_EDGE ( 'NONE', *, *, #15067, .F. ) ;
#1159 = ADVANCED_FACE ( 'NONE', ( #13126 ), #5948, .F. ) ;
#1160 = ORIENTED_EDGE ( 'NONE', *, *, #25599, .T. ) ;
#1161 = DIRECTION ( 'NONE',  ( -0.000000000000000000, -0.000000000000000000, 1.000000000000000000 ) ) ;
#1162 = CARTESIAN_POINT ( 'NONE',  ( 10.11202017158399968, 41.14070756921128691, -1.500000000000000000 ) ) ;
#1163 = CIRCLE ( 'NONE', #17097, 9.084132297865673777 ) ;
#1164 = CARTESIAN_POINT ( 'NONE',  ( -14.72475726066618407, 13.56098618572340442, 6.310736198168394928 ) ) ;
#1165 = ADVANCED_FACE ( 'NONE', ( #8741 ), #16133, .T. ) ;
#1166 = DIRECTION ( 'NONE',  ( 1.000000000000000000, 0.000000000000000000, 0.000000000000000000 ) ) ;
#1167 = ORIENTED_EDGE ( 'NONE', *, *, #6161, .F. ) ;
#1168 = CONTEXT_DEPENDENT_SHAPE_REPRESENTATION ( #14408, #17146 ) ;
#1169 = CARTESIAN_POINT ( 'NONE',  ( 24.35970437652574105, 13.37404834226503958, 42.96778633356035471 ) ) ;
#1170 = CARTESIAN_POINT ( 'NONE',  ( 5.374868878255610660, 44.10336124695606230, -19.50000000000000355 ) ) ;
#1171 = CARTESIAN_POINT ( 'NONE',  ( -9.356685943497543789, -14.22000274044912160, 6.974106381145714018 ) ) ;
#1172 = EDGE_CURVE ( 'NONE', #27927, #23361, #4939, .T. ) ;
#1173 = ORIENTED_EDGE ( 'NONE', *, *, #8480, .F. ) ;
#1174 = CARTESIAN_POINT ( 'NONE',  ( -10.82521593960875528, 5.400395169024524655, 1.500000000000001332 ) ) ;
#1175 = B_SPLINE_SURFACE_WITH_KNOTS ( 'NONE', 3, 1, ( 
 ( #26290, #11788 ),
 ( #9611, #5083 ),
 ( #21293, #28788 ),
 ( #7428, #21129 ),
 ( #7116, #16935 ),
 ( #16774, #4761 ),
 ( #21451, #26453 ),
 ( #16628, #14594 ),
 ( #28338, #9915 ),
 ( #12256, #12109 ),
 ( #19428, #24098 ),
 ( #25990, #4926 ),
 ( #21759, #2119 ),
 ( #26133, #399 ),
 ( #14443, #17084 ),
 ( #26611, #2439 ),
 ( #5238, #23945 ),
 ( #30648, #16474 ),
 ( #4619, #14268 ),
 ( #23787, #11960 ),
 ( #2591, #10382 ),
 ( #12886, #2903 ),
 ( #17403, #13035 ),
 ( #12725, #22065 ),
 ( #22525, #19727 ),
 ( #20039, #19896 ),
 ( #12421, #29097 ),
 ( #5542, #24409 ),
 ( #15044, #18287 ),
 ( #10531, #27808 ),
 ( #29413, #17551 ) ),
 .UNSPECIFIED., .F., .F., .F.,
 ( 4, 3, 3, 3, 3, 3, 3, 3, 3, 3, 4 ),
 ( 2, 2 ),
 ( 0.000000000000000000, 0.05425176834609614362, 0.1085332949128348518, 0.1623767749169379715, 0.2157504826133058717, 0.2688657508888169789, 0.3218907763505471364, 0.3749548578363334772, 0.4282048033836237666, 0.4818374082110496448, 0.4999999999131652384 ),
 ( 0.000000000000000000, 1.000000000000000000 ),
 .UNSPECIFIED. ) ;
#1176 = AXIS2_PLACEMENT_3D ( 'NONE', #4448, #24929, #1953 ) ;
#1177 = ADVANCED_FACE ( 'NONE', ( #4517, #28690, #28535, #7328, #20890, #16837, #14027, #23530, #16679, #2176, #11399, #13884 ), #7011, .F. ) ;
#1178 = CARTESIAN_POINT ( 'NONE',  ( 0.000000000000000000, 0.000000000000000000, 1.500000000000001332 ) ) ;
#1179 = CARTESIAN_POINT ( 'NONE',  ( -15.55309275218070830, -34.20504001467671884, 37.49999999988268229 ) ) ;
#1180 = ORIENTED_EDGE ( 'NONE', *, *, #8394, .T. ) ;
#1181 = DIRECTION ( 'NONE',  ( 0.000000000000000000, 0.000000000000000000, -1.000000000000000000 ) ) ;
#1182 = EDGE_CURVE ( 'NONE', #25305, #3669, #9352, .T. ) ;
#1183 = VECTOR ( 'NONE', #12787, 1000.000000000000000 ) ;
#1184 = AXIS2_PLACEMENT_3D ( 'NONE', #30275, #2035, #11412 ) ;
#1185 = LINE ( 'NONE', #5548, #28491 ) ;
#1186 = CARTESIAN_POINT ( 'NONE',  ( 16.74250988114177474, 3.198928528055117404, 18.34798005863078885 ) ) ;
#1187 = DIRECTION ( 'NONE',  ( 1.000000000000000000, 0.000000000000000000, 0.000000000000000000 ) ) ;
#1188 = VERTEX_POINT ( 'NONE', #2021 ) ;
#1189 = CYLINDRICAL_SURFACE ( 'NONE', #21253, 10.00000000000000178 ) ;
#1190 = DIRECTION ( 'NONE',  ( 0.000000000000000000, 0.000000000000000000, 1.000000000000000000 ) ) ;
#1191 = FACE_OUTER_BOUND ( 'NONE', #19568, .T. ) ;
#1192 = DIRECTION ( 'NONE',  ( -0.000000000000000000, 1.132880637372608986E-16, -1.000000000000000000 ) ) ;
#1193 = DIRECTION ( 'NONE',  ( 0.000000000000000000, 1.000000000000000000, 0.000000000000000000 ) ) ;
#1194 = DIRECTION ( 'NONE',  ( -0.000000000000000000, 1.132880637372608986E-16, -1.000000000000000000 ) ) ;
#1195 = CARTESIAN_POINT ( 'NONE',  ( -1.687027447297492211, -8.840471615930066918, -3.621320343559650379 ) ) ;
#1196 = DIRECTION ( 'NONE',  ( 1.000000000000000000, 0.000000000000000000, 0.000000000000000000 ) ) ;
#1197 = ORIENTED_EDGE ( 'NONE', *, *, #17988, .F. ) ;
#1198 = ADVANCED_FACE ( 'NONE', ( #30415 ), #16212, .F. ) ;
#1199 = EDGE_CURVE ( 'NONE', #24108, #2130, #15785, .T. ) ;
#1200 = ADVANCED_FACE ( 'NONE', ( #23844 ), #2488, .F. ) ;
#1201 = CARTESIAN_POINT ( 'NONE',  ( 33.26787633654601706, -9.290711110048576415, 40.45924760685198862 ) ) ;
#1202 = FACE_OUTER_BOUND ( 'NONE', #13290, .T. ) ;
#1203 = VERTEX_POINT ( 'NONE', #29467 ) ;
#1204 = ADVANCED_FACE ( 'NONE', ( #746 ), #459, .F. ) ;
#1205 = ORIENTED_EDGE ( 'NONE', *, *, #1997, .F. ) ;
#1206 = FACE_OUTER_BOUND ( 'NONE', #15379, .T. ) ;
#1207 = CIRCLE ( 'NONE', #5672, 0.7500000000000011102 ) ;
#1208 = CARTESIAN_POINT ( 'NONE',  ( 25.19442432473618254, -35.44676296258426618, -19.50000000000000355 ) ) ;
#1209 = CARTESIAN_POINT ( 'NONE',  ( -8.795879380940579750, -2.270234684139648795, 13.22130136205108819 ) ) ;
#1210 = EDGE_CURVE ( 'NONE', #27501, #29565, #30630, .T. ) ;
#1211 = ORIENTED_EDGE ( 'NONE', *, *, #13206, .F. ) ;
#1212 = DIRECTION ( 'NONE',  ( 1.000000000000000000, 0.000000000000000000, 0.000000000000000000 ) ) ;
#1213 = CARTESIAN_POINT ( 'NONE',  ( 9.031466002702407181, -14.42835478804157390, 19.08155846658118904 ) ) ;
#1214 = ADVANCED_FACE ( 'NONE', ( #7629 ), #12629, .T. ) ;
#1215 = ADVANCED_FACE ( 'NONE', ( #8102 ), #291, .T. ) ;
#1216 = ORIENTED_EDGE ( 'NONE', *, *, #25747, .F. ) ;
#1217 = ORIENTED_EDGE ( 'NONE', *, *, #11109, .T. ) ;
#1218 = CARTESIAN_POINT ( 'NONE',  ( -4.163336342344337027E-14, 1.387778780781445676E-14, 37.50000000000000000 ) ) ;
#1219 = CARTESIAN_POINT ( 'NONE',  ( 17.92140030663551187, -8.878400182913017247, 6.913388067999403752 ) ) ;
#1220 = CARTESIAN_POINT ( 'NONE',  ( -5.881244434206279514, -6.812559277181949646, -1.500000000000002665 ) ) ;
#1221 = FACE_BOUND ( 'NONE', #816, .T. ) ;
#1222 = VERTEX_POINT ( 'NONE', #12775 ) ;
#1223 = CARTESIAN_POINT ( 'NONE',  ( -4.573988094335678767, 16.39521158297133852, 19.41069149716888020 ) ) ;
#1224 = EDGE_LOOP ( 'NONE', ( #18742, #29323, #2067, #24627 ) ) ;
#1225 = ORIENTED_EDGE ( 'NONE', *, *, #15509, .T. ) ;
#1226 = AXIS2_PLACEMENT_3D ( 'NONE', #23821, #14627, #4503 ) ;
#1227 = LINE ( 'NONE', #6051, #29164 ) ;
#1228 = ADVANCED_FACE ( 'NONE', ( #29312 ), #600, .F. ) ;
#1229 = CARTESIAN_POINT ( 'NONE',  ( -24.35970437652574105, 13.37404834226503247, 42.96778633356043287 ) ) ;
#1230 = CARTESIAN_POINT ( 'NONE',  ( 16.70510464924394967, 3.421819763545496773, 5.678370764302467677 ) ) ;
#1231 = PLANE ( 'NONE',  #10135 ) ;
#1232 = EDGE_CURVE ( 'NONE', #6203, #13370, #19780, .T. ) ;
#1233 = DIRECTION ( 'NONE',  ( 1.000000000000000000, 0.000000000000000000, 0.000000000000000000 ) ) ;
#1234 = CARTESIAN_POINT ( 'NONE',  ( -19.64177907938615064, -36.71644397333972876, 24.50000000000000000 ) ) ;
#1235 = DIRECTION ( 'NONE',  ( 1.000000000000000000, 0.000000000000000000, 0.000000000000000000 ) ) ;
#1236 = FACE_OUTER_BOUND ( 'NONE', #7384, .T. ) ;
#1237 = ORIENTED_EDGE ( 'NONE', *, *, #20788, .T. ) ;
#1238 = CARTESIAN_POINT ( 'NONE',  ( 0.000000000000000000, 0.000000000000000000, 82.49999999999998579 ) ) ;
#1239 = FACE_OUTER_BOUND ( 'NONE', #5088, .T. ) ;
#1240 = DIRECTION ( 'NONE',  ( 0.000000000000000000, 0.000000000000000000, 1.000000000000000000 ) ) ;
#1241 = ORIENTED_EDGE ( 'NONE', *, *, #23033, .F. ) ;
#1242 = VERTEX_POINT ( 'NONE', #7485 ) ;
#1243 = CARTESIAN_POINT ( 'NONE',  ( 49.45745851869548204, 69.99439104891119712, 19.18218888609259665 ) ) ;
#1244 = FACE_OUTER_BOUND ( 'NONE', #9042, .T. ) ;
#1245 = CARTESIAN_POINT ( 'NONE',  ( -4.718303904200451981, 16.35736724179926682, 7.176035686813569292 ) ) ;
#1246 = ORIENTED_EDGE ( 'NONE', *, *, #13192, .F. ) ;
#1247 = DIRECTION ( 'NONE',  ( 0.000000000000000000, 1.132880637372608986E-16, -1.000000000000000000 ) ) ;
#1248 = FACE_OUTER_BOUND ( 'NONE', #28914, .T. ) ;
#1249 = AXIS2_PLACEMENT_3D ( 'NONE', #11598, #19076, #21091 ) ;
#1250 = CARTESIAN_POINT ( 'NONE',  ( 0.8038475772933646457, 5.196152422706634688, -9.000000000000001776 ) ) ;
#1251 = EDGE_LOOP ( 'NONE', ( #20084, #3933, #13079, #18206 ) ) ;
#1252 = LINE ( 'NONE', #3268, #8766 ) ;
#1253 = CARTESIAN_POINT ( 'NONE',  ( 11.67039530559479843, 12.46804495696167692, 6.447548852708279377 ) ) ;
#1254 = CARTESIAN_POINT ( 'NONE',  ( 16.82340201860978368, 2.653416696629036675, 7.500898271101006820 ) ) ;
#1255 = VERTEX_POINT ( 'NONE', #2637 ) ;
#1256 = CARTESIAN_POINT ( 'NONE',  ( 15.31102578509455903, 12.89549683364648835, 5.862424720655265098 ) ) ;
#1257 = ORIENTED_EDGE ( 'NONE', *, *, #26177, .F. ) ;
#1258 = CYLINDRICAL_SURFACE ( 'NONE', #28879, 9.482273699623480212 ) ;
#1259 = AXIS2_PLACEMENT_3D ( 'NONE', #19682, #29205, #29053 ) ;
#1260 = LINE ( 'NONE', #29338, #27317 ) ;
#1261 = ORIENTED_EDGE ( 'NONE', *, *, #10902, .T. ) ;
#1262 = EDGE_LOOP ( 'NONE', ( #5349, #15850, #2816 ) ) ;
#1263 = CARTESIAN_POINT ( 'NONE',  ( 5.159688198573268991, 19.34150021954530274, 7.643931100913408550 ) ) ;
#1264 = EDGE_CURVE ( 'NONE', #6747, #8400, #30302, .T. ) ;
#1265 = LINE ( 'NONE', #18424, #21036 ) ;
#1266 = CARTESIAN_POINT ( 'NONE',  ( 6.262045289545328686, 18.99438835075423881, 19.21471108562414543 ) ) ;
#1267 = AXIS2_PLACEMENT_3D ( 'NONE', #10644, #30128, #8758 ) ;
#1268 = CARTESIAN_POINT ( 'NONE',  ( -35.76481447503398670, -5.202797454133643917, 34.80090346875804386 ) ) ;
#1269 = CARTESIAN_POINT ( 'NONE',  ( 30.33183837007556249, 13.53414739637283226, -16.55003854064094426 ) ) ;
#1270 = CARTESIAN_POINT ( 'NONE',  ( 16.86926274317444552, 2.283828795636141162, 19.77662771831109367 ) ) ;
#1271 = ORIENTED_EDGE ( 'NONE', *, *, #17391, .F. ) ;
#1272 = DIRECTION ( 'NONE',  ( -0.000000000000000000, 0.000000000000000000, 1.000000000000000000 ) ) ;
#1273 = CARTESIAN_POINT ( 'NONE',  ( 15.54925513364909939, -6.943479002078030149, 7.429667576816606278 ) ) ;
#1274 = CARTESIAN_POINT ( 'NONE',  ( -13.97362136398187538, 9.814707526993059261, 19.69140814234746273 ) ) ;
#1275 = CARTESIAN_POINT ( 'NONE',  ( -4.163336342344337027E-14, -1.387778780781445676E-14, 1.500000000000000000 ) ) ;
#1276 = ORIENTED_EDGE ( 'NONE', *, *, #27924, .F. ) ;
#1277 = ORIENTED_EDGE ( 'NONE', *, *, #5949, .F. ) ;
#1278 = CARTESIAN_POINT ( 'NONE',  ( 31.30424506559346298, -25.35202612174932568, 8.284888684157436956 ) ) ;
#1279 = CARTESIAN_POINT ( 'NONE',  ( 9.864937699929955173, -13.90063973435163724, 5.652196082368482699 ) ) ;
#1280 = B_SPLINE_CURVE_WITH_KNOTS ( 'NONE', 3,
 ( #2307, #12145, #11993, #11834, #4507, #21164, #4800, #28524, #26026, #24132, #7155, #9957, #441, #2624 ),
 .UNSPECIFIED., .F., .F.,
 ( 4, 2, 2, 2, 2, 2, 4 ),
 ( 2.108610145898612731E-07, 0.0004867403503157787643, 0.0009732698396169676622, 0.001459799328918156506, 0.001946328818219345350, 0.002919387796821717399, 0.003892446775424089015 ),
 .UNSPECIFIED. ) ;
#1281 = CARTESIAN_POINT ( 'NONE',  ( -5.865338193562683600, 19.13956943172006220, 20.34789198813115263 ) ) ;
#1282 = LINE ( 'NONE', #15460, #19231 ) ;
#1283 = DIRECTION ( 'NONE',  ( 0.000000000000000000, 0.000000000000000000, -1.000000000000000000 ) ) ;
#1284 = DIRECTION ( 'NONE',  ( -1.000000000000000000, 0.000000000000000000, 0.000000000000000000 ) ) ;
#1285 = CARTESIAN_POINT ( 'NONE',  ( 19.84998497291395125, 36.59036391654254317, 29.38252776222237372 ) ) ;
#1286 = VERTEX_POINT ( 'NONE', #28994 ) ;
#1287 = CARTESIAN_POINT ( 'NONE',  ( -33.51229671200703564, -9.872960191568498800, 35.82118098709739940 ) ) ;
#1288 = CARTESIAN_POINT ( 'NONE',  ( -33.48612972047447300, 10.91418318924902131, 39.78046893947538365 ) ) ;
#1289 = CARTESIAN_POINT ( 'NONE',  ( 8.840471615930072247, -1.687027447297460236, 21.50000000000000000 ) ) ;
#1290 = VERTEX_POINT ( 'NONE', #3249 ) ;
#1291 = CIRCLE ( 'NONE', #19710, 1.000000000000008660 ) ;
#1292 = VERTEX_POINT ( 'NONE', #17293 ) ;
#1293 = DIRECTION ( 'NONE',  ( 0.000000000000000000, -0.000000000000000000, -1.000000000000000000 ) ) ;
#1294 = VECTOR ( 'NONE', #26040, 1000.000000000000000 ) ;
#1295 = ORIENTED_EDGE ( 'NONE', *, *, #22144, .F. ) ;
#1296 = CARTESIAN_POINT ( 'NONE',  ( 9.743151247090292344, -38.04912300944125292, 27.50000000000000000 ) ) ;
#1297 = CARTESIAN_POINT ( 'NONE',  ( 14.87689969681335178, 47.73552663251712147, -56.98063042392984556 ) ) ;
#1298 = CARTESIAN_POINT ( 'NONE',  ( -6.192647045995789412, -41.97176936070047049, 20.15864424522374065 ) ) ;
#1299 = CARTESIAN_POINT ( 'NONE',  ( -37.98074266006555888, 9.653107878580014400, 13.30882976141995222 ) ) ;
#1300 = CARTESIAN_POINT ( 'NONE',  ( -24.98398214727286515, 23.12412086524405908, -16.50001200000000523 ) ) ;
#1301 = AXIS2_PLACEMENT_3D ( 'NONE', #4447, #20953, #23150 ) ;
#1302 = CARTESIAN_POINT ( 'NONE',  ( -12.33859880789482233, 8.132258305203423632, -1.500000000000000000 ) ) ;
#1303 = DIRECTION ( 'NONE',  ( 1.000000000000000000, 0.000000000000000000, 0.000000000000000000 ) ) ;
#1304 = ORIENTED_EDGE ( 'NONE', *, *, #26374, .T. ) ;
#1305 = CARTESIAN_POINT ( 'NONE',  ( -8.835414383224243551, -14.56605378991199196, 20.29090034784956131 ) ) ;
#1306 = CARTESIAN_POINT ( 'NONE',  ( -0.8750451464063155882, -9.041888939645136958, 13.22130136205108641 ) ) ;
#1307 = CARTESIAN_POINT ( 'NONE',  ( -24.44496207165490276, -7.595930209050158588, 49.40206402021039622 ) ) ;
#1308 = AXIS2_PLACEMENT_3D ( 'NONE', #17106, #19296, #2769 ) ;
#1309 = B_SPLINE_CURVE_WITH_KNOTS ( 'NONE', 3,
 ( #28103, #25755, #20466, #11254 ),
 .UNSPECIFIED., .F., .F.,
 ( 4, 4 ),
 ( 3.022186913359086288E-07, 0.007932103869840195776 ),
 .UNSPECIFIED. ) ;
#1310 = CARTESIAN_POINT ( 'NONE',  ( -35.78163722268750746, -27.43648963448195133, -11.49999999999999645 ) ) ;
#1311 = CARTESIAN_POINT ( 'NONE',  ( 35.76344986163714168, -22.29344514668044752, -19.50000000000000355 ) ) ;
#1312 = AXIS2_PLACEMENT_3D ( 'NONE', #15629, #1609, #6117 ) ;
#1313 = DIRECTION ( 'NONE',  ( 1.000000000000000000, 0.000000000000000000, 0.000000000000000000 ) ) ;
#1314 = VERTEX_POINT ( 'NONE', #19950 ) ;
#1315 = ORIENTED_EDGE ( 'NONE', *, *, #26545, .T. ) ;
#1316 = LINE ( 'NONE', #30013, #9536 ) ;
#1317 = CARTESIAN_POINT ( 'NONE',  ( -5.105024945675580739, -42.22604126506273303, -1.500000000000000000 ) ) ;
#1318 = FACE_OUTER_BOUND ( 'NONE', #10044, .T. ) ;
#1319 = DIRECTION ( 'NONE',  ( 0.000000000000000000, 0.000000000000000000, -1.000000000000000000 ) ) ;
#1320 = ORIENTED_EDGE ( 'NONE', *, *, #3335, .T. ) ;
#1321 = CARTESIAN_POINT ( 'NONE',  ( 27.86235613436985759, 14.72519157938689460, 39.24389099736750808 ) ) ;
#1322 = FACE_OUTER_BOUND ( 'NONE', #29141, .T. ) ;
#1323 = CARTESIAN_POINT ( 'NONE',  ( -9.389232999038370053, -14.19758896559616979, 6.530762810602277924 ) ) ;
#1324 = ORIENTED_EDGE ( 'NONE', *, *, #21960, .T. ) ;
#1325 = CARTESIAN_POINT ( 'NONE',  ( -8.550548372801090480, -14.74545326687210434, 20.34789198813115263 ) ) ;
#1326 = CARTESIAN_POINT ( 'NONE',  ( -11.70595374688322821, -40.54787758647957219, 34.56692815348143455 ) ) ;
#1327 = EDGE_CURVE ( 'NONE', #25485, #25063, #15100, .T. ) ;
#1328 = ORIENTED_EDGE ( 'NONE', *, *, #17743, .T. ) ;
#1329 = DIRECTION ( 'NONE',  ( -1.000000000000000000, 0.000000000000000000, 0.000000000000000000 ) ) ;
#1330 = CIRCLE ( 'NONE', #18761, 9.084132297865673777 ) ;
#1331 = VECTOR ( 'NONE', #23455, 1000.000000000000000 ) ;
#1332 = CARTESIAN_POINT ( 'NONE',  ( 26.80246859415415273, -7.028748154183637631, -16.50000000000000000 ) ) ;
#1333 = CIRCLE ( 'NONE', #4815, 0.7500000000000006661 ) ;
#1334 = CARTESIAN_POINT ( 'NONE',  ( 31.89304216768362821, -14.79375299452194348, 39.84323675255973995 ) ) ;
#1335 = PLANE ( 'NONE',  #29203 ) ;
#1336 = ORIENTED_EDGE ( 'NONE', *, *, #9963, .T. ) ;
#1337 = DIRECTION ( 'NONE',  ( 0.000000000000000000, -1.132880637372608986E-16, 1.000000000000000000 ) ) ;
#1338 = CARTESIAN_POINT ( 'NONE',  ( 12.98116905410817523, 11.01127998639621275, 19.66962785902261146 ) ) ;
#1339 = CARTESIAN_POINT ( 'NONE',  ( 16.12178322344232129, -5.613588367463943740, 6.037360021877315575 ) ) ;
#1340 = ADVANCED_FACE ( 'NONE', ( #14794 ), #21656, .F. ) ;
#1341 = CARTESIAN_POINT ( 'NONE',  ( -22.95669091611927826, -27.54300778121952220, 1.500000000000000000 ) ) ;
#1342 = CARTESIAN_POINT ( 'NONE',  ( -17.05006382469673198, 0.8465830298419860789, 7.269896094239230777 ) ) ;
#1343 = B_SPLINE_CURVE_WITH_KNOTS ( 'NONE', 3,
 ( #28708, #11874, #19499, #9676, #12175, #21673, #26843, #5148, #14659, #4840, #24161, #2813, #12336, #26205, #17153, #7650, #26672, #19039, #19641, #2509, #29011, #23697, #14510, #28553, #4998, #309, #9, #155, #7799, #14355, #12023, #7185, #23865, #21836 ),
 .UNSPECIFIED., .F., .F.,
 ( 4, 2, 2, 2, 2, 2, 2, 2, 2, 2, 2, 2, 2, 2, 2, 2, 4 ),
 ( 0.1877422973930296390, 0.1907727015327729259, 0.1938031056725162127, 0.1998639139520027586, 0.2028943180917460454, 0.2044095201616177027, 0.2059247222314893322, 0.2119855305109759058, 0.2150159346507191649, 0.2165311367205908222, 0.2180463387904624517, 0.2241071470699490531, 0.2271375512096923677, 0.2286527532795639972, 0.2301679553494356545, 0.2331983594891789413, 0.2362287636289222559 ),
 .UNSPECIFIED. ) ;
#1344 = CARTESIAN_POINT ( 'NONE',  ( 0.000000000000000000, 8.021365865836055733E-32, -87.50000000000000000 ) ) ;
#1345 = CARTESIAN_POINT ( 'NONE',  ( 4.608906612435600181, 7.730328572437758616, 1.500000000000001332 ) ) ;
#1346 = AXIS2_PLACEMENT_3D ( 'NONE', #18219, #6660, #16178 ) ;
#1347 = LINE ( 'NONE', #3692, #2454 ) ;
#1348 = CARTESIAN_POINT ( 'NONE',  ( 9.031466002689079176, -14.42835478804960303, 6.385774490351133537 ) ) ;
#1349 = LINE ( 'NONE', #8378, #16772 ) ;
#1350 = CARTESIAN_POINT ( 'NONE',  ( -8.978548835276082940, -14.47379921341572562, 20.22273502201483097 ) ) ;
#1351 = CONICAL_SURFACE ( 'NONE', #5825, 9.000000000000000000, 1.047197551196600296 ) ;
#1352 = VERTEX_POINT ( 'NONE', #5606 ) ;
#1353 = ORIENTED_EDGE ( 'NONE', *, *, #8218, .F. ) ;
#1355 = ADVANCED_FACE ( 'NONE', ( #21970 ), #24617, .F. ) ;
#1354 = VECTOR ( 'NONE', #16103, 1000.000000000000000 ) ;
#1356 = DIRECTION ( 'NONE',  ( -1.000000000000000000, 0.000000000000000000, 0.000000000000000000 ) ) ;
#1357 = CARTESIAN_POINT ( 'NONE',  ( -40.89187623478217404, 5.790488632116478129, -19.50000000000000355 ) ) ;
#1358 = DIRECTION ( 'NONE',  ( 1.000000000000000000, 0.000000000000000000, 0.000000000000000000 ) ) ;
#1359 = AXIS2_PLACEMENT_3D ( 'NONE', #12045, #21538, #28424 ) ;
#1360 = ORIENTED_EDGE ( 'NONE', *, *, #7124, .F. ) ;
#1361 =( LENGTH_UNIT ( ) NAMED_UNIT ( * ) SI_UNIT ( .MILLI., .METRE. ) );
#1362 = CARTESIAN_POINT ( 'NONE',  ( 23.27838111857050407, -36.10018641471199174, -16.50000599999999906 ) ) ;
#1363 = CARTESIAN_POINT ( 'NONE',  ( 9.640932123821245980, -14.04859418178019759, 20.32222155561918697 ) ) ;
#1364 = VERTEX_POINT ( 'NONE', #5132 ) ;
#1365 = EDGE_LOOP ( 'NONE', ( #17122, #18661, #20473, #30492 ) ) ;
#1366 = CARTESIAN_POINT ( 'NONE',  ( 15.94288127717318915, -6.058927977062414705, 20.29915277494337644 ) ) ;
#1367 = CIRCLE ( 'NONE', #19785, 0.7500000000000006661 ) ;
#1368 = CARTESIAN_POINT ( 'NONE',  ( 16.70665413472816496, 3.412884783584985815, 20.32367522806703874 ) ) ;
#1369 = AXIS2_PLACEMENT_3D ( 'NONE', #4710, #21541, #14681 ) ;
#1370 = CARTESIAN_POINT ( 'NONE',  ( -10.62006778255435613, -16.96839658127461803, 18.35377592296120497 ) ) ;
#1371 = CARTESIAN_POINT ( 'NONE',  ( -5.974369479646943759, 42.02548368003539991, 34.60052964640640738 ) ) ;
#1372 = ORIENTED_EDGE ( 'NONE', *, *, #17855, .F. ) ;
#1373 = CARTESIAN_POINT ( 'NONE',  ( -5.544451647051928944, 16.11829164193971664, 20.34789198813115263 ) ) ;
#1374 = ADVANCED_FACE ( 'NONE', ( #920 ), #26827, .T. ) ;
#1375 = VERTEX_POINT ( 'NONE', #14486 ) ;
#1376 = VECTOR ( 'NONE', #15752, 1000.000000000000000 ) ;
#1377 = EDGE_CURVE ( 'NONE', #14465, #15390, #21818, .T. ) ;
#1378 = CARTESIAN_POINT ( 'NONE',  ( 24.03057240117691862, -26.57182937991349903, -6.500000000000000888 ) ) ;
#1379 = CARTESIAN_POINT ( 'NONE',  ( -16.84831847207179223, 2.450595477917709264, 19.96344307082652492 ) ) ;
#1380 = ORIENTED_EDGE ( 'NONE', *, *, #22384, .F. ) ;
#1381 = AXIS2_PLACEMENT_3D ( 'NONE', #28177, #18216, #23028 ) ;
#1382 = EDGE_CURVE ( 'NONE', #4772, #14537, #29775, .T. ) ;
#1383 = ADVANCED_FACE ( 'NONE', ( #20409, #22433, #24933, #13410, #30077, #1076, #24770, #15720, #11202, #3569, #10909, #15409 ), #29618, .T. ) ;
#1384 = CARTESIAN_POINT ( 'NONE',  ( 12.58101777923778997, -40.23389158998374171, 29.03989791324179848 ) ) ;
#1385 = CARTESIAN_POINT ( 'NONE',  ( 19.57830992477560272, 4.170884463583997892, 6.892848776733236704 ) ) ;
#1386 = CARTESIAN_POINT ( 'NONE',  ( -13.16299300229363567, 10.81582545713520638, 18.39701043959520987 ) ) ;
#1387 = AXIS2_PLACEMENT_3D ( 'NONE', #12324, #3117, #21827 ) ;
#1388 = CARTESIAN_POINT ( 'NONE',  ( 1.307979816591920308, -17.01201364160250051, 5.759928666072750225 ) ) ;
#1389 = EDGE_CURVE ( 'NONE', #6566, #2038, #8416, .T. ) ;
#1390 = CARTESIAN_POINT ( 'NONE',  ( 16.74328841314636662, 3.194145055459935545, 20.34789198813115263 ) ) ;
#1391 = DIRECTION ( 'NONE',  ( 0.000000000000000000, 0.000000000000000000, 1.000000000000000000 ) ) ;
#1392 = CARTESIAN_POINT ( 'NONE',  ( 9.749114229549594057, -0.1262659238204522361, 1.500000000000001332 ) ) ;
#1393 = ORIENTED_EDGE ( 'NONE', *, *, #9979, .F. ) ;
#1394 = AXIS2_PLACEMENT_3D ( 'NONE', #19673, #26872, #10321 ) ;
#1395 = EDGE_CURVE ( 'NONE', #29287, #2154, #4898, .T. ) ;
#1396 = CIRCLE ( 'NONE', #28285, 1.000000000000004441 ) ;
#1397 = CARTESIAN_POINT ( 'NONE',  ( 8.860628911697515875, 8.184276679720483116, 1.500000000000000000 ) ) ;
#1398 = CARTESIAN_POINT ( 'NONE',  ( 35.99999999999999289, -2.601438916704202242, 34.80090346875810070 ) ) ;
#1399 = AXIS2_PLACEMENT_3D ( 'NONE', #12089, #14577, #5219 ) ;
#1400 = ORIENTED_EDGE ( 'NONE', *, *, #2774, .T. ) ;
#1401 = ORIENTED_EDGE ( 'NONE', *, *, #20994, .F. ) ;
#1402 = ADVANCED_FACE ( 'NONE', ( #8251, #17927, #1686 ), #10739, .T. ) ;
#1403 = CARTESIAN_POINT ( 'NONE',  ( 49.99999999999998579, 70.00000000000001421, 21.82070150977413903 ) ) ;
#1404 = CYLINDRICAL_SURFACE ( 'NONE', #3158, 0.7500000000000007772 ) ;
#1405 = CARTESIAN_POINT ( 'NONE',  ( -5.147812317479952604, 19.34466387292043876, 7.176035686813569292 ) ) ;
#1406 = ORIENTED_EDGE ( 'NONE', *, *, #6377, .F. ) ;
#1407 = DIRECTION ( 'NONE',  ( 0.000000000000000000, 0.000000000000000000, 1.000000000000000000 ) ) ;
#1408 = CIRCLE ( 'NONE', #17835, 27.70876437800068359 ) ;
#1409 = DIRECTION ( 'NONE',  ( 0.000000000000000000, 1.132880637372608986E-16, -1.000000000000000000 ) ) ;
#1410 = DIRECTION ( 'NONE',  ( -0.000000000000000000, -0.000000000000000000, 1.000000000000000000 ) ) ;
#1411 = ORIENTED_EDGE ( 'NONE', *, *, #14365, .T. ) ;
#1412 = CARTESIAN_POINT ( 'NONE',  ( 24.44496207165490276, -7.595930209050162141, -16.55003854064094426 ) ) ;
#1413 = CARTESIAN_POINT ( 'NONE',  ( -10.18506332983504237, -29.04537757311072710, 1.500000000000000000 ) ) ;
#1414 = CARTESIAN_POINT ( 'NONE',  ( -33.43088607478084384, -9.613432587296607323, 40.21452297281935984 ) ) ;
#1415 = ORIENTED_EDGE ( 'NONE', *, *, #25806, .F. ) ;
#1416 = LINE ( 'NONE', #3591, #23261 ) ;
#1417 = EDGE_CURVE ( 'NONE', #22306, #24939, #17759, .T. ) ;
#1418 = EDGE_LOOP ( 'NONE', ( #23104, #19972, #12540, #30228 ) ) ;
#1419 =( GEOMETRIC_REPRESENTATION_CONTEXT ( 3 ) GLOBAL_UNCERTAINTY_ASSIGNED_CONTEXT ( ( #17991 ) ) GLOBAL_UNIT_ASSIGNED_CONTEXT ( ( #21477, #23197, #28368 ) ) REPRESENTATION_CONTEXT ( 'NONE', 'WORKASPACE' ) );
#1420 = CARTESIAN_POINT ( 'NONE',  ( -2.270234684139619485, 8.795879380940585079, 21.50000000000000000 ) ) ;
#1421 = ADVANCED_FACE ( 'NONE', ( #4031 ), #18074, .F. ) ;
#1422 = AXIS2_PLACEMENT_3D ( 'NONE', #15991, #2089, #3991 ) ;
#1423 = ORIENTED_EDGE ( 'NONE', *, *, #5801, .F. ) ;
#1424 = AXIS2_PLACEMENT_3D ( 'NONE', #10624, #13592, #15757 ) ;
#1425 = EDGE_CURVE ( 'NONE', #11023, #8165, #6059, .T. ) ;
#1426 = ORIENTED_EDGE ( 'NONE', *, *, #17426, .T. ) ;
#1427 = CYLINDRICAL_SURFACE ( 'NONE', #14286, 0.7441270634457319844 ) ;
#1428 = DIRECTION ( 'NONE',  ( -0.000000000000000000, -0.000000000000000000, -1.000000000000000000 ) ) ;
#1429 = CYLINDRICAL_SURFACE ( 'NONE', #20294, 20.00000000000000355 ) ;
#1430 = ORIENTED_EDGE ( 'NONE', *, *, #26299, .F. ) ;
#1431 = CARTESIAN_POINT ( 'NONE',  ( 9.676137610658589239, -14.02562811695956313, 18.36582235739946611 ) ) ;
#1432 = CARTESIAN_POINT ( 'NONE',  ( 19.76130408545751749, 3.194145055459935101, 20.34789198813115263 ) ) ;
#1433 = ORIENTED_EDGE ( 'NONE', *, *, #18979, .T. ) ;
#1434 = CARTESIAN_POINT ( 'NONE',  ( -26.80246859415415273, 7.028748154183637631, -16.50000000000000000 ) ) ;
#1435 = CARTESIAN_POINT ( 'NONE',  ( 17.97060409579513163, -8.818932628521070072, 6.211014596808754007 ) ) ;
#1436 = CYLINDRICAL_SURFACE ( 'NONE', #9348, 0.7499999999999997780 ) ;
#1437 = CARTESIAN_POINT ( 'NONE',  ( 4.982076346116049770, 19.38816267120398962, 20.29915277494337644 ) ) ;
#1438 = ORIENTED_EDGE ( 'NONE', *, *, #7875, .T. ) ;
#1439 = ORIENTED_EDGE ( 'NONE', *, *, #14389, .F. ) ;
#1440 = FACE_BOUND ( 'NONE', #28403, .T. ) ;
#1441 = B_SPLINE_SURFACE_WITH_KNOTS ( 'NONE', 3, 1, ( 
 ( #29652, #10011 ),
 ( #10154, #29183 ),
 ( #7990, #8289 ),
 ( #26541, #17333 ),
 ( #14675, #24179 ),
 ( #5642, #19983 ),
 ( #7669, #5485 ),
 ( #17171, #19826 ),
 ( #14987, #24499 ),
 ( #26692, #3145 ),
 ( #22161, #785 ),
 ( #22317, #17493 ),
 ( #24654, #3289 ),
 ( #959, #14833 ),
 ( #29501, #17645 ),
 ( #5789, #27780 ),
 ( #6247, #6091 ),
 ( #25439, #15602 ),
 ( #15756, #20444 ),
 ( #10777, #25277 ),
 ( #6558, #20889 ),
 ( #20291, #30414 ),
 ( #17805, #15927 ),
 ( #13281, #23220 ),
 ( #22775, #30259 ),
 ( #3603, #18430 ),
 ( #6409, #1431 ),
 ( #3925, #18108 ),
 ( #27623, #25120 ),
 ( #16070, #3762 ),
 ( #1874, #15445 ) ),
 .UNSPECIFIED., .F., .F., .F.,
 ( 4, 3, 3, 3, 3, 3, 3, 3, 3, 3, 4 ),
 ( 2, 2 ),
 ( 0.000000000000000000, 0.05425176834609614362, 0.1085332949128348518, 0.1623767749169379715, 0.2157504826133058717, 0.2688657508888169789, 0.3218907763505471364, 0.3749548578363334772, 0.4282048033836237666, 0.4818374082110496448, 0.4999999999131654604 ),
 ( 0.000000000000000000, 1.000000000000000000 ),
 .UNSPECIFIED. ) ;
#1442 = CARTESIAN_POINT ( 'NONE',  ( 66.99999999999998579, 50.00000000000000000, 59.49999999999999289 ) ) ;
#1443 =( LENGTH_UNIT ( ) NAMED_UNIT ( * ) SI_UNIT ( .MILLI., .METRE. ) );
#1444 = AXIS2_PLACEMENT_3D ( 'NONE', #23756, #17055, #24221 ) ;
#1445 = FACE_OUTER_BOUND ( 'NONE', #22621, .T. ) ;
#1446 = AXIS2_PLACEMENT_3D ( 'NONE', #152, #26052, #4684 ) ;
#1447 = CARTESIAN_POINT ( 'NONE',  ( 0.000000000000000000, -2.435693370351110282E-15, 21.50000000000000355 ) ) ;
#1448 = CYLINDRICAL_SURFACE ( 'NONE', #28363, 19.49999999999996447 ) ;
#1449 = ADVANCED_FACE ( 'NONE', ( #1236 ), #15568, .F. ) ;
#1450 = ORIENTED_EDGE ( 'NONE', *, *, #13936, .F. ) ;
#1451 = ADVANCED_FACE ( 'NONE', ( #8871 ), #6375, .F. ) ;
#1452 = CARTESIAN_POINT ( 'NONE',  ( -33.42925964089141644, -11.06161099612212695, 35.54550565580013455 ) ) ;
#1454 = EDGE_LOOP ( 'NONE', ( #21314, #26779, #24672, #6275 ) ) ;
#1453 = VECTOR ( 'NONE', #13826, 1000.000000000000000 ) ;
#1455 = CARTESIAN_POINT ( 'NONE',  ( -33.42925964089140933, 11.06161099612212695, 39.78814634291943264 ) ) ;
#1456 = CARTESIAN_POINT ( 'NONE',  ( -7.488956955540436056, -5.141690706682852330, -1.500000000000002442 ) ) ;
#1457 = EDGE_LOOP ( 'NONE', ( #8273, #15549, #9451, #27302 ) ) ;
#1458 = VERTEX_POINT ( 'NONE', #22735 ) ;
#1459 = CARTESIAN_POINT ( 'NONE',  ( -19.72672318758257148, 3.296256974645884075, 7.267242832833948007 ) ) ;
#1460 = CIRCLE ( 'NONE', #27926, 0.7441270634456903510 ) ;
#1461 = DIRECTION ( 'NONE',  ( -0.000000000000000000, -0.000000000000000000, 1.000000000000000000 ) ) ;
#1462 = ORIENTED_EDGE ( 'NONE', *, *, #19357, .F. ) ;
#1463 = CARTESIAN_POINT ( 'NONE',  ( 66.99999999999998579, 50.00000000000000000, 62.49999999999999289 ) ) ;
#1464 = CARTESIAN_POINT ( 'NONE',  ( 13.01460760711195519, 48.27982028891777588, -47.47714469611751298 ) ) ;
#1465 = DIRECTION ( 'NONE',  ( 1.000000000000000000, 0.000000000000000000, 0.000000000000000000 ) ) ;
#1466 = CARTESIAN_POINT ( 'NONE',  ( -22.85987860430571317, -23.19171692911513460, -16.50001200000000168 ) ) ;
#1467 = DIRECTION ( 'NONE',  ( -1.000000000000000000, 0.000000000000000000, 0.000000000000000000 ) ) ;
#1468 = AXIS2_PLACEMENT_3D ( 'NONE', #28004, #20963, #1806 ) ;
#1469 = DIRECTION ( 'NONE',  ( -1.000000000000000000, 0.000000000000000000, 0.000000000000000000 ) ) ;
#1470 = CARTESIAN_POINT ( 'NONE',  ( 1.082887659287353754, -19.98847979319445756, 5.951255046771932733 ) ) ;
#1471 = FACE_OUTER_BOUND ( 'NONE', #1058, .T. ) ;
#1472 = ORIENTED_EDGE ( 'NONE', *, *, #24991, .T. ) ;
#1473 = CIRCLE ( 'NONE', #23359, 2.061368542273053883 ) ;
#1474 = PLANE ( 'NONE',  #26220 ) ;
#1475 = LINE ( 'NONE', #15646, #18551 ) ;
#1476 = CARTESIAN_POINT ( 'NONE',  ( 10.22519205257000863, -13.65449557370669176, 7.559636331181775581 ) ) ;
#1477 = CARTESIAN_POINT ( 'NONE',  ( 2.687479362164894248, -44.39187623478217404, -19.50000000000000355 ) ) ;
#1478 = AXIS2_PLACEMENT_3D ( 'NONE', #12501, #7807, #4847 ) ;
#1479 = CARTESIAN_POINT ( 'NONE',  ( 49.99999999999998579, 50.00000000000000000, 12.49999999999999112 ) ) ;
#1480 = ORIENTED_EDGE ( 'NONE', *, *, #24394, .F. ) ;
#1481 = CARTESIAN_POINT ( 'NONE',  ( 0.000000000000000000, -7.794228634059938265, -4.500000000000013323 ) ) ;
#1482 = CARTESIAN_POINT ( 'NONE',  ( -39.83602371821034183, 11.57901747687032490, -19.50000000000000355 ) ) ;
#1483 = CARTESIAN_POINT ( 'NONE',  ( 35.71656808851346199, -17.11898487263705704, 31.35097916509175420 ) ) ;
#1484 = CARTESIAN_POINT ( 'NONE',  ( 24.03057240117691862, 26.57182937991349903, -6.499999999999999112 ) ) ;
#1485 = EDGE_LOOP ( 'NONE', ( #14703, #24943, #18019, #16923 ) ) ;
#1486 = FACE_OUTER_BOUND ( 'NONE', #16197, .T. ) ;
#1487 = EDGE_CURVE ( 'NONE', #29934, #18617, #5750, .T. ) ;
#1488 = CARTESIAN_POINT ( 'NONE',  ( 39.00000000000000000, -5.563236990218592304, -1.500000000000000000 ) ) ;
#1489 = EDGE_CURVE ( 'NONE', #8853, #24056, #20553, .T. ) ;
#1490 = LINE ( 'NONE', #21948, #12448 ) ;
#1491 = ADVANCED_FACE ( 'NONE', ( #27743 ), #18226, .T. ) ;
#1492 = ORIENTED_EDGE ( 'NONE', *, *, #28292, .F. ) ;
#1493 = CIRCLE ( 'NONE', #9942, 0.7500000000000006661 ) ;
#1494 = LINE ( 'NONE', #25341, #4870 ) ;
#1495 = CARTESIAN_POINT ( 'NONE',  ( 19.58194293052861212, 4.068188588073703649, 18.84486140012300126 ) ) ;
#1496 = ORIENTED_EDGE ( 'NONE', *, *, #13412, .F. ) ;
#1497 = CARTESIAN_POINT ( 'NONE',  ( -31.10273980501929003, -15.38400267427140022, 40.30072466179765911 ) ) ;
#1498 = CIRCLE ( 'NONE', #2484, 0.7500000000000011102 ) ;
#1499 = LINE ( 'NONE', #27688, #26304 ) ;
#1500 = DIRECTION ( 'NONE',  ( 0.000000000000000000, -1.132880637372608986E-16, 1.000000000000000000 ) ) ;
#1501 = ORIENTED_EDGE ( 'NONE', *, *, #17776, .F. ) ;
#1502 = CARTESIAN_POINT ( 'NONE',  ( 12.00027744594693324, 12.12900492880153891, 18.45571264222803975 ) ) ;
#1503 = DIRECTION ( 'NONE',  ( 0.000000000000000000, 0.000000000000000000, -1.000000000000000000 ) ) ;
#1504 = CARTESIAN_POINT ( 'NONE',  ( 0.8643805006890388221, -19.98168094404549322, 18.47531940416305929 ) ) ;
#1505 = LINE ( 'NONE', #11014, #27746 ) ;
#1506 = CARTESIAN_POINT ( 'NONE',  ( -16.99797872337272153, 1.390050218453713349, 7.652108011868849147 ) ) ;
#1507 = DIRECTION ( 'NONE',  ( 0.000000000000000000, 0.000000000000000000, -1.000000000000000000 ) ) ;
#1508 = FACE_OUTER_BOUND ( 'NONE', #28742, .T. ) ;
#1509 = CARTESIAN_POINT ( 'NONE',  ( 1.687027447297431371, 8.840471615930075799, -3.621320343559650379 ) ) ;
#1510 = CARTESIAN_POINT ( 'NONE',  ( -16.69721919944057831, 13.88429941593312122, 1.500000000000000000 ) ) ;
#1511 = CARTESIAN_POINT ( 'NONE',  ( 33.51208342369033488, -9.877893692955346694, 40.06259746622173168 ) ) ;
#1512 = DIRECTION ( 'NONE',  ( 0.5503133621338236470, -0.8349582046168341209, -0.000000000000000000 ) ) ;
#1513 = VERTEX_POINT ( 'NONE', #16184 ) ;
#1514 = ORIENTED_EDGE ( 'NONE', *, *, #15762, .F. ) ;
#1515 = CARTESIAN_POINT ( 'NONE',  ( 4.510281037539698445E-13, -4.926614671774132148E-13, 65.49999999999998579 ) ) ;
#1516 = CARTESIAN_POINT ( 'NONE',  ( -32.74775157610409337, 27.21557300919391054, -19.50000000000000355 ) ) ;
#1517 = DIRECTION ( 'NONE',  ( 0.000000000000000000, -1.132880637372608986E-16, 1.000000000000000000 ) ) ;
#1518 = ORIENTED_EDGE ( 'NONE', *, *, #17633, .T. ) ;
#1519 = DIRECTION ( 'NONE',  ( -0.000000000000000000, 0.000000000000000000, 1.000000000000000000 ) ) ;
#1520 = CARTESIAN_POINT ( 'NONE',  ( 9.184330860358528525, -14.33603326865607741, 18.72771030977186868 ) ) ;
#1521 = EDGE_CURVE ( 'NONE', #28904, #8444, #426, .T. ) ;
#1522 = ORIENTED_EDGE ( 'NONE', *, *, #24101, .F. ) ;
#1523 = EDGE_LOOP ( 'NONE', ( #7018, #9466, #4233, #11567 ) ) ;
#1524 = EDGE_CURVE ( 'NONE', #8240, #3050, #30833, .T. ) ;
#1525 = CARTESIAN_POINT ( 'NONE',  ( -11.25351117620539121, -16.53363456493219985, 18.84056766331481825 ) ) ;
#1526 = CARTESIAN_POINT ( 'NONE',  ( -29.61203839202723032, -15.40012917324033381, 37.38016955275590192 ) ) ;
#1527 = CARTESIAN_POINT ( 'NONE',  ( 15.05691039802739084, 13.16451011206821242, 7.626647697317575414 ) ) ;
#1528 = CARTESIAN_POINT ( 'NONE',  ( -40.00000000000000000, 90.00000000000001421, 12.49999999999999112 ) ) ;
#1529 = EDGE_LOOP ( 'NONE', ( #9098, #1501, #3280, #21052, #26247, #3559 ) ) ;
#1530 = DIRECTION ( 'NONE',  ( -0.000000000000000000, 1.132880637372608986E-16, -1.000000000000000000 ) ) ;
#1531 = ORIENTED_EDGE ( 'NONE', *, *, #30532, .T. ) ;
#1532 = CARTESIAN_POINT ( 'NONE',  ( -14.93131746129344961, -8.256826158564470219, 5.759928666072747561 ) ) ;
#1533 = AXIS2_PLACEMENT_3D ( 'NONE', #5893, #583, #10420 ) ;
#1534 = CARTESIAN_POINT ( 'NONE',  ( -25.47847050916410439, -26.57182937991348481, 24.50000000000000000 ) ) ;
#1535 = EDGE_LOOP ( 'NONE', ( #14556, #8831 ) ) ;
#1536 = FACE_OUTER_BOUND ( 'NONE', #20558, .T. ) ;
#1537 = CARTESIAN_POINT ( 'NONE',  ( -11.21147646446735102, 30.29926891764210595, 1.500000000000000000 ) ) ;
#1538 = CARTESIAN_POINT ( 'NONE',  ( 0.01267125088587631523, -20.01782649599895691, 7.595116371587256054 ) ) ;
#1539 = CARTESIAN_POINT ( 'NONE',  ( -9.908187358984028137, -17.39367339311968053, 20.06253562465620632 ) ) ;
#1540 = CARTESIAN_POINT ( 'NONE',  ( -17.02473723647801052, 1.129071356443817065, 20.24143955528809258 ) ) ;
#1541 = CARTESIAN_POINT ( 'NONE',  ( -17.04940614979727798, 0.8516807413325224729, 18.73743063545763121 ) ) ;
#1542 = DIRECTION ( 'NONE',  ( -0.000000000000000000, -0.000000000000000000, -1.000000000000000000 ) ) ;
#1543 = ORIENTED_EDGE ( 'NONE', *, *, #27881, .T. ) ;
#1544 = DIRECTION ( 'NONE',  ( -0.000000000000000000, -0.000000000000000000, -1.000000000000000000 ) ) ;
#1545 = CARTESIAN_POINT ( 'NONE',  ( 17.94248964168179583, 34.33858135081683827, 34.80090346875809360 ) ) ;
#1546 = ORIENTED_EDGE ( 'NONE', *, *, #14387, .F. ) ;
#1547 = ORIENTED_EDGE ( 'NONE', *, *, #7279, .F. ) ;
#1548 = CARTESIAN_POINT ( 'NONE',  ( 47.38379984956800683, 69.82936349420988620, 15.74781942413362401 ) ) ;
#1549 = EDGE_CURVE ( 'NONE', #19074, #19937, #8411, .T. ) ;
#1550 = CARTESIAN_POINT ( 'NONE',  ( -15.34618562042307310, 12.82554431217321245, 5.652196082369965069 ) ) ;
#1551 = AXIS2_PLACEMENT_3D ( 'NONE', #27356, #5980, #30295 ) ;
#1552 = CARTESIAN_POINT ( 'NONE',  ( -5.103338407348687156, 19.35644909001343450, 6.211014596808754007 ) ) ;
#1553 = ORIENTED_EDGE ( 'NONE', *, *, #27298, .F. ) ;
#1554 = DIRECTION ( 'NONE',  ( 0.000000000000000000, 0.000000000000000000, -1.000000000000000000 ) ) ;
#1555 = CIRCLE ( 'NONE', #2046, 0.7499999999999997780 ) ;
#1556 = EDGE_CURVE ( 'NONE', #15672, #2241, #10408, .T. ) ;
#1557 = CARTESIAN_POINT ( 'NONE',  ( -13.29701885124480576, 10.65950381936556113, 5.651492010659111997 ) ) ;
#1558 = CARTESIAN_POINT ( 'NONE',  ( 23.13152334643393715, 11.98019263786950184, 48.95036236640387983 ) ) ;
#1559 = VERTEX_POINT ( 'NONE', #23806 ) ;
#1560 = EDGE_CURVE ( 'NONE', #2431, #1375, #11898, .T. ) ;
#1561 = DIRECTION ( 'NONE',  ( -0.000000000000000000, -0.000000000000000000, -1.000000000000000000 ) ) ;
#1562 = CARTESIAN_POINT ( 'NONE',  ( 2.094186647214742347, -9.248129367672074608, 1.500000000000001332 ) ) ;
#1563 = B_SPLINE_CURVE_WITH_KNOTS ( 'NONE', 3,
 ( #8926, #25745, #9067, #30722, #30123, #1889 ),
 .UNSPECIFIED., .F., .F.,
 ( 4, 2, 4 ),
 ( 0.01057608626842624147, 0.01589305904737019909, 0.02121003182631415324 ),
 .UNSPECIFIED. ) ;
#1564 = VERTEX_POINT ( 'NONE', #23356 ) ;
#1565 = DIRECTION ( 'NONE',  ( 1.000000000000000000, 0.000000000000000000, 0.000000000000000000 ) ) ;
#1566 = ORIENTED_EDGE ( 'NONE', *, *, #24828, .F. ) ;
#1567 = EDGE_CURVE ( 'NONE', #23779, #9215, #4782, .T. ) ;
#1568 = CARTESIAN_POINT ( 'NONE',  ( -25.47847050916410439, -26.57182937991348481, 26.54355021145562787 ) ) ;
#1569 = EDGE_LOOP ( 'NONE', ( #15158, #10530, #11871, #10690 ) ) ;
#1570 = EDGE_CURVE ( 'NONE', #14635, #28482, #19349, .T. ) ;
#1571 = ORIENTED_EDGE ( 'NONE', *, *, #2711, .T. ) ;
#1572 = EDGE_CURVE ( 'NONE', #27348, #886, #4923, .T. ) ;
#1573 = CARTESIAN_POINT ( 'NONE',  ( 3.215610563331066540, 16.76717343535964844, 7.196036389296800451 ) ) ;
#1574 = B_SPLINE_CURVE_WITH_KNOTS ( 'NONE', 3,
 ( #9873, #15005, #12688, #10176, #510 ),
 .UNSPECIFIED., .F., .F.,
 ( 4, 1, 4 ),
 ( 0.1429309129599393158, 0.1481973127024909243, 0.1534637124450425050 ),
 .UNSPECIFIED. ) ;
#1575 = CARTESIAN_POINT ( 'NONE',  ( 33.48319591361583036, 9.771272583783428445, 40.12028472023447279 ) ) ;
#1576 = CARTESIAN_POINT ( 'NONE',  ( 5.545588074468605022, 19.21617731956021302, 18.37250658438899009 ) ) ;
#1577 = ORIENTED_EDGE ( 'NONE', *, *, #1998, .F. ) ;
#1578 = VECTOR ( 'NONE', #3789, 1000.000000000000000 ) ;
#1579 = CARTESIAN_POINT ( 'NONE',  ( -23.69412710310941605, -29.84645176427128987, 34.80090346875804386 ) ) ;
#1580 = DIRECTION ( 'NONE',  ( 1.000000000000000000, 0.000000000000000000, 0.000000000000000000 ) ) ;
#1581 = CARTESIAN_POINT ( 'NONE',  ( 19.89498243266959676, 2.215034284604904702, 19.11611934778430921 ) ) ;
#1582 = ORIENTED_EDGE ( 'NONE', *, *, #3226, .T. ) ;
#1583 = CARTESIAN_POINT ( 'NONE',  ( -16.82187727961403922, 2.603938281378752162, 19.66989035740801839 ) ) ;
#1584 = DIRECTION ( 'NONE',  ( 0.000000000000000000, -1.132880637372608986E-16, 1.000000000000000000 ) ) ;
#1585 = CARTESIAN_POINT ( 'NONE',  ( -14.01239083805804597, 9.763392886517387126, 6.560937769032974209 ) ) ;
#1586 = CARTESIAN_POINT ( 'NONE',  ( 5.298969250677085796, 19.30368332842023094, 18.34798005862662507 ) ) ;
#1587 = ORIENTED_EDGE ( 'NONE', *, *, #7500, .T. ) ;
#1588 = ORIENTED_EDGE ( 'NONE', *, *, #27343, .F. ) ;
#1589 = CARTESIAN_POINT ( 'NONE',  ( 39.99999999999998579, 80.00000000000001421, 27.49999999999998934 ) ) ;
#1590 = EDGE_CURVE ( 'NONE', #21023, #20390, #27339, .T. ) ;
#1591 = LINE ( 'NONE', #6710, #11635 ) ;
#1592 = EDGE_CURVE ( 'NONE', #21977, #11816, #18995, .T. ) ;
#1593 = CARTESIAN_POINT ( 'NONE',  ( 8.884323311075775109, 1.438332125858202692, 21.50000000000000000 ) ) ;
#1594 = CARTESIAN_POINT ( 'NONE',  ( -5.023839636758346217, 19.37724795171757819, 19.11611934778430921 ) ) ;
#1595 = FACE_OUTER_BOUND ( 'NONE', #5843, .T. ) ;
#1596 = DIRECTION ( 'NONE',  ( -0.000000000000000000, 0.000000000000000000, 1.000000000000000000 ) ) ;
#1597 = EDGE_CURVE ( 'NONE', #6797, #18116, #28187, .T. ) ;
#1598 = LINE ( 'NONE', #25900, #7425 ) ;
#1599 = CARTESIAN_POINT ( 'NONE',  ( -5.846240454020377619, 19.12690956503888629, 7.652108011868849147 ) ) ;
#1600 = VERTEX_POINT ( 'NONE', #6818 ) ;
#1601 = EDGE_CURVE ( 'NONE', #9461, #16202, #8925, .T. ) ;
#1602 = AXIS2_PLACEMENT_3D ( 'NONE', #1378, #19360, #7512 ) ;
#1603 = CARTESIAN_POINT ( 'NONE',  ( -19.87001189204712759, 2.428856360474549447, 7.652108011868850035 ) ) ;
#1604 = CARTESIAN_POINT ( 'NONE',  ( -33.03011559203990544, 8.976883822286589876, 40.77182279851235336 ) ) ;
#1605 = CARTESIAN_POINT ( 'NONE',  ( 39.87350638640253919, -4.706224724400463799, -6.500000000000000888 ) ) ;
#1606 = EDGE_LOOP ( 'NONE', ( #29960, #14559, #1780, #5201 ) ) ;
#1607 = ORIENTED_EDGE ( 'NONE', *, *, #15669, .T. ) ;
#1608 = EDGE_CURVE ( 'NONE', #30496, #8380, #2142, .T. ) ;
#1609 = DIRECTION ( 'NONE',  ( -0.000000000000000000, -0.000000000000000000, -1.000000000000000000 ) ) ;
#1610 = CARTESIAN_POINT ( 'NONE',  ( -19.85983307072122628, 2.367331911061644423, 20.34789198813115618 ) ) ;
#1611 = EDGE_LOOP ( 'NONE', ( #27625, #4985, #27472, #29846 ) ) ;
#1612 = CARTESIAN_POINT ( 'NONE',  ( 0.2238118478526182897, -19.99918941848005360, 5.651480102388688032 ) ) ;
#1613 = CARTESIAN_POINT ( 'NONE',  ( -5.881244434206279514, -6.812559277181949646, 1.500000000000001332 ) ) ;
#1614 = AXIS2_PLACEMENT_3D ( 'NONE', #4560, #28279, #9547 ) ;
#1615 = CARTESIAN_POINT ( 'NONE',  ( -18.94750032487069902, -37.15750911010949409, 24.13564184353800712 ) ) ;
#1616 = CARTESIAN_POINT ( 'NONE',  ( 47.14142842854284510, 69.79466010243311302, 59.49999999999998579 ) ) ;
#1617 = LINE ( 'NONE', #20922, #5360 ) ;
#1618 = LINE ( 'NONE', #23264, #22771 ) ;
#1619 = CARTESIAN_POINT ( 'NONE',  ( 1.265447379378153769, -19.97763032565216079, 7.098451512883313441 ) ) ;
#1620 = CARTESIAN_POINT ( 'NONE',  ( -16.87879800889955106, 2.262652451732489745, 5.848946451764560628 ) ) ;
#1621 = ORIENTED_EDGE ( 'NONE', *, *, #4317, .F. ) ;
#1622 = EDGE_CURVE ( 'NONE', #10771, #1929, #26341, .T. ) ;
#1623 = EDGE_CURVE ( 'NONE', #26855, #21196, #9024, .T. ) ;
#1624 = AXIS2_PLACEMENT_3D ( 'NONE', #8813, #25347, #23302 ) ;
#1625 = DIRECTION ( 'NONE',  ( 1.000000000000000000, 0.000000000000000000, 0.000000000000000000 ) ) ;
#1626 = DIRECTION ( 'NONE',  ( -0.000000000000000000, -0.000000000000000000, 1.000000000000000000 ) ) ;
#1627 = DIRECTION ( 'NONE',  ( 0.000000000000000000, 0.000000000000000000, -1.000000000000000000 ) ) ;
#1628 = CARTESIAN_POINT ( 'NONE',  ( -38.00000000000000711, 65.00000000000000000, 50.49999999999998579 ) ) ;
#1629 = CARTESIAN_POINT ( 'NONE',  ( -19.64114023396061981, 37.13592150528867109, -1.500000000000000000 ) ) ;
#1630 = CARTESIAN_POINT ( 'NONE',  ( -22.94541271838176044, 35.03073867844246081, -6.500000000000000888 ) ) ;
#1631 = ORIENTED_EDGE ( 'NONE', *, *, #838, .F. ) ;
#1632 = DIRECTION ( 'NONE',  ( 1.000000000000000000, 0.000000000000000000, 0.000000000000000000 ) ) ;
#1633 = VECTOR ( 'NONE', #3197, 1000.000000000000000 ) ;
#1634 = CARTESIAN_POINT ( 'NONE',  ( 35.57581530336350539, -17.46952725568587894, 34.79368316662617389 ) ) ;
#1636 = VECTOR ( 'NONE', #26633, 1000.000000000000000 ) ;
#1635 = CARTESIAN_POINT ( 'NONE',  ( 0.000000000000000000, 0.000000000000000000, 21.50000000000000000 ) ) ;
#1637 = VERTEX_POINT ( 'NONE', #16344 ) ;
#1638 = EDGE_LOOP ( 'NONE', ( #27726, #29523, #9939 ) ) ;
#1639 = CARTESIAN_POINT ( 'NONE',  ( -5.374868878256215510, -44.10336124695545124, -19.50000000000000355 ) ) ;
#1640 = CARTESIAN_POINT ( 'NONE',  ( -8.478038329015333829, 15.04174200911163517, -0.6213203435596476032 ) ) ;
#1641 = ORIENTED_EDGE ( 'NONE', *, *, #15331, .F. ) ;
#1642 = DIRECTION ( 'NONE',  ( 1.000000000000000000, 0.000000000000000000, 0.000000000000000000 ) ) ;
#1643 = CARTESIAN_POINT ( 'NONE',  ( 19.63396244889326425, 3.810028285208275634, 18.54958172136248606 ) ) ;
#1644 = ORIENTED_EDGE ( 'NONE', *, *, #2360, .T. ) ;
#1645 = CARTESIAN_POINT ( 'NONE',  ( 17.75446986341059841, 9.207540381081344094, 24.50000000000000000 ) ) ;
#1646 = FACE_OUTER_BOUND ( 'NONE', #22033, .T. ) ;
#1647 = ORIENTED_EDGE ( 'NONE', *, *, #1560, .F. ) ;
#1648 = CARTESIAN_POINT ( 'NONE',  ( 11.80522207443771521, 12.33118449403810146, 19.96568007040469084 ) ) ;
#1649 = AXIS2_PLACEMENT_3D ( 'NONE', #27433, #3724, #22886 ) ;
#1650 = CARTESIAN_POINT ( 'NONE',  ( 16.65271093596605922, 3.715728438117816168, 5.759928666072751113 ) ) ;
#1651 = DIRECTION ( 'NONE',  ( -0.000000000000000000, -0.000000000000000000, -1.000000000000000000 ) ) ;
#1652 = AXIS2_PLACEMENT_3D ( 'NONE', #29084, #17072, #7725 ) ;
#1653 = CARTESIAN_POINT ( 'NONE',  ( -47.82582523423074861, 69.88269270952190482, 16.26542374043941308 ) ) ;
#1654 = CARTESIAN_POINT ( 'NONE',  ( 24.73258466867350336, -33.64422401625958514, -6.500000000000000888 ) ) ;
#1655 = CARTESIAN_POINT ( 'NONE',  ( 35.78163722268750746, 27.43648963448195133, -11.49999999999999645 ) ) ;
#1656 = CARTESIAN_POINT ( 'NONE',  ( 0.000000000000000000, 0.000000000000000000, 1.500000000000001332 ) ) ;
#1657 = CARTESIAN_POINT ( 'NONE',  ( -8.840471615930058036, 1.687027447297517080, -3.621320343559650379 ) ) ;
#1658 = PLANE ( 'NONE',  #446 ) ;
#1659 = CARTESIAN_POINT ( 'NONE',  ( -8.774062813931127636, -14.60569725955141962, 20.32222155561919053 ) ) ;
#1660 =( REPRESENTATION_RELATIONSHIP ('NONE','NONE', #19885, #7129 ) REPRESENTATION_RELATIONSHIP_WITH_TRANSFORMATION ( #14438 )SHAPE_REPRESENTATION_RELATIONSHIP( ) );
#1661 = VERTEX_POINT ( 'NONE', #25551 ) ;
#1662 = VERTEX_POINT ( 'NONE', #4176 ) ;
#1663 = DIRECTION ( 'NONE',  ( -1.000000000000000000, 0.000000000000000000, 0.000000000000000000 ) ) ;
#1664 = FACE_OUTER_BOUND ( 'NONE', #28593, .T. ) ;
#1665 = VERTEX_POINT ( 'NONE', #25860 ) ;
#1666 = CARTESIAN_POINT ( 'NONE',  ( -6.028330626922774549, 10.93629592680536788, 1.500000000000001332 ) ) ;
#1667 = CARTESIAN_POINT ( 'NONE',  ( 24.03057240117691862, 26.57182937991349903, -6.500000000000000888 ) ) ;
#1668 = EDGE_LOOP ( 'NONE', ( #30066, #14694, #18967, #7612 ) ) ;
#1669 = CIRCLE ( 'NONE', #19099, 37.50000000000001421 ) ;
#1670 = DIRECTION ( 'NONE',  ( 0.000000000000000000, 0.000000000000000000, 1.000000000000000000 ) ) ;
#1671 = B_SPLINE_CURVE_WITH_KNOTS ( 'NONE', 3,
 ( #9802, #19468, #7618, #11837, #2626, #7157, #23979, #21647, #19014, #19160, #17281, #14316, #21487, #9496, #28526, #21806, #28983, #17123, #28679, #24301 ),
 .UNSPECIFIED., .F., .F.,
 ( 4, 2, 2, 2, 2, 2, 2, 2, 2, 4 ),
 ( 0.000000000000000000, 0.06250000000000160982, 0.1250000000000035527, 0.1875000000000054956, 0.2187500000000055789, 0.2500000000000056621, 0.3125000000000041633, 0.3750000000000026645, 0.4375000000000011657, 0.5000000000000000000 ),
 .UNSPECIFIED. ) ;
#1672 = CARTESIAN_POINT ( 'NONE',  ( -10.71492722147446308, -16.90904491356049633, 18.36582235739946611 ) ) ;
#1673 = DIRECTION ( 'NONE',  ( 0.000000000000000000, -1.132880637372608986E-16, 1.000000000000000000 ) ) ;
#1674 = EDGE_LOOP ( 'NONE', ( #10641, #9379, #25960, #27802 ) ) ;
#1675 = FACE_OUTER_BOUND ( 'NONE', #11524, .T. ) ;
#1676 = ORIENTED_EDGE ( 'NONE', *, *, #17163, .T. ) ;
#1677 = DIRECTION ( 'NONE',  ( 0.000000000000000000, 0.000000000000000000, 1.000000000000000000 ) ) ;
#1678 = ORIENTED_EDGE ( 'NONE', *, *, #16623, .T. ) ;
#1679 = DIRECTION ( 'NONE',  ( -0.000000000000000000, -0.000000000000000000, 1.000000000000000000 ) ) ;
#1680 = CARTESIAN_POINT ( 'NONE',  ( 31.34809375791739683, -25.29209928965034848, 30.54052050932160256 ) ) ;
#1681 = DIRECTION ( 'NONE',  ( -0.000000000000000000, -0.000000000000000000, -1.000000000000000000 ) ) ;
#1682 = CARTESIAN_POINT ( 'NONE',  ( 17.79239818699415920, 14.89473990422378158, 1.500000000000000000 ) ) ;
#1683 = CYLINDRICAL_SURFACE ( 'NONE', #566, 4.999999999999997335 ) ;
#1684 = VECTOR ( 'NONE', #5109, 1000.000000000000000 ) ;
#1685 = CARTESIAN_POINT ( 'NONE',  ( -17.05973338880502155, 0.7261025713186424202, 18.92976555901915603 ) ) ;
#1686 = FACE_BOUND ( 'NONE', #30371, .T. ) ;
#1687 = ORIENTED_EDGE ( 'NONE', *, *, #3333, .T. ) ;
#1688 = VECTOR ( 'NONE', #24091, 1000.000000000000000 ) ;
#1689 = B_SPLINE_CURVE_WITH_KNOTS ( 'NONE', 3,
 ( #23857, #12017, #9671, #7339, #16849, #26363, #7964, #9827, #14963, #470, #29322, #7642, #22287, #26515, #21981, #29006, #10129, #19634 ),
 .UNSPECIFIED., .F., .F.,
 ( 4, 2, 2, 2, 2, 2, 2, 2, 4 ),
 ( 0.000000000000000000, 0.0003967869494442956908, 0.0007935738988885913817, 0.001190360848332887127, 0.001587147797777182763, 0.001983934747221478400, 0.002380721696665774254, 0.002777508646110069673, 0.003174295595554365527 ),
 .UNSPECIFIED. ) ;
#1690 = CARTESIAN_POINT ( 'NONE',  ( -28.54661976619838981, 28.95749706969278847, 15.30506458469658071 ) ) ;
#1691 = DIRECTION ( 'NONE',  ( 0.9594929736144952592, -0.2817325568414371095, 0.000000000000000000 ) ) ;
#1692 = VERTEX_POINT ( 'NONE', #13704 ) ;
#1693 = ORIENTED_EDGE ( 'NONE', *, *, #24644, .F. ) ;
#1694 = CARTESIAN_POINT ( 'NONE',  ( -2.431858781452794993, -8.752572334588114344, 21.50000000000000000 ) ) ;
#1695 = CARTESIAN_POINT ( 'NONE',  ( -4.940218127011007709, 16.29708528951389113, 5.862424720655265098 ) ) ;
#1696 = ORIENTED_EDGE ( 'NONE', *, *, #28797, .T. ) ;
#1697 = DIRECTION ( 'NONE',  ( -0.000000000000000000, -0.000000000000000000, -1.000000000000000000 ) ) ;
#1698 = CARTESIAN_POINT ( 'NONE',  ( -30.33183837007556249, -13.53414739637282516, -16.55003854064094426 ) ) ;
#1699 = DIRECTION ( 'NONE',  ( 1.000000000000000000, 0.000000000000000000, -0.000000000000000000 ) ) ;
#1700 = ORIENTED_EDGE ( 'NONE', *, *, #22914, .F. ) ;
#1701 = DIRECTION ( 'NONE',  ( -1.000000000000000000, 0.000000000000000000, 0.000000000000000000 ) ) ;
#1702 = LINE ( 'NONE', #20570, #17967 ) ;
#1703 = ORIENTED_EDGE ( 'NONE', *, *, #13989, .F. ) ;
#1704 = CARTESIAN_POINT ( 'NONE',  ( -23.07950435457407679, 11.50806656539752737, -16.55003854064094426 ) ) ;
#1705 = CIRCLE ( 'NONE', #23109, 3.000000000000002665 ) ;
#1706 = ORIENTED_EDGE ( 'NONE', *, *, #15656, .T. ) ;
#1707 = CARTESIAN_POINT ( 'NONE',  ( -4.163336342344337027E-14, -1.387778780781445676E-14, -1.500000000000000000 ) ) ;
#1708 = ORIENTED_EDGE ( 'NONE', *, *, #23072, .F. ) ;
#1709 = ORIENTED_EDGE ( 'NONE', *, *, #11204, .T. ) ;
#1710 = EDGE_CURVE ( 'NONE', #17660, #12655, #26844, .T. ) ;
#1711 = CARTESIAN_POINT ( 'NONE',  ( -15.57772019539775776, -6.859948791675931190, 6.755862304746362845 ) ) ;
#1712 = PRODUCT_RELATED_PRODUCT_CATEGORY ( 'part', '', ( #23591 ) ) ;
#1713 = DIRECTION ( 'NONE',  ( -1.000000000000000000, 0.000000000000000000, 0.000000000000000000 ) ) ;
#1714 = CARTESIAN_POINT ( 'NONE',  ( -64.99999999999998579, -36.86186943028246787, 97.07879600563551037 ) ) ;
#1715 = VERTEX_POINT ( 'NONE', #4492 ) ;
#1716 = CARTESIAN_POINT ( 'NONE',  ( -35.76481447503398670, -5.202797454133643917, 27.50000000000000355 ) ) ;
#1717 = CARTESIAN_POINT ( 'NONE',  ( 1.438332125858173605, -8.884323311075778662, -3.621320343559650379 ) ) ;
#1718 = FACE_OUTER_BOUND ( 'NONE', #25812, .T. ) ;
#1719 = ORIENTED_EDGE ( 'NONE', *, *, #13952, .T. ) ;
#1720 = ADVANCED_FACE ( 'NONE', ( #21149 ), #30669, .F. ) ;
#1721 = CARTESIAN_POINT ( 'NONE',  ( -16.96496223448354712, 1.652369715233090286, 20.34789198813115263 ) ) ;
#1722 = CARTESIAN_POINT ( 'NONE',  ( 15.39622458953738082, -7.259188434806188361, 6.864725433338323413 ) ) ;
#1723 = DIRECTION ( 'NONE',  ( -0.000000000000000000, -0.000000000000000000, 1.000000000000000000 ) ) ;
#1724 = CARTESIAN_POINT ( 'NONE',  ( 4.316117848019421999, 19.54676362458759087, 19.36813350477385143 ) ) ;
#1725 = VERTEX_POINT ( 'NONE', #12127 ) ;
#1726 = EDGE_LOOP ( 'NONE', ( #5104, #22705, #1867, #28955 ) ) ;
#1727 = CIRCLE ( 'NONE', #29633, 23.20393738267273420 ) ;
#1728 = CARTESIAN_POINT ( 'NONE',  ( -37.99999999999999289, 209.2686044187655909, -75.50000000000000000 ) ) ;
#1729 = CARTESIAN_POINT ( 'NONE',  ( 39.99999999999998579, 90.00000000000001421, 59.49999999999999289 ) ) ;
#1730 = CARTESIAN_POINT ( 'NONE',  ( -4.673829994069182980, 16.36915245889225545, 18.90679857307105749 ) ) ;
#1731 = DIRECTION ( 'NONE',  ( 1.000000000000000000, 0.000000000000000000, 0.000000000000000000 ) ) ;
#1732 = CARTESIAN_POINT ( 'NONE',  ( 11.80353037517518366, 12.33292095755542483, 6.037360021877313798 ) ) ;
#1733 = ADVANCED_FACE ( 'NONE', ( #5565 ), #29631, .F. ) ;
#1734 = CARTESIAN_POINT ( 'NONE',  ( 26.11179934312167816, -14.04991663536889135, 41.10667063058289727 ) ) ;
#1735 = EDGE_CURVE ( 'NONE', #4121, #4711, #16798, .T. ) ;
#1736 = LINE ( 'NONE', #23090, #25376 ) ;
#1737 = ORIENTED_EDGE ( 'NONE', *, *, #20599, .T. ) ;
#1738 = CARTESIAN_POINT ( 'NONE',  ( 0.6218383925729503714, -19.99069893758407446, 5.679672709359372185 ) ) ;
#1739 = CARTESIAN_POINT ( 'NONE',  ( 14.79007711409980175, 13.46370387462956586, 18.34869673959212122 ) ) ;
#1740 = CARTESIAN_POINT ( 'NONE',  ( -4.163336342344337027E-14, 1.387778780781445676E-14, -1.500000000000000000 ) ) ;
#1741 = VERTEX_POINT ( 'NONE', #5257 ) ;
#1742 = CYLINDRICAL_SURFACE ( 'NONE', #11330, 0.7500000000000007772 ) ;
#1743 = ORIENTED_EDGE ( 'NONE', *, *, #12996, .F. ) ;
#1744 = FACE_OUTER_BOUND ( 'NONE', #18324, .T. ) ;
#1745 = UNCERTAINTY_MEASURE_WITH_UNIT (LENGTH_MEASURE( 1.000000000000000082E-05 ), #891, 'distance_accuracy_value', 'NONE');
#1746 = DIRECTION ( 'NONE',  ( 1.000000000000000000, 0.000000000000000000, 0.000000000000000000 ) ) ;
#1747 = ORIENTED_EDGE ( 'NONE', *, *, #14163, .F. ) ;
#1748 = CARTESIAN_POINT ( 'NONE',  ( 0.000000000000000000, 0.000000000000000000, 21.50000000000000000 ) ) ;
#1749 = VECTOR ( 'NONE', #19643, 1000.000000000000000 ) ;
#1750 = ADVANCED_FACE ( 'NONE', ( #21628, #14614 ), #24117, .T. ) ;
#1751 = CARTESIAN_POINT ( 'NONE',  ( 11.90408231459837296, 48.56330485012143328, -64.13958309445501982 ) ) ;
#1752 = EDGE_CURVE ( 'NONE', #8742, #20574, #14920, .T. ) ;
#1753 = DIRECTION ( 'NONE',  ( 1.000000000000000000, 0.000000000000000000, 0.000000000000000000 ) ) ;
#1754 = CARTESIAN_POINT ( 'NONE',  ( -25.64627119138473432, -23.40052582045089480, -16.50000600000000262 ) ) ;
#1755 = CARTESIAN_POINT ( 'NONE',  ( -50.00000000000000000, 70.00000000000000000, -92.50000000000000000 ) ) ;
#1756 = ADVANCED_FACE ( 'NONE', ( #10234 ), #12279, .F. ) ;
#1757 = CARTESIAN_POINT ( 'NONE',  ( 24.03057240117690441, -26.57182937991349903, 26.54355021145563143 ) ) ;
#1758 = CARTESIAN_POINT ( 'NONE',  ( 1.411528516173250924, -17.00651183856732374, 7.441806358946449151 ) ) ;
#1759 = CARTESIAN_POINT ( 'NONE',  ( -27.75715622479468081, 2.303929616531696922E-16, 24.50000000000000000 ) ) ;
#1760 = VERTEX_POINT ( 'NONE', #7755 ) ;
#1761 = ADVANCED_FACE ( 'NONE', ( #19447 ), #14758, .F. ) ;
#1762 = ADVANCED_FACE ( 'NONE', ( #9938, #26790 ), #19141, .T. ) ;
#1763 = CARTESIAN_POINT ( 'NONE',  ( 0.000000000000000000, 44.39187623478217404, -19.50000000000000355 ) ) ;
#1764 = CARTESIAN_POINT ( 'NONE',  ( 32.19782014694307293, 14.25394737442116444, -16.55003854064094426 ) ) ;
#1765 = ORIENTED_EDGE ( 'NONE', *, *, #23091, .F. ) ;
#1766 = ADVANCED_FACE ( 'NONE', ( #12444 ), #3221, .F. ) ;
#1767 = DIRECTION ( 'NONE',  ( -0.000000000000000000, -0.000000000000000000, -1.000000000000000000 ) ) ;
#1768 = CARTESIAN_POINT ( 'NONE',  ( -14.83655028254229258, -8.438271213925730763, 18.64703902303423178 ) ) ;
#1769 = ADVANCED_FACE ( 'NONE', ( #26470 ), #29276, .F. ) ;
#1770 = CARTESIAN_POINT ( 'NONE',  ( 6.900000000000000355, 0.000000000000000000, 0.000000000000000000 ) ) ;
#1771 = ORIENTED_EDGE ( 'NONE', *, *, #28051, .F. ) ;
#1772 = DIRECTION ( 'NONE',  ( 1.000000000000000000, 0.000000000000000000, 0.000000000000000000 ) ) ;
#1773 = AXIS2_PLACEMENT_3D ( 'NONE', #23243, #11876, #18449 ) ;
#1774 = CARTESIAN_POINT ( 'NONE',  ( -12.72536390617885260, -2.839914339433650348, 1.500000000000001332 ) ) ;
#1775 = CARTESIAN_POINT ( 'NONE',  ( 36.88240865182195449, -7.258209409195951700, 37.49999999993649880 ) ) ;
#1777 = DIRECTION ( 'NONE',  ( 0.000000000000000000, 0.000000000000000000, -1.000000000000000000 ) ) ;
#1776 = B_SPLINE_CURVE_WITH_KNOTS ( 'NONE', 3,
 ( #25057, #10873, #5721, #3702, #19928, #29442 ),
 .UNSPECIFIED., .F., .F.,
 ( 4, 2, 4 ),
 ( 2.380730968220726544E-07, 0.002629065763328351790, 0.005257893453559881955 ),
 .UNSPECIFIED. ) ;
#1778 = ORIENTED_EDGE ( 'NONE', *, *, #6616, .T. ) ;
#1779 = CARTESIAN_POINT ( 'NONE',  ( 7.500000000000000000, 5.196152422706634688, -9.000000000000001776 ) ) ;
#1780 = ORIENTED_EDGE ( 'NONE', *, *, #4048, .T. ) ;
#1781 = CARTESIAN_POINT ( 'NONE',  ( -2.687479363073305372, 44.39187623477332068, -19.50000000000000355 ) ) ;
#1782 = DIRECTION ( 'NONE',  ( -0.000000000000000000, -0.000000000000000000, -1.000000000000000000 ) ) ;
#1783 = EDGE_CURVE ( 'NONE', #27228, #19294, #6425, .T. ) ;
#1784 = VERTEX_POINT ( 'NONE', #4948 ) ;
#1785 = AXIS2_PLACEMENT_3D ( 'NONE', #22998, #27857, #27696 ) ;
#1786 = CARTESIAN_POINT ( 'NONE',  ( -6.388525611213331068, -41.95271539343359990, 34.59875978651353989 ) ) ;
#1787 = ORIENTED_EDGE ( 'NONE', *, *, #18332, .T. ) ;
#1788 = CARTESIAN_POINT ( 'NONE',  ( 17.84153987719590972, -14.83584055149750114, 1.500000000000000000 ) ) ;
#1789 = ADVANCED_FACE ( 'NONE', ( #7449 ), #14460, .T. ) ;
#1790 = EDGE_CURVE ( 'NONE', #20003, #11001, #16858, .T. ) ;
#1791 = DIRECTION ( 'NONE',  ( 1.000000000000000000, 0.000000000000000000, 0.000000000000000000 ) ) ;
#1792 = DIRECTION ( 'NONE',  ( 1.000000000000000000, 0.000000000000000000, 0.000000000000000000 ) ) ;
#1793 = ORIENTED_EDGE ( 'NONE', *, *, #14566, .T. ) ;
#1794 = EDGE_CURVE ( 'NONE', #13443, #12232, #13404, .T. ) ;
#1795 = CARTESIAN_POINT ( 'NONE',  ( 23.07601128794333434, 11.40611796340042261, 45.01673140500131609 ) ) ;
#1796 = AXIS2_PLACEMENT_3D ( 'NONE', #16884, #14215, #26081 ) ;
#1797 = CARTESIAN_POINT ( 'NONE',  ( 16.56110944985980282, 4.167213836802830862, 6.917457548096560771 ) ) ;
#1798 = EDGE_CURVE ( 'NONE', #23467, #17274, #12906, .T. ) ;
#1799 = FACE_OUTER_BOUND ( 'NONE', #1077, .T. ) ;
#1800 = CARTESIAN_POINT ( 'NONE',  ( 3.637110358602582583, 19.99473753024312117, 1.500000000000000000 ) ) ;
#1801 = AXIS2_PLACEMENT_3D ( 'NONE', #26371, #16999, #2977 ) ;
#1802 = CARTESIAN_POINT ( 'NONE',  ( 24.35970437652574816, -13.37404834226503958, 47.21042702067961727 ) ) ;
#1803 = CYLINDRICAL_SURFACE ( 'NONE', #7872, 9.482273699623480212 ) ;
#1804 = DIRECTION ( 'NONE',  ( 0.000000000000000000, 0.000000000000000000, 1.000000000000000000 ) ) ;
#1805 = CARTESIAN_POINT ( 'NONE',  ( 3.264443110924797331, 16.75603743217150310, 19.96568007040468373 ) ) ;
#1806 = DIRECTION ( 'NONE',  ( 1.000000000000000000, 0.000000000000000000, 0.000000000000000000 ) ) ;
#1807 = LINE ( 'NONE', #8829, #5442 ) ;
#1808 = DIRECTION ( 'NONE',  ( -0.000000000000000000, 1.132880637372608986E-16, -1.000000000000000000 ) ) ;
#1809 = AXIS2_PLACEMENT_3D ( 'NONE', #13199, #12740, #10549 ) ;
#1810 = ORIENTED_EDGE ( 'NONE', *, *, #27747, .F. ) ;
#1811 = ORIENTED_EDGE ( 'NONE', *, *, #210, .F. ) ;
#1812 = CARTESIAN_POINT ( 'NONE',  ( 33.67904611717059993, 24.24635140542181233, -14.83330431306680453 ) ) ;
#1813 = AXIS2_PLACEMENT_3D ( 'NONE', #19674, #10322, #8151 ) ;
#1814 = CARTESIAN_POINT ( 'NONE',  ( -7.717362503659074058, -15.23305454438620110, 6.329955581934034292 ) ) ;
#1815 = CARTESIAN_POINT ( 'NONE',  ( 53.00000000000045475, -4.861708391419322267E-13, 65.49999999999998579 ) ) ;
#1816 = AXIS2_PLACEMENT_3D ( 'NONE', #15642, #22653, #25154 ) ;
#1817 = ORIENTED_EDGE ( 'NONE', *, *, #27673, .T. ) ;
#1818 = CARTESIAN_POINT ( 'NONE',  ( 0.000000000000000000, 0.000000000000000000, 0.000000000000000000 ) ) ;
#1819 = CARTESIAN_POINT ( 'NONE',  ( 15.38930515692758405, -7.273136567754734827, 19.22654678686458141 ) ) ;
#1820 = CARTESIAN_POINT ( 'NONE',  ( 9.181265711014134467, -14.33790826712539079, 19.96344307082652492 ) ) ;
#1821 = CIRCLE ( 'NONE', #9786, 0.7441270634457337607 ) ;
#1822 = ADVANCED_FACE ( 'NONE', ( #6024 ), #8376, .F. ) ;
#1823 = ORIENTED_EDGE ( 'NONE', *, *, #26337, .F. ) ;
#1824 = CARTESIAN_POINT ( 'NONE',  ( -19.83214989528428163, 2.722369515932092643, 5.670038381137163519 ) ) ;
#1825 = EDGE_CURVE ( 'NONE', #30853, #15826, #19864, .T. ) ;
#1826 = CIRCLE ( 'NONE', #1312, 0.7499999999999997780 ) ;
#1827 = VERTEX_POINT ( 'NONE', #20372 ) ;
#1828 = CARTESIAN_POINT ( 'NONE',  ( 29.61203839202725518, -15.40012917324033381, 41.62281023987508632 ) ) ;
#1829 = ORIENTED_EDGE ( 'NONE', *, *, #16466, .T. ) ;
#1830 = CARTESIAN_POINT ( 'NONE',  ( 0.000000000000000000, 1.699320956058915452E-16, -1.500000000000001776 ) ) ;
#1831 = CARTESIAN_POINT ( 'NONE',  ( 11.21147646446735102, 30.29926891764210595, -1.500000000000000000 ) ) ;
#1832 = AXIS2_PLACEMENT_3D ( 'NONE', #30006, #11583, #28276 ) ;
#1833 = ORIENTED_EDGE ( 'NONE', *, *, #13418, .F. ) ;
#1834 = AXIS2_PLACEMENT_3D ( 'NONE', #801, #3775, #24978 ) ;
#1835 = CARTESIAN_POINT ( 'NONE',  ( 19.74328841314636307, 3.194145055459935101, 7.652108011868850035 ) ) ;
#1836 =( NAMED_UNIT ( * ) PLANE_ANGLE_UNIT ( ) SI_UNIT ( $, .RADIAN. ) );
#1837 = DIRECTION ( 'NONE',  ( -0.000000000000000000, 1.000000000000000000, -0.000000000000000000 ) ) ;
#1838 = CARTESIAN_POINT ( 'NONE',  ( 39.99999999999998579, 80.00000000000001421, 17.49999999999999645 ) ) ;
#1839 = CIRCLE ( 'NONE', #27764, 37.50000000000001421 ) ;
#1840 = CYLINDRICAL_SURFACE ( 'NONE', #3816, 12.50000000000000000 ) ;
#1841 = AXIS2_PLACEMENT_3D ( 'NONE', #15376, #12910, #15536 ) ;
#1842 = CARTESIAN_POINT ( 'NONE',  ( -7.028330626922778990, 10.93629592680536788, 1.500000000000001332 ) ) ;
#1843 = DIRECTION ( 'NONE',  ( 1.000000000000000000, 0.000000000000000000, 0.000000000000000000 ) ) ;
#1844 = DIRECTION ( 'NONE',  ( 0.000000000000000000, 0.000000000000000000, 1.000000000000000000 ) ) ;
#1845 = VERTEX_POINT ( 'NONE', #18039 ) ;
#1846 = AXIS2_PLACEMENT_3D ( 'NONE', #16145, #6484, #1954 ) ;
#1847 = CIRCLE ( 'NONE', #17271, 27.70876437800068359 ) ;
#1848 = CARTESIAN_POINT ( 'NONE',  ( 17.94248964168179583, -34.33858135081684537, 34.80090346875808649 ) ) ;
#1849 = ORIENTED_EDGE ( 'NONE', *, *, #22349, .F. ) ;
#1850 = ORIENTED_EDGE ( 'NONE', *, *, #14891, .F. ) ;
#1851 = CARTESIAN_POINT ( 'NONE',  ( -25.10445388623454477, 25.60065097860747585, -1.500000000000000000 ) ) ;
#1852 = CARTESIAN_POINT ( 'NONE',  ( -7.856594496258223259, -4.390207617113929039, 21.50000000000000000 ) ) ;
#1853 = VERTEX_POINT ( 'NONE', #25363 ) ;
#1854 = CARTESIAN_POINT ( 'NONE',  ( -23.20393738267338790, 0.000000000000000000, 1.500000000000000000 ) ) ;
#1855 = CARTESIAN_POINT ( 'NONE',  ( 15.75094665830062723, -12.32508334119354032, 24.50000000000000000 ) ) ;
#1856 = ORIENTED_EDGE ( 'NONE', *, *, #17785, .F. ) ;
#1857 = DIRECTION ( 'NONE',  ( -0.000000000000000000, 1.000000000000000000, 0.000000000000000000 ) ) ;
#1858 = VECTOR ( 'NONE', #158, 1000.000000000000000 ) ;
#1859 = EDGE_CURVE ( 'NONE', #11064, #12314, #939, .T. ) ;
#1860 = CARTESIAN_POINT ( 'NONE',  ( 0.000000000000000000, 1.699320956058915452E-16, -1.500000000000001776 ) ) ;
#1861 = ORIENTED_EDGE ( 'NONE', *, *, #16788, .T. ) ;
#1862 = VECTOR ( 'NONE', #12585, 1000.000000000000000 ) ;
#1863 = VERTEX_POINT ( 'NONE', #23003 ) ;
#1864 = CARTESIAN_POINT ( 'NONE',  ( -24.73258466867759608, 33.64422401626517001, -6.500000000000000888 ) ) ;
#1865 = AXIS2_PLACEMENT_3D ( 'NONE', #30712, #18883, #7020 ) ;
#1866 = ORIENTED_EDGE ( 'NONE', *, *, #5959, .F. ) ;
#1867 = ORIENTED_EDGE ( 'NONE', *, *, #2489, .T. ) ;
#1868 = AXIS2_PLACEMENT_3D ( 'NONE', #21433, #375, #22045 ) ;
#1869 = LINE ( 'NONE', #6846, #8646 ) ;
#1870 = CARTESIAN_POINT ( 'NONE',  ( 0.8038475772933806329, -10.39230484541329247, 6.144194323733775069E-17 ) ) ;
#1871 = AXIS2_PLACEMENT_3D ( 'NONE', #12190, #16553, #28887 ) ;
#1872 = AXIS2_PLACEMENT_3D ( 'NONE', #24898, #18348, #27700 ) ;
#1873 = CARTESIAN_POINT ( 'NONE',  ( -11.52197458429825261, -37.50933785548060229, 27.49999999999999645 ) ) ;
#1874 = CARTESIAN_POINT ( 'NONE',  ( 11.11866449908641208, -16.64592002940951687, 18.34798005862930736 ) ) ;
#1875 = CARTESIAN_POINT ( 'NONE',  ( 19.76052160831509852, 3.198927888535952668, 18.34798005862930736 ) ) ;
#1876 = ORIENTED_EDGE ( 'NONE', *, *, #23476, .F. ) ;
#1877 = CARTESIAN_POINT ( 'NONE',  ( -19.70840172719294969, 3.506524300503917502, 19.33715507985239412 ) ) ;
#1878 = CARTESIAN_POINT ( 'NONE',  ( 15.67696945782692453, -6.669264855739881703, 5.701226463332907279 ) ) ;
#1879 = CIRCLE ( 'NONE', #15838, 1.447898107987198646 ) ;
#1880 = CARTESIAN_POINT ( 'NONE',  ( -14.00200865723716781, 9.777219707070196719, 6.447548852708279377 ) ) ;
#1881 = CARTESIAN_POINT ( 'NONE',  ( 3.338654329031695678, 16.73860904129763938, 18.64703902303423178 ) ) ;
#1882 = VERTEX_POINT ( 'NONE', #22858 ) ;
#1883 = ORIENTED_EDGE ( 'NONE', *, *, #17006, .T. ) ;
#1884 = VECTOR ( 'NONE', #29889, 1000.000000000000000 ) ;
#1885 = DIRECTION ( 'NONE',  ( -0.000000000000000000, -1.000000000000000000, -0.000000000000000000 ) ) ;
#1886 = CARTESIAN_POINT ( 'NONE',  ( 10.52561254559630655, -13.43997246249538513, 7.269896094239229001 ) ) ;
#1887 = CARTESIAN_POINT ( 'NONE',  ( 12.93287820108835007, 11.07039438038045454, 7.156916968540299351 ) ) ;
#1888 = CARTESIAN_POINT ( 'NONE',  ( 0.000000000000000000, 42.50000000000000000, 37.50000000000000000 ) ) ;
#1889 = CARTESIAN_POINT ( 'NONE',  ( 34.70577939417254498, 10.49309206032065944, 34.49999999999999289 ) ) ;
#1890 = CARTESIAN_POINT ( 'NONE',  ( 24.35970437652574816, -13.37404834226503958, 47.21042702067961727 ) ) ;
#1891 = ORIENTED_EDGE ( 'NONE', *, *, #29175, .F. ) ;
#1892 = AXIS2_PLACEMENT_3D ( 'NONE', #14281, #24110, #26306 ) ;
#1893 = CARTESIAN_POINT ( 'NONE',  ( -17.06158983937615403, 0.7019473037495110868, 6.995624166085161910 ) ) ;
#1894 = CARTESIAN_POINT ( 'NONE',  ( 14.18379620663259644, 14.10035196125401846, 19.48477075383298285 ) ) ;
#1895 = CARTESIAN_POINT ( 'NONE',  ( 19.64177907938615064, 36.71644397333972876, 24.50000000000000000 ) ) ;
#1896 = EDGE_LOOP ( 'NONE', ( #27103, #9157, #6706, #24049 ) ) ;
#1897 = CARTESIAN_POINT ( 'NONE',  ( 35.00000000000000000, 70.00000000000000000, 12.49999999999999112 ) ) ;
#1898 = ORIENTED_EDGE ( 'NONE', *, *, #24612, .T. ) ;
#1899 = CARTESIAN_POINT ( 'NONE',  ( 15.90320373664001075, -6.152843468454366693, 5.678370764302467677 ) ) ;
#1900 = ADVANCED_FACE ( 'NONE', ( #10701 ), #18192, .F. ) ;
#1901 = AXIS2_PLACEMENT_3D ( 'NONE', #16865, #26382, #29171 ) ;
#1902 = CARTESIAN_POINT ( 'NONE',  ( -20.29038667444665833, 38.16990472509154841, -16.50000000000000000 ) ) ;
#1903 = VERTEX_POINT ( 'NONE', #27087 ) ;
#1904 = DIRECTION ( 'NONE',  ( -1.000000000000000000, 0.000000000000000000, 0.000000000000000000 ) ) ;
#1905 = LINE ( 'NONE', #18458, #3825 ) ;
#1906 = FACE_OUTER_BOUND ( 'NONE', #6700, .T. ) ;
#1907 = CARTESIAN_POINT ( 'NONE',  ( -24.98398214727285804, -23.12412086524405908, -16.50001200000000523 ) ) ;
#1908 = CARTESIAN_POINT ( 'NONE',  ( -25.64627119138473788, 23.40052582045089480, -16.50000000000000000 ) ) ;
#1909 = EDGE_CURVE ( 'NONE', #26525, #23603, #11392, .T. ) ;
#1910 = DIRECTION ( 'NONE',  ( 1.000000000000000000, 0.000000000000000000, 0.000000000000000000 ) ) ;
#1911 = CARTESIAN_POINT ( 'NONE',  ( -25.48568755041063838, 12.36160011285429583, 24.50000000000000000 ) ) ;
#1912 = ORIENTED_EDGE ( 'NONE', *, *, #28902, .T. ) ;
#1913 = CIRCLE ( 'NONE', #915, 20.00000000000000000 ) ;
#1914 = CARTESIAN_POINT ( 'NONE',  ( -28.79137815760242702, -9.331429872129930914, 1.500000000000000000 ) ) ;
#1915 = FACE_OUTER_BOUND ( 'NONE', #241, .T. ) ;
#1916 = ORIENTED_EDGE ( 'NONE', *, *, #18398, .F. ) ;
#1917 = CARTESIAN_POINT ( 'NONE',  ( -25.10445388623454477, -25.60065097860747585, 1.500000000000000000 ) ) ;
#1918 = CARTESIAN_POINT ( 'NONE',  ( -17.62281152098609738, -9.494300025206934279, 19.03762469184452755 ) ) ;
#1919 = DIRECTION ( 'NONE',  ( 0.000000000000000000, 0.000000000000000000, 1.000000000000000000 ) ) ;
#1920 = DIRECTION ( 'NONE',  ( -0.3598999890241700306, 0.9329908884337522190, 0.000000000000000000 ) ) ;
#1921 = AXIS2_PLACEMENT_3D ( 'NONE', #25373, #30355, #8997 ) ;
#1922 = ORIENTED_EDGE ( 'NONE', *, *, #25410, .F. ) ;
#1923 = DIRECTION ( 'NONE',  ( 0.000000000000000000, 0.000000000000000000, 1.000000000000000000 ) ) ;
#1924 = LINE ( 'NONE', #1774, #18634 ) ;
#1925 = ADVANCED_FACE ( 'NONE', ( #15845 ), #27406, .F. ) ;
#1926 = CARTESIAN_POINT ( 'NONE',  ( 27.05998495714042207, -30.73416682267111000, 34.52243346884028341 ) ) ;
#1927 = EDGE_CURVE ( 'NONE', #21957, #15560, #26866, .T. ) ;
#1928 = CARTESIAN_POINT ( 'NONE',  ( 0.8762659238204211221, 8.999114229549594057, -3.621320343559650379 ) ) ;
#1929 = VERTEX_POINT ( 'NONE', #15682 ) ;
#1930 = EDGE_CURVE ( 'NONE', #5916, #2507, #1347, .T. ) ;
#1931 = DIRECTION ( 'NONE',  ( 1.000000000000000000, 0.000000000000000000, -0.000000000000000000 ) ) ;
#1932 = CARTESIAN_POINT ( 'NONE',  ( -23.96732207938974213, -33.98584080153308662, -1.500000000000000000 ) ) ;
#1933 = CARTESIAN_POINT ( 'NONE',  ( -15.00000000000004086, 1.571475800653548713E-14, 67.49999999999997158 ) ) ;
#1934 = AXIS2_PLACEMENT_3D ( 'NONE', #1818, #2262, #7111 ) ;
#1935 = ORIENTED_EDGE ( 'NONE', *, *, #16710, .F. ) ;
#1936 = EDGE_CURVE ( 'NONE', #1827, #23754, #10864, .T. ) ;
#1937 = B_SPLINE_SURFACE_WITH_KNOTS ( 'NONE', 3, 1, ( 
 ( #25467, #21206 ),
 ( #4234, #9079 ),
 ( #6729, #4540 ),
 ( #25759, #1899 ),
 ( #11261, #20757 ),
 ( #14197, #14048 ),
 ( #20915, #21379 ),
 ( #6586, #16099 ),
 ( #30438, #16240 ),
 ( #11568, #21060 ),
 ( #9224, #18740 ),
 ( #28253, #14821 ),
 ( #26380, #316 ),
 ( #773, #21844 ),
 ( #10144, #26851 ),
 ( #19356, #5310 ),
 ( #19811, #5474 ),
 ( #2518, #14975 ),
 ( #12181, #161 ),
 ( #10296, #19191 ),
 ( #9840, #29170 ),
 ( #9681, #7191 ),
 ( #16702, #24336 ),
 ( #5155, #24488 ),
 ( #3133, #625 ),
 ( #28877, #10001 ),
 ( #21995, #19649 ),
 ( #12656, #16864 ),
 ( #17007, #26529 ),
 ( #7509, #2983 ),
 ( #26211, #28715 ) ),
 .UNSPECIFIED., .F., .F., .F.,
 ( 4, 3, 3, 3, 3, 3, 3, 3, 3, 3, 4 ),
 ( 2, 2 ),
 ( 0.4999999998345681651, 0.5360336730431942698, 0.5907651151589017324, 0.6456034593241839481, 0.6998270958050443191, 0.7529536536315944995, 0.8052385063053264513, 0.8575343587103996246, 0.9106564858195047574, 0.9648414833209688624, 1.000000006602610014 ),
 ( 0.000000000000000000, 1.000000000000000000 ),
 .UNSPECIFIED. ) ;
#1938 = VECTOR ( 'NONE', #25198, 1000.000000000000000 ) ;
#1939 = CIRCLE ( 'NONE', #11900, 9.084132297865673777 ) ;
#1940 = DIRECTION ( 'NONE',  ( 0.000000000000000000, 0.000000000000000000, 1.000000000000000000 ) ) ;
#1941 = EDGE_LOOP ( 'NONE', ( #5294, #26095 ) ) ;
#1942 = B_SPLINE_CURVE_WITH_KNOTS ( 'NONE', 3,
 ( #9420, #2073, #9257, #28295, #25496, #27983, #18623, #28443, #11297, #6920, #21409, #16430, #2228, #15977, #25945, #6614 ),
 .UNSPECIFIED., .F., .F.,
 ( 4, 2, 2, 2, 2, 2, 2, 4 ),
 ( 0.5000000000000000000, 0.6250000000000004441, 0.6875000000000008882, 0.7187500000000008882, 0.7500000000000008882, 0.8125000000000006661, 0.8750000000000002220, 1.000000000000000000 ),
 .UNSPECIFIED. ) ;
#1943 = DIRECTION ( 'NONE',  ( 0.000000000000000000, -1.132880637372608986E-16, 1.000000000000000000 ) ) ;
#1944 = ADVANCED_FACE ( 'NONE', ( #20059 ), #29898, .F. ) ;
#1945 = PLANE ( 'NONE',  #16481 ) ;
#1946 = DIRECTION ( 'NONE',  ( 1.000000000000000000, 0.000000000000000000, 0.000000000000000000 ) ) ;
#1947 = ADVANCED_FACE ( 'NONE', ( #3996 ), #10402, .F. ) ;
#1948 = ORIENTED_EDGE ( 'NONE', *, *, #3915, .T. ) ;
#1949 = CARTESIAN_POINT ( 'NONE',  ( 33.56327786402390245, -10.34181101807379477, 35.63689980405263924 ) ) ;
#1950 = ADVANCED_FACE ( 'NONE', ( #20519, #3379 ), #29581, .T. ) ;
#1951 = DIRECTION ( 'NONE',  ( 1.000000000000000000, 0.000000000000000000, 0.000000000000000000 ) ) ;
#1952 = FACE_OUTER_BOUND ( 'NONE', #6640, .T. ) ;
#1953 = DIRECTION ( 'NONE',  ( 1.000000000000000000, -5.780230957810361426E-15, 0.000000000000000000 ) ) ;
#1954 = DIRECTION ( 'NONE',  ( 0.000000000000000000, 0.000000000000000000, 1.000000000000000000 ) ) ;
#1955 = VECTOR ( 'NONE', #22976, 1000.000000000000000 ) ;
#1956 = CARTESIAN_POINT ( 'NONE',  ( 3.395021109945021376, 30.50000000000000000, 24.50000000000000000 ) ) ;
#1957 = DIRECTION ( 'NONE',  ( 0.4154150130018864906, -0.9096319953545183301, 0.000000000000000000 ) ) ;
#1958 = LINE ( 'NONE', #18960, #28468 ) ;
#1959 = FACE_OUTER_BOUND ( 'NONE', #10569, .T. ) ;
#1960 = DIRECTION ( 'NONE',  ( -1.000000000000000000, 0.000000000000000000, 0.000000000000000000 ) ) ;
#1961 = DIRECTION ( 'NONE',  ( 0.000000000000000000, 1.000000000000000000, -0.000000000000000000 ) ) ;
#1962 = ORIENTED_EDGE ( 'NONE', *, *, #2846, .F. ) ;
#1963 = EDGE_LOOP ( 'NONE', ( #27185, #1518, #15732, #5340 ) ) ;
#1964 = CARTESIAN_POINT ( 'NONE',  ( 12.56641067637628240, -40.32935944494942504, -1.500000000000000000 ) ) ;
#1965 = EDGE_CURVE ( 'NONE', #6185, #27407, #6927, .T. ) ;
#1966 = CARTESIAN_POINT ( 'NONE',  ( -26.80246859415415273, -7.028748154183645624, -1.499999999999999556 ) ) ;
#1967 = EDGE_CURVE ( 'NONE', #23890, #24237, #17649, .T. ) ;
#1968 = VERTEX_POINT ( 'NONE', #11772 ) ;
#1969 = DIRECTION ( 'NONE',  ( 0.000000000000000000, 0.000000000000000000, 1.000000000000000000 ) ) ;
#1970 = CIRCLE ( 'NONE', #4441, 1.447898107987198646 ) ;
#1971 = CARTESIAN_POINT ( 'NONE',  ( 15.55167013926946140, -6.938753487154069255, 18.55820869691756769 ) ) ;
#1972 = ADVANCED_FACE ( 'NONE', ( #14100 ), #16903, .F. ) ;
#1973 = CARTESIAN_POINT ( 'NONE',  ( 4.575061044035273028, 16.40537387836875993, 7.500898271101006820 ) ) ;
#1974 = VERTEX_POINT ( 'NONE', #23609 ) ;
#1975 = CARTESIAN_POINT ( 'NONE',  ( -11.19315777850258620, -16.57474394094692371, 19.96302680909623462 ) ) ;
#1976 = EDGE_CURVE ( 'NONE', #12213, #16156, #16385, .T. ) ;
#1977 = CARTESIAN_POINT ( 'NONE',  ( 11.80864398233535795, 12.32734916534602654, 6.041646659195333058 ) ) ;
#1978 = VECTOR ( 'NONE', #13755, 1000.000000000000114 ) ;
#1979 = CARTESIAN_POINT ( 'NONE',  ( 9.590471615930072247, -1.687027447297460236, 1.500000000000001332 ) ) ;
#1980 = CARTESIAN_POINT ( 'NONE',  ( 2.212236613306092892, 42.53911549472210396, 34.61403848092495394 ) ) ;
#1981 = ORIENTED_EDGE ( 'NONE', *, *, #21356, .F. ) ;
#1982 = FACE_OUTER_BOUND ( 'NONE', #21567, .T. ) ;
#1983 = EDGE_CURVE ( 'NONE', #12192, #18134, #25856, .T. ) ;
#1984 = CARTESIAN_POINT ( 'NONE',  ( -26.58597676761596063, 6.321098805557481271, 43.43030304422423882 ) ) ;
#1985 = CARTESIAN_POINT ( 'NONE',  ( -14.81308450742032967, 13.43805957489523095, 7.267242832833945343 ) ) ;
#1986 = EDGE_LOOP ( 'NONE', ( #7812, #6825, #5779, #9715, #22803 ) ) ;
#1987 = CARTESIAN_POINT ( 'NONE',  ( 16.81826667486039639, 2.692788315295377988, 20.22273502201483453 ) ) ;
#1988 = CARTESIAN_POINT ( 'NONE',  ( 25.53015708495998837, -6.470147010658197750, 44.42018155122899969 ) ) ;
#1989 = CARTESIAN_POINT ( 'NONE',  ( 23.06931171825916493, -36.25841434086032677, -16.50000000000000000 ) ) ;
#1990 = DIRECTION ( 'NONE',  ( 0.000000000000000000, 0.000000000000000000, 1.000000000000000000 ) ) ;
#1991 = AXIS2_PLACEMENT_3D ( 'NONE', #27841, #25338, #23290 ) ;
#1992 = DIRECTION ( 'NONE',  ( -0.7071067811865487940, -8.659560562354948882E-17, -0.7071067811865463515 ) ) ;
#1993 = CYLINDRICAL_SURFACE ( 'NONE', #11539, 7.500000000000013323 ) ;
#1994 = CARTESIAN_POINT ( 'NONE',  ( -19.86072491926578110, 2.502642356747510899, 20.34789198813115263 ) ) ;
#1995 = DIRECTION ( 'NONE',  ( 1.000000000000000000, 0.000000000000000000, 0.000000000000000000 ) ) ;
#1996 = ORIENTED_EDGE ( 'NONE', *, *, #20841, .T. ) ;
#1997 = EDGE_CURVE ( 'NONE', #27352, #27365, #19892, .T. ) ;
#1998 = EDGE_CURVE ( 'NONE', #7862, #25485, #16458, .T. ) ;
#1999 = ADVANCED_FACE ( 'NONE', ( #11327 ), #14249, .F. ) ;
#2000 = VECTOR ( 'NONE', #21282, 1000.000000000000000 ) ;
#2001 = CARTESIAN_POINT ( 'NONE',  ( -5.549075634136967139, 16.11684027513961226, 5.652196082368482699 ) ) ;
#2002 = CARTESIAN_POINT ( 'NONE',  ( -13.88429941593315853, -16.69721919944146649, 1.500000000000000000 ) ) ;
#2003 = ORIENTED_EDGE ( 'NONE', *, *, #16264, .T. ) ;
#2004 = ORIENTED_EDGE ( 'NONE', *, *, #6342, .T. ) ;
#2005 = CARTESIAN_POINT ( 'NONE',  ( -15.96020336975123577, 12.05298949301765887, 6.392525840300344875 ) ) ;
#2006 = ORIENTED_EDGE ( 'NONE', *, *, #838, .T. ) ;
#2007 = CARTESIAN_POINT ( 'NONE',  ( 24.44496207165490631, -7.595930209050163029, 45.15942333309103418 ) ) ;
#2008 = VERTEX_POINT ( 'NONE', #4457 ) ;
#2009 = B_SPLINE_CURVE_WITH_KNOTS ( 'NONE', 3,
 ( #16990, #26512, #16530, #11702, #7021, #23395, #2033, #28545, #21360, #11557 ),
 .UNSPECIFIED., .F., .F.,
 ( 4, 2, 2, 2, 4 ),
 ( 0.08772604163077325767, 0.09629186329443806258, 0.1119390432090576204, 0.1197626331663674271, 0.1275862231236772337 ),
 .UNSPECIFIED. ) ;
#2010 = CARTESIAN_POINT ( 'NONE',  ( -15.43151021478632501, 12.72345061513107112, 18.34869673959212477 ) ) ;
#2011 = AXIS2_PLACEMENT_3D ( 'NONE', #26375, #24332, #9996 ) ;
#2012 = CARTESIAN_POINT ( 'NONE',  ( -24.03057240117691862, 26.57182937991348481, 26.54355021145563143 ) ) ;
#2013 = ORIENTED_EDGE ( 'NONE', *, *, #27648, .F. ) ;
#2014 = EDGE_LOOP ( 'NONE', ( #18586, #30083, #10339 ) ) ;
#2015 = DIRECTION ( 'NONE',  ( -0.000000000000000000, -0.000000000000000000, -1.000000000000000000 ) ) ;
#2016 = ORIENTED_EDGE ( 'NONE', *, *, #30517, .T. ) ;
#2017 = ORIENTED_EDGE ( 'NONE', *, *, #10988, .T. ) ;
#2018 = CARTESIAN_POINT ( 'NONE',  ( -0.1027882698221962710, -17.02358378464945687, 19.85270094495842130 ) ) ;
#2019 = CARTESIAN_POINT ( 'NONE',  ( -5.352643706120520761, -7.827050521741861999, 13.00000000000000178 ) ) ;
#2020 = LINE ( 'NONE', #12003, #27280 ) ;
#2021 = CARTESIAN_POINT ( 'NONE',  ( -9.185733585337898077, 2.352830851074200869, 1.500000000000001332 ) ) ;
#2022 = ORIENTED_EDGE ( 'NONE', *, *, #29111, .F. ) ;
#2023 = CARTESIAN_POINT ( 'NONE',  ( -16.93638505691475160, 1.872096242067391225, 18.36582235739946611 ) ) ;
#2024 = CARTESIAN_POINT ( 'NONE',  ( 2.049713242724727991, -39.50000000000001421, 34.50000000000000000 ) ) ;
#2025 = VECTOR ( 'NONE', #25260, 1000.000000000000000 ) ;
#2026 = EDGE_CURVE ( 'NONE', #18898, #12149, #21272, .T. ) ;
#2027 = CARTESIAN_POINT ( 'NONE',  ( -13.47895127716181207, 10.44112259311556379, 5.661398277488802755 ) ) ;
#2028 = CARTESIAN_POINT ( 'NONE',  ( 3.085425824774455261, 16.79642356368104927, 19.58863275299554019 ) ) ;
#2029 = ORIENTED_EDGE ( 'NONE', *, *, #8765, .F. ) ;
#2030 = ORIENTED_EDGE ( 'NONE', *, *, #27366, .F. ) ;
#2031 = EDGE_CURVE ( 'NONE', #29358, #9984, #26365, .T. ) ;
#2032 = FACE_OUTER_BOUND ( 'NONE', #19721, .T. ) ;
#2033 = CARTESIAN_POINT ( 'NONE',  ( -10.11202017158466759, 41.14070756921185534, -1.500000000000009992 ) ) ;
#2034 = CARTESIAN_POINT ( 'NONE',  ( -5.292761969338718231, 19.30549167878804440, 18.63641924841378028 ) ) ;
#2035 = DIRECTION ( 'NONE',  ( 1.000000000000000000, 0.000000000000000000, 0.000000000000000000 ) ) ;
#2036 = CARTESIAN_POINT ( 'NONE',  ( -1.438332125858111432, 8.884323311075791096, -3.621320343559650379 ) ) ;
#2037 = DIRECTION ( 'NONE',  ( -1.000000000000000000, -0.000000000000000000, -0.000000000000000000 ) ) ;
#2038 = VERTEX_POINT ( 'NONE', #30190 ) ;
#2039 = CARTESIAN_POINT ( 'NONE',  ( -19.96032475228488323, 1.513912977174407981, 6.892848776733236704 ) ) ;
#2040 = DIRECTION ( 'NONE',  ( 1.000000000000000000, 0.000000000000000000, 0.000000000000000000 ) ) ;
#2041 = CARTESIAN_POINT ( 'NONE',  ( 3.668292057955996555, -8.743977807160087323, 1.500000000000001332 ) ) ;
#2042 = ORIENTED_EDGE ( 'NONE', *, *, #21748, .F. ) ;
#2043 = FACE_OUTER_BOUND ( 'NONE', #24533, .T. ) ;
#2044 = EDGE_LOOP ( 'NONE', ( #2535, #19126, #18814, #3222 ) ) ;
#2045 = FACE_OUTER_BOUND ( 'NONE', #13773, .T. ) ;
#2046 = AXIS2_PLACEMENT_3D ( 'NONE', #10083, #19596, #29117 ) ;
#2047 = CARTESIAN_POINT ( 'NONE',  ( -19.05926965620446722, 38.91648619949726395, -16.49999999999999289 ) ) ;
#2048 = ORIENTED_EDGE ( 'NONE', *, *, #29042, .T. ) ;
#2049 = CARTESIAN_POINT ( 'NONE',  ( 29.73573388937572659, -22.26985569269989895, 27.49999999999999645 ) ) ;
#2050 = CARTESIAN_POINT ( 'NONE',  ( -39.52380524535562500, 7.028748154183637631, -11.49999999999999645 ) ) ;
#2051 = CARTESIAN_POINT ( 'NONE',  ( 2.185336383880203570, -8.817355867515820123, -1.500000000000002887 ) ) ;
#2052 = DIRECTION ( 'NONE',  ( 0.000000000000000000, 0.000000000000000000, 1.000000000000000000 ) ) ;
#2053 = CARTESIAN_POINT ( 'NONE',  ( -6.878634932266925794, 18.79866186728735400, 19.69140814234746273 ) ) ;
#2054 = DIRECTION ( 'NONE',  ( 0.000000000000000000, 0.000000000000000000, 1.000000000000000000 ) ) ;
#2055 = DIRECTION ( 'NONE',  ( 5.125319360840571077E-16, -1.000000000000000000, 0.000000000000000000 ) ) ;
#2056 = ORIENTED_EDGE ( 'NONE', *, *, #20964, .F. ) ;
#2057 = AXIS2_PLACEMENT_3D ( 'NONE', #1842, #13702, #11200 ) ;
#2058 = CARTESIAN_POINT ( 'NONE',  ( 15.47699552843811155, -7.094814489843902727, 6.031926333436656407 ) ) ;
#2059 = DIRECTION ( 'NONE',  ( 1.000000000000000000, 0.000000000000000000, 0.000000000000000000 ) ) ;
#2060 = DIRECTION ( 'NONE',  ( -0.000000000000000000, -0.000000000000000000, 1.000000000000000000 ) ) ;
#2061 = EDGE_LOOP ( 'NONE', ( #19925, #1644, #18712, #22600 ) ) ;
#2062 = CARTESIAN_POINT ( 'NONE',  ( 7.500000000000000000, -5.196152422706639129, -9.000000000000000000 ) ) ;
#2063 = CARTESIAN_POINT ( 'NONE',  ( 11.29839223038184670, -16.52442514205455026, 7.627891251804737927 ) ) ;
#2064 = CARTESIAN_POINT ( 'NONE',  ( 9.999999999999959144, 1.510243460696181139E-14, 21.50000000000000000 ) ) ;
#2065 = ADVANCED_BREP_SHAPE_REPRESENTATION ( '', ( #23377, #7396 ), #3935 ) ;
#2066 = CARTESIAN_POINT ( 'NONE',  ( 0.000000000000000000, 0.000000000000000000, 1.500000000000001332 ) ) ;
#2067 = ORIENTED_EDGE ( 'NONE', *, *, #17202, .T. ) ;
#2068 = CARTESIAN_POINT ( 'NONE',  ( 6.812559277181973627, -5.881244434206257310, -1.500000000000002220 ) ) ;
#2069 = DIRECTION ( 'NONE',  ( -0.000000000000000000, -0.000000000000000000, 1.000000000000000000 ) ) ;
#2070 = CARTESIAN_POINT ( 'NONE',  ( 8.813079928575357158, -41.51132794799057280, 28.92494092171985898 ) ) ;
#2071 = DIRECTION ( 'NONE',  ( -1.000000000000000000, 0.000000000000000000, 0.000000000000000000 ) ) ;
#2072 = VERTEX_POINT ( 'NONE', #8828 ) ;
#2073 = CARTESIAN_POINT ( 'NONE',  ( -13.55077504496076557, 10.35587614721247718, 5.653604225791663218 ) ) ;
#2074 = ORIENTED_EDGE ( 'NONE', *, *, #968, .F. ) ;
#2075 = CARTESIAN_POINT ( 'NONE',  ( -34.07766914599908148, -21.40380666528021081, -1.500000000000000000 ) ) ;
#2076 = LINE ( 'NONE', #25500, #21890 ) ;
#2077 = ORIENTED_EDGE ( 'NONE', *, *, #24044, .F. ) ;
#2078 = ORIENTED_EDGE ( 'NONE', *, *, #10320, .F. ) ;
#2079 = CARTESIAN_POINT ( 'NONE',  ( 28.79137815760242702, -9.331429872129930914, -1.500000000000000000 ) ) ;
#2080 = LINE ( 'NONE', #28140, #25328 ) ;
#2081 = ORIENTED_EDGE ( 'NONE', *, *, #17855, .T. ) ;
#2082 = CARTESIAN_POINT ( 'NONE',  ( -31.79204601741444236, -14.90874471747207686, 39.88609648712696298 ) ) ;
#2083 = CARTESIAN_POINT ( 'NONE',  ( -7.669844488642331370, -15.25924058316908827, 6.560937769032974209 ) ) ;
#2084 = VECTOR ( 'NONE', #19436, 1000.000000000000000 ) ;
#2085 = CYLINDRICAL_SURFACE ( 'NONE', #8887, 29.99999999999928946 ) ;
#2086 = CARTESIAN_POINT ( 'NONE',  ( 1.694955473231259058, -16.99033591619068773, 19.79423548914561692 ) ) ;
#2087 = ORIENTED_EDGE ( 'NONE', *, *, #20649, .F. ) ;
#2088 = CARTESIAN_POINT ( 'NONE',  ( 49.99999999999998579, 50.00000000000000000, 12.49999999999999112 ) ) ;
#2089 = DIRECTION ( 'NONE',  ( 0.000000000000000000, -1.000000000000000000, 0.000000000000000000 ) ) ;
#2090 = DIRECTION ( 'NONE',  ( 1.000000000000000000, 0.000000000000000000, 0.000000000000000000 ) ) ;
#2091 = DIRECTION ( 'NONE',  ( -1.000000000000000000, 0.000000000000000000, 0.000000000000000000 ) ) ;
#2092 = VERTEX_POINT ( 'NONE', #18350 ) ;
#2093 = PRODUCT_DEFINITION ( 'UNKNOWN', '', #6419, #16060 ) ;
#2094 = B_SPLINE_CURVE_WITH_KNOTS ( 'NONE', 3,
 ( #6785, #6951, #25974, #23611, #11774, #21275, #18965, #28473, #3192, #19882, #5682, #10516, #29236, #15178 ),
 .UNSPECIFIED., .F., .F.,
 ( 4, 2, 2, 2, 2, 2, 4 ),
 ( 2.980251112064282051E-07, 0.0007442722521831233746, 0.001488246479255040311, 0.001860233592791005501, 0.002232220706326970474, 0.002604207819862935230, 0.002976194933398900420 ),
 .UNSPECIFIED. ) ;
#2095 = DIRECTION ( 'NONE',  ( 1.000000000000000000, 0.000000000000000000, -0.000000000000000000 ) ) ;
#2096 = EDGE_CURVE ( 'NONE', #11840, #29091, #8440, .T. ) ;
#2097 = CARTESIAN_POINT ( 'NONE',  ( -15.16517293421788537, -7.781889191988407006, 20.34789198813115263 ) ) ;
#2098 = LINE ( 'NONE', #8984, #28287 ) ;
#2099 = LINE ( 'NONE', #11622, #24469 ) ;
#2100 = ADVANCED_FACE ( 'NONE', ( #25824 ), #20824, .F. ) ;
#2101 = CARTESIAN_POINT ( 'NONE',  ( 14.50629223094009035, 39.46103756294984777, 22.23272703466988887 ) ) ;
#2102 = CARTESIAN_POINT ( 'NONE',  ( -23.72845085825479572, 12.99428747377816151, 43.70389027930196590 ) ) ;
#2103 = EDGE_CURVE ( 'NONE', #7486, #17105, #15760, .T. ) ;
#2104 = CARTESIAN_POINT ( 'NONE',  ( 9.169883732660084164, -9.268939115642975679, 1.500000000000001332 ) ) ;
#2105 = CARTESIAN_POINT ( 'NONE',  ( 33.51937758206383222, -10.82799271170304323, 35.53333982454045525 ) ) ;
#2106 = VERTEX_POINT ( 'NONE', #966 ) ;
#2107 = ORIENTED_EDGE ( 'NONE', *, *, #3911, .F. ) ;
#2108 = CARTESIAN_POINT ( 'NONE',  ( -10.00000000000004263, 1.387778780781445676E-14, 1.500000000000000000 ) ) ;
#2109 = CARTESIAN_POINT ( 'NONE',  ( -25.19442432475839055, 35.44676296258369064, -19.50000000000000355 ) ) ;
#2110 = EDGE_CURVE ( 'NONE', #16733, #28141, #22382, .T. ) ;
#2111 = DIRECTION ( 'NONE',  ( 1.000000000000000000, 0.000000000000000000, 0.000000000000000000 ) ) ;
#2112 = EDGE_LOOP ( 'NONE', ( #6991, #27206 ) ) ;
#2113 = DIRECTION ( 'NONE',  ( 1.000000000000000000, 0.000000000000000000, 0.000000000000000000 ) ) ;
#2114 = CARTESIAN_POINT ( 'NONE',  ( 15.45190528822775633, -7.145941350103554690, 19.87181966307587544 ) ) ;
#2115 = EDGE_CURVE ( 'NONE', #12148, #22258, #12417, .T. ) ;
#2116 = CARTESIAN_POINT ( 'NONE',  ( 5.524396280439209939, 19.24072699314231727, 7.632642797338977658 ) ) ;
#2117 = EDGE_CURVE ( 'NONE', #28435, #9405, #12931, .T. ) ;
#2118 = VERTEX_POINT ( 'NONE', #17813 ) ;
#2119 = CARTESIAN_POINT ( 'NONE',  ( 4.994189150946232836, 16.27260345083323756, 19.56050940960062690 ) ) ;
#2120 = PLANE ( 'NONE',  #11256 ) ;
#2121 = FACE_OUTER_BOUND ( 'NONE', #29788, .T. ) ;
#2122 = CARTESIAN_POINT ( 'NONE',  ( -33.54031841762500932, 21.84949147252275381, 30.89863097042385931 ) ) ;
#2123 = ORIENTED_EDGE ( 'NONE', *, *, #24038, .F. ) ;
#2124 = DIRECTION ( 'NONE',  ( 0.000000000000000000, 0.000000000000000000, 1.000000000000000000 ) ) ;
#2125 = VECTOR ( 'NONE', #190, 1000.000000000000000 ) ;
#2126 = VECTOR ( 'NONE', #2316, 1000.000000000000000 ) ;
#2127 = AXIS2_PLACEMENT_3D ( 'NONE', #16002, #25522, #22698 ) ;
#2128 = CARTESIAN_POINT ( 'NONE',  ( 8.413215745754998309, -3.196529495465417980, -3.621320343559650379 ) ) ;
#2129 = CARTESIAN_POINT ( 'NONE',  ( -57.50000000000001421, -50.00000000000000000, 12.49999999999999112 ) ) ;
#2130 = VERTEX_POINT ( 'NONE', #14428 ) ;
#2131 = CARTESIAN_POINT ( 'NONE',  ( -32.82330813384395185, 22.94799032727105370, -1.500000000000000000 ) ) ;
#2132 = EDGE_CURVE ( 'NONE', #24759, #6184, #9736, .T. ) ;
#2133 =( NAMED_UNIT ( * ) SI_UNIT ( $, .STERADIAN. ) SOLID_ANGLE_UNIT ( ) );
#2134 = EDGE_CURVE ( 'NONE', #12801, #20802, #16920, .T. ) ;
#2135 = CARTESIAN_POINT ( 'NONE',  ( 5.229169525036386545, -43.72378943593913192, -16.49999999999999289 ) ) ;
#2136 = CARTESIAN_POINT ( 'NONE',  ( 0.2355109517537151975, -20.01673911375432624, 7.652108011868850035 ) ) ;
#2137 = EDGE_CURVE ( 'NONE', #22258, #26398, #30829, .T. ) ;
#2138 = ADVANCED_FACE ( 'NONE', ( #20141 ), #26435, .F. ) ;
#2139 = CARTESIAN_POINT ( 'NONE',  ( 32.98805937973593672, 0.000000000000000000, 13.00000000000000178 ) ) ;
#2140 = FACE_OUTER_BOUND ( 'NONE', #17021, .T. ) ;
#2141 = CARTESIAN_POINT ( 'NONE',  ( -17.01545599012840526, 1.214108451629964058, 20.25542030744407640 ) ) ;
#2142 = LINE ( 'NONE', #2458, #29836 ) ;
#2143 = ORIENTED_EDGE ( 'NONE', *, *, #25575, .T. ) ;
#2144 = EDGE_CURVE ( 'NONE', #30466, #1099, #21366, .T. ) ;
#2145 = FACE_OUTER_BOUND ( 'NONE', #28041, .T. ) ;
#2146 = CARTESIAN_POINT ( 'NONE',  ( 11.52197458429827037, 37.50933785548059518, 34.80090346875809360 ) ) ;
#2147 = ORIENTED_EDGE ( 'NONE', *, *, #15449, .T. ) ;
#2148 = ORIENTED_EDGE ( 'NONE', *, *, #10232, .T. ) ;
#2149 = EDGE_CURVE ( 'NONE', #11604, #2369, #16151, .T. ) ;
#2150 = CIRCLE ( 'NONE', #25556, 3.000000000000002665 ) ;
#2151 = CARTESIAN_POINT ( 'NONE',  ( 5.163176754322200246, 19.32250783072323586, 18.34869673959212122 ) ) ;
#2152 = ADVANCED_FACE ( 'NONE', ( #24081 ), #22326, .T. ) ;
#2153 = CIRCLE ( 'NONE', #29051, 37.60050224823048381 ) ;
#2154 = VERTEX_POINT ( 'NONE', #5221 ) ;
#2155 = FACE_OUTER_BOUND ( 'NONE', #1137, .T. ) ;
#2156 = FACE_BOUND ( 'NONE', #12173, .T. ) ;
#2157 = EDGE_LOOP ( 'NONE', ( #5767, #21097, #13023 ) ) ;
#2158 = LINE ( 'NONE', #20876, #18238 ) ;
#2159 = DIRECTION ( 'NONE',  ( 0.000000000000000000, 0.000000000000000000, 1.000000000000000000 ) ) ;
#2160 = ORIENTED_EDGE ( 'NONE', *, *, #16829, .T. ) ;
#2161 = CARTESIAN_POINT ( 'NONE',  ( 0.000000000000000000, 0.000000000000000000, -16.50000000000000000 ) ) ;
#2162 = ORIENTED_EDGE ( 'NONE', *, *, #238, .F. ) ;
#2163 = EDGE_CURVE ( 'NONE', #20389, #2236, #1117, .T. ) ;
#2164 = DIRECTION ( 'NONE',  ( 1.000000000000000000, 0.000000000000000000, 0.000000000000000000 ) ) ;
#2165 = EDGE_CURVE ( 'NONE', #28271, #28669, #8297, .T. ) ;
#2166 = AXIS2_PLACEMENT_3D ( 'NONE', #17378, #7866, #26899 ) ;
#2167 = VERTEX_POINT ( 'NONE', #23767 ) ;
#2168 = ORIENTED_EDGE ( 'NONE', *, *, #26325, .T. ) ;
#2169 = CIRCLE ( 'NONE', #23573, 1.000000000000008438 ) ;
#2170 = EDGE_CURVE ( 'NONE', #18929, #12149, #21437, .T. ) ;
#2171 = VECTOR ( 'NONE', #29665, 1000.000000000000000 ) ;
#2172 = PLANE ( 'NONE',  #6139 ) ;
#2173 = CARTESIAN_POINT ( 'NONE',  ( 0.5152247664106277547, -17.03071091119081615, 20.32222155561919053 ) ) ;
#2174 = LINE ( 'NONE', #21178, #5076 ) ;
#2175 = CARTESIAN_POINT ( 'NONE',  ( -23.07950435457404481, 11.62838985844542883, 49.15679243825150024 ) ) ;
#2176 = FACE_BOUND ( 'NONE', #19630, .T. ) ;
#2177 = ORIENTED_EDGE ( 'NONE', *, *, #2506, .T. ) ;
#2178 = CARTESIAN_POINT ( 'NONE',  ( 9.669732009941352402, -14.02977311367123647, 7.632642797338977658 ) ) ;
#2179 = DIRECTION ( 'NONE',  ( -1.000000000000000000, 0.000000000000000000, 0.000000000000000000 ) ) ;
#2180 = CARTESIAN_POINT ( 'NONE',  ( 8.413215745754998309, -3.196529495465417980, 21.50000000000000000 ) ) ;
#2181 = ORIENTED_EDGE ( 'NONE', *, *, #17821, .F. ) ;
#2182 = ORIENTED_EDGE ( 'NONE', *, *, #12436, .F. ) ;
#2183 = CARTESIAN_POINT ( 'NONE',  ( 18.33792385446292883, -7.982495159855863776, 18.34798005863227388 ) ) ;
#2184 = CARTESIAN_POINT ( 'NONE',  ( 49.99999999999998579, -50.00000000000000000, 12.49999999999998401 ) ) ;
#2185 = CARTESIAN_POINT ( 'NONE',  ( 15.21635490854753847, 12.97988522761634655, 20.22277707861861984 ) ) ;
#2186 = CARTESIAN_POINT ( 'NONE',  ( -5.460567910819448478, 19.25894470870317932, 18.49267272388512140 ) ) ;
#2187 = B_SPLINE_CURVE_WITH_KNOTS ( 'NONE', 3,
 ( #14332, #21037, #12156, #21655, #9052, #7167, #18872, #23529, #14485, #14171, #2175, #21497 ),
 .UNSPECIFIED., .F., .F.,
 ( 4, 2, 2, 2, 2, 4 ),
 ( 2.975096543306551241E-07, 0.0007805422437037903925, 0.001560786977753250097, 0.002341031711802709584, 0.002731154078827434124, 0.003121276445852158229 ),
 .UNSPECIFIED. ) ;
#2188 = DIRECTION ( 'NONE',  ( 0.000000000000000000, 0.000000000000000000, 1.000000000000000000 ) ) ;
#2189 = DIRECTION ( 'NONE',  ( 0.000000000000000000, 0.000000000000000000, -1.000000000000000000 ) ) ;
#2190 = AXIS2_PLACEMENT_3D ( 'NONE', #7061, #2386, #6916 ) ;
#2191 = CARTESIAN_POINT ( 'NONE',  ( -5.124412594240641106, 19.33243322302223532, 7.156831654632821227 ) ) ;
#2192 = EDGE_LOOP ( 'NONE', ( #1641, #28752 ) ) ;
#2193 = CARTESIAN_POINT ( 'NONE',  ( -17.04815991962220068, 0.8662532504481914586, 7.280727868105637768 ) ) ;
#2194 = DIRECTION ( 'NONE',  ( 1.000000000000000000, 0.000000000000000000, 0.000000000000000000 ) ) ;
#2195 = CARTESIAN_POINT ( 'NONE',  ( 40.05104235265675783, -2.353288714521556191, -6.500000000000000888 ) ) ;
#2196 = ORIENTED_EDGE ( 'NONE', *, *, #15690, .F. ) ;
#2197 = DIRECTION ( 'NONE',  ( 0.000000000000000000, 1.000000000000000000, 0.000000000000000000 ) ) ;
#2198 = ORIENTED_EDGE ( 'NONE', *, *, #12967, .F. ) ;
#2199 = EDGE_CURVE ( 'NONE', #28757, #3557, #22108, .T. ) ;
#2200 = FACE_OUTER_BOUND ( 'NONE', #9290, .T. ) ;
#2201 = DIRECTION ( 'NONE',  ( -0.000000000000000000, -0.000000000000000000, 1.000000000000000000 ) ) ;
#2202 = EDGE_LOOP ( 'NONE', ( #4000, #3710 ) ) ;
#2203 = CARTESIAN_POINT ( 'NONE',  ( 32.30280224124133781, 17.44315250269476891, 27.50000000000000711 ) ) ;
#2204 = CARTESIAN_POINT ( 'NONE',  ( 0.000000000000000000, 0.000000000000000000, 9.000000000000000000 ) ) ;
#2205 = CARTESIAN_POINT ( 'NONE',  ( -16.96496224101209194, 1.652369717150044659, 7.652108011868850923 ) ) ;
#2206 = CARTESIAN_POINT ( 'NONE',  ( 0.000000000000000000, 0.000000000000000000, 1.500000000000000000 ) ) ;
#2207 = CARTESIAN_POINT ( 'NONE',  ( -5.870757325077153865, 16.01346137069357312, 18.39992786714538298 ) ) ;
#2208 = VECTOR ( 'NONE', #8117, 1000.000000000000000 ) ;
#2209 = DIRECTION ( 'NONE',  ( 0.000000000000000000, 0.000000000000000000, 1.000000000000000000 ) ) ;
#2210 = CARTESIAN_POINT ( 'NONE',  ( 6.899999999999999467, 10.39230484541327471, 0.000000000000000000 ) ) ;
#2211 = CARTESIAN_POINT ( 'NONE',  ( 0.000000000000000000, 0.000000000000000000, 1.500000000000001332 ) ) ;
#2212 = ORIENTED_EDGE ( 'NONE', *, *, #23274, .T. ) ;
#2213 = CARTESIAN_POINT ( 'NONE',  ( 5.291489565152559749, 19.28730510418394672, 18.34798005863226678 ) ) ;
#2214 = CARTESIAN_POINT ( 'NONE',  ( 2.552544031601107211, 42.49999999998228617, -1.500000000000000000 ) ) ;
#2215 = FACE_OUTER_BOUND ( 'NONE', #8737, .T. ) ;
#2216 = ORIENTED_EDGE ( 'NONE', *, *, #26162, .F. ) ;
#2217 = CARTESIAN_POINT ( 'NONE',  ( 24.03057240117691862, 26.57182937991349903, 26.54355021145562787 ) ) ;
#2218 = CARTESIAN_POINT ( 'NONE',  ( -17.77905984561984454, -9.199004478715989919, 20.13759033520874908 ) ) ;
#2219 = DIRECTION ( 'NONE',  ( 1.000000000000000000, 0.000000000000000000, 0.000000000000000000 ) ) ;
#2220 = CARTESIAN_POINT ( 'NONE',  ( 0.01899995639453604460, 8.236198097127175544, 3.734486434573633495 ) ) ;
#2221 = CARTESIAN_POINT ( 'NONE',  ( 35.76344986165623396, 22.29344514668041199, -19.50000000000000355 ) ) ;
#2222 = ORIENTED_EDGE ( 'NONE', *, *, #23631, .T. ) ;
#2223 = CARTESIAN_POINT ( 'NONE',  ( 0.3518703668723784928, -19.99690444156084723, 20.34789198813115263 ) ) ;
#2224 = CARTESIAN_POINT ( 'NONE',  ( -1.000000000000016875, 29.50000000000000000, 24.50000000000000000 ) ) ;
#2225 = CARTESIAN_POINT ( 'NONE',  ( 24.72409811164068572, 32.98527725324579052, 29.74032444299796296 ) ) ;
#2226 = FACE_BOUND ( 'NONE', #16094, .T. ) ;
#2227 = ORIENTED_EDGE ( 'NONE', *, *, #29644, .F. ) ;
#2228 = CARTESIAN_POINT ( 'NONE',  ( -13.88572908622542812, 9.930151408543668623, 7.269896094239229889 ) ) ;
#2229 = DIRECTION ( 'NONE',  ( 1.000000000000000000, 0.000000000000000000, 0.000000000000000000 ) ) ;
#2230 = CYLINDRICAL_SURFACE ( 'NONE', #24903, 20.00000000000000000 ) ;
#2231 = VERTEX_POINT ( 'NONE', #10865 ) ;
#2232 = CIRCLE ( 'NONE', #25147, 1.000000000000011324 ) ;
#2233 = VERTEX_POINT ( 'NONE', #27703 ) ;
#2234 = DIRECTION ( 'NONE',  ( 1.000000000000000000, 0.000000000000000000, 0.000000000000000000 ) ) ;
#2235 = EDGE_CURVE ( 'NONE', #24520, #11332, #7958, .T. ) ;
#2236 = VERTEX_POINT ( 'NONE', #22859 ) ;
#2237 = CARTESIAN_POINT ( 'NONE',  ( -0.5073662589470785411, -20.01152162034081528, 18.80699882434806369 ) ) ;
#2238 = CARTESIAN_POINT ( 'NONE',  ( -10.14924625765043587, -17.25430667454971356, 7.559636331181775581 ) ) ;
#2239 = DIRECTION ( 'NONE',  ( 1.000000000000000000, 0.000000000000000000, 0.000000000000000000 ) ) ;
#2240 = CARTESIAN_POINT ( 'NONE',  ( 0.5800982118606496929, -20.00934090639730201, 18.37415474056476938 ) ) ;
#2241 = VERTEX_POINT ( 'NONE', #17140 ) ;
#2242 = DIRECTION ( 'NONE',  ( 1.000000000000000000, -1.559722691008415723E-11, 0.000000000000000000 ) ) ;
#2243 = DIRECTION ( 'NONE',  ( 0.000000000000000000, 0.000000000000000000, 1.000000000000000000 ) ) ;
#2244 = CARTESIAN_POINT ( 'NONE',  ( 0.9714284548196561175, -19.97661650614234929, 20.15039051365863543 ) ) ;
#2245 = CARTESIAN_POINT ( 'NONE',  ( 1.224646799147357201E-15, -10.00000000000005329, 117.5000000000000000 ) ) ;
#2246 = ORIENTED_EDGE ( 'NONE', *, *, #18754, .T. ) ;
#2247 = DIRECTION ( 'NONE',  ( 0.6548607339452782172, -0.7557495743542642641, 0.000000000000000000 ) ) ;
#2248 = CARTESIAN_POINT ( 'NONE',  ( -13.04869608149710558, 10.94699654838865222, 20.22273502201483453 ) ) ;
#2249 = AXIS2_PLACEMENT_3D ( 'NONE', #8441, #17784, #27145 ) ;
#2250 = PLANE ( 'NONE',  #26984 ) ;
#2251 = CARTESIAN_POINT ( 'NONE',  ( -23.13391957319673864, -11.02874123662317984, 49.37194155098371340 ) ) ;
#2252 = CARTESIAN_POINT ( 'NONE',  ( -18.04365185506139113, -8.627086862512678422, 20.34789198813115263 ) ) ;
#2253 = CARTESIAN_POINT ( 'NONE',  ( -18.20359163036460615, -8.327231829331820379, 20.29090034784956131 ) ) ;
#2254 = CARTESIAN_POINT ( 'NONE',  ( 32.82330813384209023, -22.94799032726822929, -1.500000000000000000 ) ) ;
#2255 = ORIENTED_EDGE ( 'NONE', *, *, #24890, .F. ) ;
#2256 = VERTEX_POINT ( 'NONE', #20520 ) ;
#2257 = CYLINDRICAL_SURFACE ( 'NONE', #24911, 0.7500000000000006661 ) ;
#2258 = CARTESIAN_POINT ( 'NONE',  ( 5.105024945674004222, 42.22604126506330857, -1.500000000000000000 ) ) ;
#2259 = DIRECTION ( 'NONE',  ( -0.000000000000000000, -0.000000000000000000, -1.000000000000000000 ) ) ;
#2260 = CARTESIAN_POINT ( 'NONE',  ( 11.83211694375101253, -16.12463123479446381, 19.85730954408919757 ) ) ;
#2261 = VERTEX_POINT ( 'NONE', #13366 ) ;
#2262 = DIRECTION ( 'NONE',  ( 0.000000000000000000, 0.000000000000000000, 1.000000000000000000 ) ) ;
#2263 = CARTESIAN_POINT ( 'NONE',  ( 18.08817148584474310, -8.575141465928741269, 20.12545155307891065 ) ) ;
#2264 = COLOUR_RGB ( '',0.7921568627450980005, 0.8196078431372548767, 0.9333333333333333481 ) ;
#2265 = CARTESIAN_POINT ( 'NONE',  ( 6.127899591227619069, 19.05688428395638923, 7.176035686813569292 ) ) ;
#2266 = EDGE_CURVE ( 'NONE', #580, #21713, #19371, .T. ) ;
#2267 = ORIENTED_EDGE ( 'NONE', *, *, #11841, .F. ) ;
#2268 = CARTESIAN_POINT ( 'NONE',  ( 0.000000000000000000, 0.000000000000000000, 1.500000000000001332 ) ) ;
#2269 = CARTESIAN_POINT ( 'NONE',  ( 5.687793815610356241, -6.974883619896809606, 1.500000000000001332 ) ) ;
#2270 = CARTESIAN_POINT ( 'NONE',  ( -21.58118279630250314, -37.32782027973600947, -16.50000000000000000 ) ) ;
#2271 = CARTESIAN_POINT ( 'NONE',  ( -23.13757476351621989, 34.33072287895263486, 34.50373710099040636 ) ) ;
#2272 = VERTEX_POINT ( 'NONE', #15535 ) ;
#2273 = CARTESIAN_POINT ( 'NONE',  ( 9.169883732660084164, -9.268939115642975679, 1.500000000000001332 ) ) ;
#2274 = AXIS2_PLACEMENT_3D ( 'NONE', #940, #5771, #25682 ) ;
#2275 = ADVANCED_FACE ( 'NONE', ( #22124, #27555, #25049, #17464, #14800, #750 ), #2967, .T. ) ;
#2276 = LINE ( 'NONE', #7270, #18049 ) ;
#2277 = AXIS2_PLACEMENT_3D ( 'NONE', #21988, #27456, #22297 ) ;
#2278 = DIRECTION ( 'NONE',  ( -0.000000000000000000, -0.000000000000000000, -1.000000000000000000 ) ) ;
#2279 = ORIENTED_EDGE ( 'NONE', *, *, #15617, .F. ) ;
#2280 = CARTESIAN_POINT ( 'NONE',  ( -18.20359163036459194, -8.327231829331816826, 7.595116371587256054 ) ) ;
#2281 = CARTESIAN_POINT ( 'NONE',  ( -6.187077094091591789, 11.47693674426096955, 24.50000000000000000 ) ) ;
#2282 = DIRECTION ( 'NONE',  ( 0.000000000000000000, 0.000000000000000000, 1.000000000000000000 ) ) ;
#2283 = CIRCLE ( 'NONE', #19724, 15.00000000000000000 ) ;
#2284 = CARTESIAN_POINT ( 'NONE',  ( -9.958038337755704461, 17.34466697471556884, 1.500000000000001332 ) ) ;
#2285 = EDGE_CURVE ( 'NONE', #15211, #1760, #19789, .T. ) ;
#2286 = LINE ( 'NONE', #18678, #87 ) ;
#2287 = CARTESIAN_POINT ( 'NONE',  ( -17.05861610865857259, 0.7402736376837835142, 19.79423548914561692 ) ) ;
#2288 = CARTESIAN_POINT ( 'NONE',  ( -7.730328572437709767, 4.608906612435681005, 21.50000000000000000 ) ) ;
#2289 = ORIENTED_EDGE ( 'NONE', *, *, #8671, .F. ) ;
#2290 = CARTESIAN_POINT ( 'NONE',  ( 10.69045173577873697, -13.31838649416133080, 19.47783254395485031 ) ) ;
#2291 = CARTESIAN_POINT ( 'NONE',  ( -22.95669091611927826, 27.54300778121952220, 1.500000000000000000 ) ) ;
#2292 = VERTEX_POINT ( 'NONE', #26986 ) ;
#2293 = EDGE_LOOP ( 'NONE', ( #27478, #25017 ) ) ;
#2294 = AXIS2_PLACEMENT_3D ( 'NONE', #25091, #27442, #6218 ) ;
#2295 = CARTESIAN_POINT ( 'NONE',  ( -50.00000000000000000, 50.00000000000000000, -92.50000000000000000 ) ) ;
#2296 = CIRCLE ( 'NONE', #18331, 1.000000000000007772 ) ;
#2297 =( NAMED_UNIT ( * ) PLANE_ANGLE_UNIT ( ) SI_UNIT ( $, .RADIAN. ) );
#2298 = VERTEX_POINT ( 'NONE', #18040 ) ;
#2299 = AXIS2_PLACEMENT_3D ( 'NONE', #17276, #15551, #26809 ) ;
#2300 = CARTESIAN_POINT ( 'NONE',  ( 15.04974025769138990, 13.19961543621590749, 20.32842677360128292 ) ) ;
#2301 = EDGE_CURVE ( 'NONE', #19148, #6231, #13523, .T. ) ;
#2302 = FACE_OUTER_BOUND ( 'NONE', #17026, .T. ) ;
#2303 = ORIENTED_EDGE ( 'NONE', *, *, #20028, .T. ) ;
#2304 = EDGE_CURVE ( 'NONE', #4693, #15666, #15040, .T. ) ;
#2305 = CARTESIAN_POINT ( 'NONE',  ( 32.24119409414369386, 26.76047229433004659, -16.50000600000000262 ) ) ;
#2306 = CARTESIAN_POINT ( 'NONE',  ( -15.96020336975123577, 12.05298949301765177, 19.08830981656265635 ) ) ;
#2307 = CARTESIAN_POINT ( 'NONE',  ( -24.44496207165490276, 7.595930209050158588, 49.40206402021040333 ) ) ;
#2308 = ORIENTED_EDGE ( 'NONE', *, *, #9530, .F. ) ;
#2309 = VERTEX_POINT ( 'NONE', #18964 ) ;
#2310 = EDGE_CURVE ( 'NONE', #20027, #22947, #13896, .T. ) ;
#2311 = ORIENTED_EDGE ( 'NONE', *, *, #22140, .T. ) ;
#2312 = EDGE_CURVE ( 'NONE', #18831, #12912, #21331, .T. ) ;
#2313 = VECTOR ( 'NONE', #14202, 1000.000000000000000 ) ;
#2314 = ADVANCED_FACE ( 'NONE', ( #28155 ), #1658, .F. ) ;
#2315 = CIRCLE ( 'NONE', #19756, 9.482273699623480212 ) ;
#2316 = DIRECTION ( 'NONE',  ( 0.000000000000000000, 0.000000000000000000, -1.000000000000000000 ) ) ;
#2317 = DIRECTION ( 'NONE',  ( -0.000000000000000000, 1.000000000000000000, -0.000000000000000000 ) ) ;
#2318 = CONICAL_SURFACE ( 'NONE', #8336, 9.000000000000000000, 1.047197551196600296 ) ;
#2319 = CARTESIAN_POINT ( 'NONE',  ( 1.497940275966470614, -17.00196529467652340, 7.366751648393900176 ) ) ;
#2320 = EDGE_CURVE ( 'NONE', #6658, #18599, #1807, .T. ) ;
#2321 = CARTESIAN_POINT ( 'NONE',  ( -9.534095299299449877, -41.21642526093817338, 28.95179448440414660 ) ) ;
#2322 = DIRECTION ( 'NONE',  ( 1.000000000000000000, 0.000000000000000000, 0.000000000000000000 ) ) ;
#2323 = CARTESIAN_POINT ( 'NONE',  ( 19.84003625978226637, 2.664153601443035146, 18.49267272388512140 ) ) ;
#2324 = ORIENTED_EDGE ( 'NONE', *, *, #18426, .T. ) ;
#2325 = CARTESIAN_POINT ( 'NONE',  ( 9.489008252200360261, -14.14611184196831495, 7.557577766377196582 ) ) ;
#2326 = CARTESIAN_POINT ( 'NONE',  ( 19.07166558422281355, -33.51611795593300513, 34.49999999999998579 ) ) ;
#2327 = CYLINDRICAL_SURFACE ( 'NONE', #892, 50.00000000000000000 ) ;
#2328 = CIRCLE ( 'NONE', #819, 1.000000000000008438 ) ;
#2329 = CARTESIAN_POINT ( 'NONE',  ( -33.42925964089140933, 11.06161099612212695, 35.54550565580014876 ) ) ;
#2330 = ORIENTED_EDGE ( 'NONE', *, *, #28057, .F. ) ;
#2331 = EDGE_LOOP ( 'NONE', ( #12248, #847, #22485, #24740 ) ) ;
#2332 = CARTESIAN_POINT ( 'NONE',  ( 40.05104235265675783, -2.353288714521559744, -11.49999999999999645 ) ) ;
#2333 = FACE_OUTER_BOUND ( 'NONE', #1535, .T. ) ;
#2334 = CARTESIAN_POINT ( 'NONE',  ( 9.755064781586030520, 13.32952022457704544, -0.6213203435596476032 ) ) ;
#2335 = DIRECTION ( 'NONE',  ( 0.000000000000000000, -1.132880637372608986E-16, 1.000000000000000000 ) ) ;
#2336 = DIRECTION ( 'NONE',  ( 0.000000000000000000, 1.000000000000000000, 1.156482317317869999E-16 ) ) ;
#2337 = CARTESIAN_POINT ( 'NONE',  ( -34.94982008328430823, 9.785536899246608300, 27.50000000000000355 ) ) ;
#2338 = CIRCLE ( 'NONE', #13823, 9.482273699623480212 ) ;
#2339 = ADVANCED_FACE ( 'NONE', ( #4289 ), #25973, .F. ) ;
#2340 = CARTESIAN_POINT ( 'NONE',  ( -5.026174198947135352, 19.35820631361449884, 6.913388067999415298 ) ) ;
#2341 = ORIENTED_EDGE ( 'NONE', *, *, #15669, .F. ) ;
#2342 = ADVANCED_FACE ( 'NONE', ( #18805 ), #23083, .T. ) ;
#2343 = CIRCLE ( 'NONE', #12833, 9.482273699623480212 ) ;
#2344 = DIRECTION ( 'NONE',  ( 1.000000000000000000, 0.000000000000000000, 0.000000000000000000 ) ) ;
#2345 = DIRECTION ( 'NONE',  ( 0.000000000000000000, 0.000000000000000000, 1.000000000000000000 ) ) ;
#2346 = EDGE_CURVE ( 'NONE', #2236, #27891, #22862, .T. ) ;
#2347 = DIRECTION ( 'NONE',  ( -0.000000000000000000, -0.000000000000000000, 1.000000000000000000 ) ) ;
#2348 = ORIENTED_EDGE ( 'NONE', *, *, #30410, .T. ) ;
#2349 = CYLINDRICAL_SURFACE ( 'NONE', #18326, 20.00000000000000355 ) ;
#2350 = ORIENTED_EDGE ( 'NONE', *, *, #2149, .F. ) ;
#2351 = AXIS2_PLACEMENT_3D ( 'NONE', #25921, #6892, #16406 ) ;
#2352 = DIRECTION ( 'NONE',  ( 0.000000000000000000, 0.000000000000000000, 1.000000000000000000 ) ) ;
#2353 = UNCERTAINTY_MEASURE_WITH_UNIT (LENGTH_MEASURE( 1.000000000000000082E-05 ), #10820, 'distance_accuracy_value', 'NONE');
#2354 = VECTOR ( 'NONE', #3453, 1000.000000000000000 ) ;
#2355 = CARTESIAN_POINT ( 'NONE',  ( -19.85060193104290960, 38.44128451546529845, -16.49999999999999645 ) ) ;
#2356 = VECTOR ( 'NONE', #14992, 1000.000000000000114 ) ;
#2357 = ORIENTED_EDGE ( 'NONE', *, *, #7891, .F. ) ;
#2358 = CARTESIAN_POINT ( 'NONE',  ( 9.775490391764725118, 38.10998157767718908, 27.50000000000000355 ) ) ;
#2359 = CLOSED_SHELL ( 'NONE', ( #30752, #4651, #16613, #18838, #2702, #10709, #14144, #2545, #28819, #29250, #25498, #1789, #7141, #24614, #25569, #3111, #20463, #29219, #11132, #29966, #9178, #7035, #14131, #8068, #25389, #12788, #19144, #614, #13567 ) ) ;
#2360 = EDGE_CURVE ( 'NONE', #14759, #11459, #10203, .T. ) ;
#2361 = CARTESIAN_POINT ( 'NONE',  ( 0.9970077338578161585, 49.99999999999997158, -40.00000000000000000 ) ) ;
#2362 = CARTESIAN_POINT ( 'NONE',  ( 10.68714603011733288, -13.32085008214098210, 19.21769074125273491 ) ) ;
#2363 = CARTESIAN_POINT ( 'NONE',  ( 0.9621688436939446198, 9.033033306777459970, -1.500000000000000666 ) ) ;
#2364 = AXIS2_PLACEMENT_3D ( 'NONE', #4195, #30096, #18246 ) ;
#2365 = AXIS2_PLACEMENT_3D ( 'NONE', #6048, #15398, #15710 ) ;
#2366 = FACE_OUTER_BOUND ( 'NONE', #5694, .T. ) ;
#2367 = DIRECTION ( 'NONE',  ( 6.216092455583553496E-15, 1.000000000000000000, 0.000000000000000000 ) ) ;
#2368 = DIRECTION ( 'NONE',  ( -0.5406408174555976665, 0.8412535328311812055, 0.000000000000000000 ) ) ;
#2369 = VERTEX_POINT ( 'NONE', #26273 ) ;
#2370 = CARTESIAN_POINT ( 'NONE',  ( 15.57266529552203416, 38.96488032230103471, -1.500000000000000000 ) ) ;
#2371 = CARTESIAN_POINT ( 'NONE',  ( 23.96732207937828463, 33.98584080152456011, -1.500000000000000000 ) ) ;
#2372 = FACE_OUTER_BOUND ( 'NONE', #19598, .T. ) ;
#2373 = ORIENTED_EDGE ( 'NONE', *, *, #8208, .T. ) ;
#2374 = PLANE ( 'NONE',  #15534 ) ;
#2375 = DIRECTION ( 'NONE',  ( -0.000000000000000000, -1.000000000000000000, -0.000000000000000000 ) ) ;
#2376 = AXIS2_PLACEMENT_3D ( 'NONE', #26555, #24830, #5183 ) ;
#2377 = DIRECTION ( 'NONE',  ( -0.000000000000000000, -0.000000000000000000, -1.000000000000000000 ) ) ;
#2378 = EDGE_CURVE ( 'NONE', #27015, #15437, #25366, .T. ) ;
#2379 = LINE ( 'NONE', #26705, #18270 ) ;
#2380 = VECTOR ( 'NONE', #13548, 1000.000000000000000 ) ;
#2381 = EDGE_CURVE ( 'NONE', #17270, #19224, #29354, .T. ) ;
#2382 = CARTESIAN_POINT ( 'NONE',  ( 13.22505861668094340, 42.10773672057246841, -19.50000000000000355 ) ) ;
#2383 = CIRCLE ( 'NONE', #10361, 0.7500000000000024425 ) ;
#2384 = ORIENTED_EDGE ( 'NONE', *, *, #13636, .F. ) ;
#2385 = DIRECTION ( 'NONE',  ( -0.000000000000000000, -0.000000000000000000, -1.000000000000000000 ) ) ;
#2386 = DIRECTION ( 'NONE',  ( 0.000000000000000000, 0.000000000000000000, 1.000000000000000000 ) ) ;
#2387 = CARTESIAN_POINT ( 'NONE',  ( 31.22614026363978112, 25.47088236078499079, 30.52195406502089980 ) ) ;
#2388 = CARTESIAN_POINT ( 'NONE',  ( -6.560142022084716196, 18.89374015187017264, 7.454606537396340826 ) ) ;
#2389 = ORIENTED_EDGE ( 'NONE', *, *, #12052, .T. ) ;
#2390 = DIRECTION ( 'NONE',  ( 1.000000000000000000, 0.000000000000000000, -0.000000000000000000 ) ) ;
#2392 = VERTEX_POINT ( 'NONE', #382 ) ;
#2391 = VECTOR ( 'NONE', #9153, 1000.000000000000000 ) ;
#2393 = CARTESIAN_POINT ( 'NONE',  ( -5.105024945675580739, -42.22604126506273303, -1.500000000000000000 ) ) ;
#2394 = DIRECTION ( 'NONE',  ( -0.000000000000000000, -0.000000000000000000, 1.000000000000000000 ) ) ;
#2395 = AXIS2_PLACEMENT_3D ( 'NONE', #18603, #30445, #25477 ) ;
#2396 = ORIENTED_EDGE ( 'NONE', *, *, #5540, .F. ) ;
#2397 = VERTEX_POINT ( 'NONE', #9900 ) ;
#2398 = CARTESIAN_POINT ( 'NONE',  ( -30.38302862529102910, -15.53680216053817986, 36.63232123326689305 ) ) ;
#2399 = ORIENTED_EDGE ( 'NONE', *, *, #24487, .T. ) ;
#2400 = ORIENTED_EDGE ( 'NONE', *, *, #26325, .F. ) ;
#2401 = CARTESIAN_POINT ( 'NONE',  ( -0.4512825100096619080, -20.01288639008904369, 19.96783386855779341 ) ) ;
#2402 = CIRCLE ( 'NONE', #20333, 6.600000000000001421 ) ;
#2403 = CARTESIAN_POINT ( 'NONE',  ( -7.715867830805696492, -15.23386229593461216, 6.341840715582230281 ) ) ;
#2404 = VECTOR ( 'NONE', #10692, 1000.000000000000114 ) ;
#2405 = LINE ( 'NONE', #17052, #29792 ) ;
#2406 = CARTESIAN_POINT ( 'NONE',  ( 1.121436987360517445, -17.01878714021719929, 18.39992786714538298 ) ) ;
#2407 = VECTOR ( 'NONE', #19625, 1000.000000000000000 ) ;
#2408 = EDGE_LOOP ( 'NONE', ( #16575, #6312, #23919, #7160 ) ) ;
#2409 = CARTESIAN_POINT ( 'NONE',  ( 18.38841581631819366, -7.866599884335185422, 7.652108011868850923 ) ) ;
#2410 = CARTESIAN_POINT ( 'NONE',  ( -23.21352257770656990, -10.78826658734919519, 45.15942333309109813 ) ) ;
#2411 = CARTESIAN_POINT ( 'NONE',  ( 11.85823002435686035, 12.27640118502220545, 18.64703902303423178 ) ) ;
#2412 = CARTESIAN_POINT ( 'NONE',  ( 15.57266529552201995, -38.96488032230103471, -1.500000000000000000 ) ) ;
#2413 = VERTEX_POINT ( 'NONE', #24395 ) ;
#2414 = AXIS2_PLACEMENT_3D ( 'NONE', #24888, #24716, #22392 ) ;
#2415 = CARTESIAN_POINT ( 'NONE',  ( 32.98805937973593672, 0.000000000000000000, 13.00000000000000178 ) ) ;
#2416 = CARTESIAN_POINT ( 'NONE',  ( 9.033033306777456417, -0.9621688436939739297, 13.22130136205108819 ) ) ;
#2417 = APPLICATION_CONTEXT ( 'automotive_design' ) ;
#2418 = CARTESIAN_POINT ( 'NONE',  ( -12.73056545648133131, 11.29944703097526748, 19.08155846658118904 ) ) ;
#2419 = CARTESIAN_POINT ( 'NONE',  ( -19.94274101607341976, 1.513210029880958984, 6.919864475265770309 ) ) ;
#2420 = CARTESIAN_POINT ( 'NONE',  ( 0.000000000000000000, 36.71644397333972165, 24.50000000000000000 ) ) ;
#2421 = DIRECTION ( 'NONE',  ( 0.000000000000000000, 0.000000000000000000, 1.000000000000000000 ) ) ;
#2422 = CARTESIAN_POINT ( 'NONE',  ( 17.79239818699415920, 14.89473990422378158, -1.500000000000000000 ) ) ;
#2423 = ADVANCED_FACE ( 'NONE', ( #686 ), #28623, .T. ) ;
#2424 = ORIENTED_EDGE ( 'NONE', *, *, #6315, .T. ) ;
#2425 = VERTEX_POINT ( 'NONE', #7566 ) ;
#2426 = CARTESIAN_POINT ( 'NONE',  ( 15.81223572262637589, -6.365019322297389870, 7.652108011868850923 ) ) ;
#2427 = EDGE_CURVE ( 'NONE', #25701, #23467, #2974, .T. ) ;
#2428 = CARTESIAN_POINT ( 'NONE',  ( -19.64114023396299302, -37.13592150529018454, -1.500000000000000000 ) ) ;
#2429 = CARTESIAN_POINT ( 'NONE',  ( -12.90456292687989759, 11.10871050118981529, 7.359006845440219102 ) ) ;
#2430 = DIRECTION ( 'NONE',  ( -0.000000000000000000, -0.000000000000000000, 1.000000000000000000 ) ) ;
#2431 = VERTEX_POINT ( 'NONE', #20025 ) ;
#2432 = CARTESIAN_POINT ( 'NONE',  ( 0.000000000000000000, 0.000000000000000000, 0.000000000000000000 ) ) ;
#2433 = CIRCLE ( 'NONE', #26264, 29.99999999999928946 ) ;
#2434 = CARTESIAN_POINT ( 'NONE',  ( 15.39534585122290267, -7.260971684546492000, 19.11611934778430921 ) ) ;
#2435 = AXIS2_PLACEMENT_3D ( 'NONE', #26630, #22244, #881 ) ;
#2436 = VECTOR ( 'NONE', #10712, 1000.000000000000000 ) ;
#2437 = DIRECTION ( 'NONE',  ( 0.000000000000000000, 1.132880637372608986E-16, -1.000000000000000000 ) ) ;
#2438 = ORIENTED_EDGE ( 'NONE', *, *, #30578, .F. ) ;
#2439 = CARTESIAN_POINT ( 'NONE',  ( 5.008980049945718882, 16.26773947435520284, 19.22654678686458141 ) ) ;
#2440 = CARTESIAN_POINT ( 'NONE',  ( -33.35889462893121049, -23.76060431981724363, -9.833271596736169684 ) ) ;
#2441 = AXIS2_PLACEMENT_3D ( 'NONE', #28161, #6956, #2111 ) ;
#2442 = LINE ( 'NONE', #11963, #7867 ) ;
#2443 = CARTESIAN_POINT ( 'NONE',  ( -31.96854311794286474, 24.49685236950227463, 34.62152949131530022 ) ) ;
#2444 = VERTEX_POINT ( 'NONE', #18011 ) ;
#2445 = CARTESIAN_POINT ( 'NONE',  ( 23.62400240902268322, 9.724154461249522541, 45.23564988763768469 ) ) ;
#2446 = B_SPLINE_CURVE_WITH_KNOTS ( 'NONE', 3,
 ( #5245, #24262, #12427, #21922 ),
 .UNSPECIFIED., .F., .F.,
 ( 4, 4 ),
 ( 2.143643656977390230E-07, 0.003421830178490235016 ),
 .UNSPECIFIED. ) ;
#2447 = LINE ( 'NONE', #11967, #11055 ) ;
#2448 = AXIS2_PLACEMENT_3D ( 'NONE', #30312, #20786, #16123 ) ;
#2449 = CARTESIAN_POINT ( 'NONE',  ( 49.99999999999998579, -70.00000000000000000, 59.49999999999999289 ) ) ;
#2450 = ORIENTED_EDGE ( 'NONE', *, *, #5383, .T. ) ;
#2451 = CARTESIAN_POINT ( 'NONE',  ( -15.21426671708081635, -7.679208962302483066, 7.652108011868850035 ) ) ;
#2452 = CARTESIAN_POINT ( 'NONE',  ( 14.32702845807335734, 13.95510847468387539, 6.037995405461177079 ) ) ;
#2453 = CARTESIAN_POINT ( 'NONE',  ( 8.616279238414451314, -7.781333699927420966, 1.500000000000000000 ) ) ;
#2454 = VECTOR ( 'NONE', #22694, 1000.000000000000000 ) ;
#2455 = DIRECTION ( 'NONE',  ( 0.000000000000000000, 1.000000000000000000, 0.000000000000000000 ) ) ;
#2456 = DIRECTION ( 'NONE',  ( -0.8932538319083086487, -0.4495526574063634095, 0.000000000000000000 ) ) ;
#2457 = CARTESIAN_POINT ( 'NONE',  ( -16.98316914218901275, 1.504314895146018127, 20.33971507717571114 ) ) ;
#2458 = CARTESIAN_POINT ( 'NONE',  ( -52.16608720827707657, 36.86186943028246787, 97.07879600563551037 ) ) ;
#2459 = ORIENTED_EDGE ( 'NONE', *, *, #2894, .T. ) ;
#2460 = CARTESIAN_POINT ( 'NONE',  ( 11.70583205457081988, -16.23839729645240126, 20.06253562465620632 ) ) ;
#2461 = AXIS2_PLACEMENT_3D ( 'NONE', #6539, #11067, #13262 ) ;
#2462 = CARTESIAN_POINT ( 'NONE',  ( 9.268856789657291984, 38.25380398711768493, 27.50000000000001066 ) ) ;
#2463 = ORIENTED_EDGE ( 'NONE', *, *, #23072, .T. ) ;
#2464 = ORIENTED_EDGE ( 'NONE', *, *, #29382, .F. ) ;
#2465 = CARTESIAN_POINT ( 'NONE',  ( 4.308942857043133401, 19.53031007734547941, 19.48477075383299706 ) ) ;
#2466 = CARTESIAN_POINT ( 'NONE',  ( -13.66184973646045542, 48.09774150583283614, -61.21269189572690550 ) ) ;
#2467 = CARTESIAN_POINT ( 'NONE',  ( -22.95669091611927826, 27.54300778121952220, -1.500000000000000000 ) ) ;
#2468 = EDGE_LOOP ( 'NONE', ( #9610, #11994, #13861, #1439 ) ) ;
#2469 = AXIS2_PLACEMENT_3D ( 'NONE', #13908, #18596, #16544 ) ;
#2470 = B_SPLINE_CURVE_WITH_KNOTS ( 'NONE', 3,
 ( #8363, #17879, #22679, #1334, #15830, #22993, #11007, #30030, #23304, #30472, #9114, #20658, #25810, #23447 ),
 .UNSPECIFIED., .F., .F.,
 ( 4, 2, 2, 2, 2, 2, 4 ),
 ( 2.111077618454142872E-07, 0.0004668847438969826258, 0.0009335583800321198365, 0.001400232016167257156, 0.001866905652302394258, 0.002800252924572680605, 0.003733600196842966519 ),
 .UNSPECIFIED. ) ;
#2471 = LINE ( 'NONE', #26482, #12697 ) ;
#2472 = CARTESIAN_POINT ( 'NONE',  ( -10.62374177707235035, -16.96647932868177122, 7.652108011868850035 ) ) ;
#2473 = VERTEX_POINT ( 'NONE', #29396 ) ;
#2474 = CARTESIAN_POINT ( 'NONE',  ( 16.06085112851923924, -5.768724642094689159, 18.56793045041961321 ) ) ;
#2475 = CARTESIAN_POINT ( 'NONE',  ( 19.61965483366450513, 3.971857776421114483, 19.97651184436794125 ) ) ;
#2476 = LINE ( 'NONE', #28981, #6020 ) ;
#2477 = ORIENTED_EDGE ( 'NONE', *, *, #27904, .T. ) ;
#2478 = CARTESIAN_POINT ( 'NONE',  ( 25.23756106473024019, 11.43858098102958287, -11.49999999999999645 ) ) ;
#2479 = ORIENTED_EDGE ( 'NONE', *, *, #16053, .F. ) ;
#2480 = AXIS2_PLACEMENT_3D ( 'NONE', #23136, #11458, #20941 ) ;
#2481 = ORIENTED_EDGE ( 'NONE', *, *, #12580, .F. ) ;
#2482 = DIRECTION ( 'NONE',  ( -0.000000000000000000, -0.000000000000000000, -1.000000000000000000 ) ) ;
#2483 = CARTESIAN_POINT ( 'NONE',  ( -17.81689967073718250, -9.086958408757460859, 5.779535427900762912 ) ) ;
#2484 = AXIS2_PLACEMENT_3D ( 'NONE', #7571, #28780, #26752 ) ;
#2485 = DIRECTION ( 'NONE',  ( -0.000000000000000000, -0.000000000000000000, 1.000000000000000000 ) ) ;
#2486 = CARTESIAN_POINT ( 'NONE',  ( -11.99928012101186958, -40.44431291024729092, 29.02086326041609254 ) ) ;
#2487 = CARTESIAN_POINT ( 'NONE',  ( 1.795426799894649594, -16.98366215210793584, 19.28454053338349183 ) ) ;
#2488 = CYLINDRICAL_SURFACE ( 'NONE', #20811, 1.447898107987198646 ) ;
#2489 = EDGE_CURVE ( 'NONE', #12801, #14860, #822, .T. ) ;
#2490 = ORIENTED_EDGE ( 'NONE', *, *, #12020, .F. ) ;
#2491 = CARTESIAN_POINT ( 'NONE',  ( -19.71077436674131533, 3.493128416889933252, 19.22654678686458141 ) ) ;
#2492 = CARTESIAN_POINT ( 'NONE',  ( 23.62400240902267967, -9.724154461249520764, 45.23564988763767758 ) ) ;
#2493 = CARTESIAN_POINT ( 'NONE',  ( -34.99999999999933920, 0.000000000000000000, 92.49999999999998579 ) ) ;
#2494 = ORIENTED_EDGE ( 'NONE', *, *, #376, .T. ) ;
#2495 = VERTEX_POINT ( 'NONE', #3654 ) ;
#2496 = CARTESIAN_POINT ( 'NONE',  ( -40.05520443301966083, -7.028746486913004077, -16.50000000000000000 ) ) ;
#2497 = CARTESIAN_POINT ( 'NONE',  ( 20.62927206985200712, -25.36120318786823802, -16.50001200000000523 ) ) ;
#2498 = EDGE_CURVE ( 'NONE', #28591, #119, #22243, .T. ) ;
#2499 = CARTESIAN_POINT ( 'NONE',  ( -4.163336342344337027E-14, 1.387778780781445676E-14, 52.50000000000000000 ) ) ;
#2500 = DIRECTION ( 'NONE',  ( 0.000000000000000000, -1.132880637372608986E-16, 1.000000000000000000 ) ) ;
#2501 = CARTESIAN_POINT ( 'NONE',  ( 11.65972768484890665, 12.47873923859707190, 6.783738457429052460 ) ) ;
#2503 = ADVANCED_FACE ( 'NONE', ( #10514 ), #6662, .T. ) ;
#2502 = AXIS2_PLACEMENT_3D ( 'NONE', #6433, #16235, #16093 ) ;
#2504 = CARTESIAN_POINT ( 'NONE',  ( -34.41394710506926202, -11.60896409125851036, 27.50000000000000355 ) ) ;
#2505 = CARTESIAN_POINT ( 'NONE',  ( -25.48568755041063838, 12.36160011285429583, 24.50000000000000000 ) ) ;
#2506 = EDGE_CURVE ( 'NONE', #8832, #12097, #26221, .T. ) ;
#2507 = VERTEX_POINT ( 'NONE', #2064 ) ;
#2508 = MANIFOLD_SOLID_BREP ( 'Cut-Extrude26', #11827 ) ;
#2509 = CARTESIAN_POINT ( 'NONE',  ( -18.27078283711139051, -34.03626749931920159, 34.50000000000000000 ) ) ;
#2510 = EDGE_CURVE ( 'NONE', #2413, #23760, #25104, .T. ) ;
#2511 = CARTESIAN_POINT ( 'NONE',  ( -18.04365185506139113, -8.627086862512678422, 20.34789198813115263 ) ) ;
#2512 = AXIS2_PLACEMENT_3D ( 'NONE', #27208, #29400, #8513 ) ;
#2513 = DIRECTION ( 'NONE',  ( -1.000000000000000000, 0.000000000000000000, 0.000000000000000000 ) ) ;
#2514 = ORIENTED_EDGE ( 'NONE', *, *, #24608, .F. ) ;
#2515 = EDGE_CURVE ( 'NONE', #24825, #14826, #23426, .T. ) ;
#2516 = CARTESIAN_POINT ( 'NONE',  ( 13.00882613046785607, 10.97723423515713215, 6.530762810602277924 ) ) ;
#2517 = VERTEX_POINT ( 'NONE', #21699 ) ;
#2518 = CARTESIAN_POINT ( 'NONE',  ( 18.72527277698615578, -7.076062192109023208, 6.892848776733236704 ) ) ;
#2519 = CYLINDRICAL_SURFACE ( 'NONE', #12031, 0.7499999999999997780 ) ;
#2520 = ORIENTED_EDGE ( 'NONE', *, *, #6743, .F. ) ;
#2521 = CARTESIAN_POINT ( 'NONE',  ( 31.51879050643202618, 19.12242388295294404, 27.49999999999999645 ) ) ;
#2522 = CARTESIAN_POINT ( 'NONE',  ( 0.000000000000000000, -2.435693370351110282E-15, 21.50000000000000355 ) ) ;
#2523 = CARTESIAN_POINT ( 'NONE',  ( 10.08077896146697761, -13.75650449133559405, 20.34789198813114908 ) ) ;
#2524 = DIRECTION ( 'NONE',  ( 0.000000000000000000, 0.000000000000000000, 1.000000000000000000 ) ) ;
#2525 = AXIS2_PLACEMENT_3D ( 'NONE', #23977, #2159, #9494 ) ;
#2526 = DIRECTION ( 'NONE',  ( -0.000000000000000000, -0.000000000000000000, 1.000000000000000000 ) ) ;
#2527 = CARTESIAN_POINT ( 'NONE',  ( -24.73258466867722660, -33.64422401626472237, -6.500000000000000888 ) ) ;
#2528 = DIRECTION ( 'NONE',  ( -0.000000000000000000, -0.000000000000000000, -1.000000000000000000 ) ) ;
#2529 = EDGE_CURVE ( 'NONE', #20718, #8541, #24039, .T. ) ;
#2530 = ORIENTED_EDGE ( 'NONE', *, *, #7260, .T. ) ;
#2531 = EDGE_CURVE ( 'NONE', #24218, #18940, #30664, .T. ) ;
#2532 = CARTESIAN_POINT ( 'NONE',  ( -2.687479363073305372, 44.39187623477332068, -19.50000000000000355 ) ) ;
#2533 = CARTESIAN_POINT ( 'NONE',  ( -7.827050521741844236, 5.352643706120543854, 1.500000000000001332 ) ) ;
#2534 = EDGE_CURVE ( 'NONE', #5487, #3669, #15769, .T. ) ;
#2535 = ORIENTED_EDGE ( 'NONE', *, *, #24634, .F. ) ;
#2536 = CARTESIAN_POINT ( 'NONE',  ( -3.221450758838616757, 1.621276839356792454, -1.500000000000000000 ) ) ;
#2537 = CARTESIAN_POINT ( 'NONE',  ( -15.16517292768934233, -7.781889190071453299, 20.34789198813115263 ) ) ;
#2538 = DIRECTION ( 'NONE',  ( 0.000000000000000000, 0.000000000000000000, 1.000000000000000000 ) ) ;
#2539 = EDGE_CURVE ( 'NONE', #6919, #11684, #5300, .T. ) ;
#2540 = CARTESIAN_POINT ( 'NONE',  ( 4.985742441154983773, 16.27537970825923352, 6.910395520694541993 ) ) ;
#2541 = CARTESIAN_POINT ( 'NONE',  ( -39.00000000000000000, -5.563236990218529243, -1.500000000000000000 ) ) ;
#2542 = EDGE_LOOP ( 'NONE', ( #9887, #6401 ) ) ;
#2543 = FACE_OUTER_BOUND ( 'NONE', #28543, .T. ) ;
#2544 = CARTESIAN_POINT ( 'NONE',  ( 37.44001822671184243, 11.96995332997097705, 31.77506326509126922 ) ) ;
#2545 = ADVANCED_FACE ( 'NONE', ( #12053 ), #9702, .F. ) ;
#2546 = CARTESIAN_POINT ( 'NONE',  ( -6.565451881449787308, 18.89189346177362694, 5.853797745100183469 ) ) ;
#2547 = VERTEX_POINT ( 'NONE', #19378 ) ;
#2548 = AXIS2_PLACEMENT_3D ( 'NONE', #29065, #5668, #12386 ) ;
#2549 = AXIS2_PLACEMENT_3D ( 'NONE', #12742, #10401, #25362 ) ;
#2550 = DIRECTION ( 'NONE',  ( 1.000000000000000000, -0.000000000000000000, -0.000000000000000000 ) ) ;
#2551 = VERTEX_POINT ( 'NONE', #11908 ) ;
#2552 = LINE ( 'NONE', #7843, #9206 ) ;
#2553 = CARTESIAN_POINT ( 'NONE',  ( -24.03057240117691862, -26.57182937991349903, -6.500000000000000888 ) ) ;
#2554 = EDGE_LOOP ( 'NONE', ( #25894, #27667, #22850, #11057, #23980, #17264 ) ) ;
#2555 = ORIENTED_EDGE ( 'NONE', *, *, #18538, .T. ) ;
#2556 = DIRECTION ( 'NONE',  ( 0.000000000000000000, 0.000000000000000000, -1.000000000000000000 ) ) ;
#2557 = EDGE_LOOP ( 'NONE', ( #20705, #9961, #8594, #30062 ) ) ;
#2558 = ORIENTED_EDGE ( 'NONE', *, *, #18946, .F. ) ;
#2559 = ORIENTED_EDGE ( 'NONE', *, *, #1389, .F. ) ;
#2560 = CARTESIAN_POINT ( 'NONE',  ( -0.09481216811183737492, -20.01790837231453324, 20.25336174263950184 ) ) ;
#2561 = EDGE_CURVE ( 'NONE', #10914, #19471, #2379, .T. ) ;
#2562 = CARTESIAN_POINT ( 'NONE',  ( -9.169883732660077058, -9.268939115642981008, 1.500000000000001332 ) ) ;
#2563 = ADVANCED_FACE ( 'NONE', ( #12523 ), #16885, .F. ) ;
#2564 = CARTESIAN_POINT ( 'NONE',  ( -24.44496207165490276, -7.595930209050158588, 45.15942333309111234 ) ) ;
#2565 = CARTESIAN_POINT ( 'NONE',  ( 0.6919288935074129343, -20.00608154967867947, 18.39992786714538298 ) ) ;
#2566 = ORIENTED_EDGE ( 'NONE', *, *, #21422, .T. ) ;
#2567 = CARTESIAN_POINT ( 'NONE',  ( -26.36764545593177544, -31.31467416275353344, -1.500000000000000000 ) ) ;
#2568 = CARTESIAN_POINT ( 'NONE',  ( -15.75094665830067697, -12.32508334119358828, 24.50000000000000000 ) ) ;
#2569 = CARTESIAN_POINT ( 'NONE',  ( 14.46722394715956916, 13.83532015011946292, 20.13759033520874908 ) ) ;
#2570 = CARTESIAN_POINT ( 'NONE',  ( -50.00000000000000000, -50.00000000000000000, 97.07879600563551037 ) ) ;
#2571 = VERTEX_POINT ( 'NONE', #18926 ) ;
#2572 = CIRCLE ( 'NONE', #1080, 1.000000000000008438 ) ;
#2573 = FACE_OUTER_BOUND ( 'NONE', #1606, .T. ) ;
#2574 = CARTESIAN_POINT ( 'NONE',  ( 37.99999999999999289, 80.00000000000000000, 50.49999999999998579 ) ) ;
#2575 = DIRECTION ( 'NONE',  ( 0.000000000000000000, 0.000000000000000000, 1.000000000000000000 ) ) ;
#2576 = DIRECTION ( 'NONE',  ( 0.000000000000000000, 0.000000000000000000, 1.000000000000000000 ) ) ;
#2577 = CARTESIAN_POINT ( 'NONE',  ( -40.00000000000002842, 80.00000000000001421, 22.49999999999983302 ) ) ;
#2578 = CARTESIAN_POINT ( 'NONE',  ( -15.39003174319561218, -7.295547530644703293, 18.49267272388512140 ) ) ;
#2579 = LINE ( 'NONE', #28156, #30018 ) ;
#2580 = ORIENTED_EDGE ( 'NONE', *, *, #22101, .T. ) ;
#2581 = ORIENTED_EDGE ( 'NONE', *, *, #17459, .F. ) ;
#2582 = DIRECTION ( 'NONE',  ( 1.000000000000000000, 0.000000000000000000, 0.000000000000000000 ) ) ;
#2583 = DIRECTION ( 'NONE',  ( 0.000000000000000000, 0.000000000000000000, -1.000000000000000000 ) ) ;
#2584 = DIRECTION ( 'NONE',  ( -1.000000000000000000, 0.000000000000000000, 0.000000000000000000 ) ) ;
#2586 = CARTESIAN_POINT ( 'NONE',  ( -27.03074382657074537, 6.449748410230984774, -16.55003854064094426 ) ) ;
#2585 = AXIS2_PLACEMENT_3D ( 'NONE', #25823, #4142, #25090 ) ;
#2587 = VERTEX_POINT ( 'NONE', #26556 ) ;
#2588 = CARTESIAN_POINT ( 'NONE',  ( 16.19472973927114268, -5.422090571236379830, 19.28454053338348473 ) ) ;
#2589 = CARTESIAN_POINT ( 'NONE',  ( 6.071284049926377158, 19.07508289763275400, 7.272049892295485485 ) ) ;
#2590 = ORIENTED_EDGE ( 'NONE', *, *, #25566, .F. ) ;
#2591 = CARTESIAN_POINT ( 'NONE',  ( 6.060672894209299777, 19.07852886212369370, 18.71435384576123440 ) ) ;
#2592 = CARTESIAN_POINT ( 'NONE',  ( 14.59923040764597779, 13.69601292063888920, 7.559636331181775581 ) ) ;
#2593 = VECTOR ( 'NONE', #21769, 1000.000000000000000 ) ;
#2594 = CARTESIAN_POINT ( 'NONE',  ( -22.43745300381736030, -36.72714324444464040, -16.50000000000000000 ) ) ;
#2595 = CARTESIAN_POINT ( 'NONE',  ( -37.69406220750976644, 10.98234033417770128, 31.84368292284955260 ) ) ;
#2596 = ORIENTED_EDGE ( 'NONE', *, *, #25773, .F. ) ;
#2597 = CARTESIAN_POINT ( 'NONE',  ( 0.000000000000000000, 1.699320956058915452E-16, -1.500000000000001776 ) ) ;
#2598 = CARTESIAN_POINT ( 'NONE',  ( 8.159193615868399974, -3.993622308618911099, 21.50000000000000000 ) ) ;
#2599 = CARTESIAN_POINT ( 'NONE',  ( 16.14703582738955490, 40.45263314063372206, -16.50000000000000711 ) ) ;
#2600 = ORIENTED_EDGE ( 'NONE', *, *, #27155, .F. ) ;
#2601 = CARTESIAN_POINT ( 'NONE',  ( -1.073881485057887497, 0.9711784013062738641, 1.500000000000000000 ) ) ;
#2602 = EDGE_CURVE ( 'NONE', #1033, #2495, #21218, .T. ) ;
#2603 = DIRECTION ( 'NONE',  ( 0.000000000000000000, 0.000000000000000000, -1.000000000000000000 ) ) ;
#2604 = LINE ( 'NONE', #2761, #2830 ) ;
#2605 = DIRECTION ( 'NONE',  ( 1.000000000000000000, 0.000000000000000000, 0.000000000000000000 ) ) ;
#2606 = CARTESIAN_POINT ( 'NONE',  ( 37.99999999999999289, 209.2686044187655909, -75.50000000000001421 ) ) ;
#2607 = DIRECTION ( 'NONE',  ( -1.000000000000000000, 0.000000000000000000, 0.000000000000000000 ) ) ;
#2608 = CARTESIAN_POINT ( 'NONE',  ( 36.63885979765411349, -14.57625097221031751, 16.42869143197607684 ) ) ;
#2609 = DIRECTION ( 'NONE',  ( 1.000000000000000000, 0.000000000000000000, 0.000000000000000000 ) ) ;
#2610 = ORIENTED_EDGE ( 'NONE', *, *, #5389, .T. ) ;
#2611 = CARTESIAN_POINT ( 'NONE',  ( -29.61203839202723032, 15.40012917324033204, 41.62281023987520001 ) ) ;
#2612 = DIRECTION ( 'NONE',  ( 0.000000000000000000, 0.000000000000000000, -1.000000000000000000 ) ) ;
#2613 = ORIENTED_EDGE ( 'NONE', *, *, #2747, .F. ) ;
#2614 = ORIENTED_EDGE ( 'NONE', *, *, #22128, .T. ) ;
#2615 = CARTESIAN_POINT ( 'NONE',  ( -50.00000000000000000, 70.00000000000000000, 52.49999999999999289 ) ) ;
#2616 = CARTESIAN_POINT ( 'NONE',  ( -1.976776171439267760, 49.97021316353860954, -40.09845666013538334 ) ) ;
#2617 = ORIENTED_EDGE ( 'NONE', *, *, #17280, .F. ) ;
#2618 = CARTESIAN_POINT ( 'NONE',  ( 17.22181377297005866, 14.41708049311048789, -1.500000000000000000 ) ) ;
#2619 = AXIS2_PLACEMENT_3D ( 'NONE', #23778, #2430, #11212 ) ;
#2620 = ORIENTED_EDGE ( 'NONE', *, *, #14985, .F. ) ;
#2621 = VECTOR ( 'NONE', #4644, 1000.000000000000000 ) ;
#2622 = CARTESIAN_POINT ( 'NONE',  ( 16.15906311113806382, -5.516254886378318290, 19.79423548914561692 ) ) ;
#2623 = CARTESIAN_POINT ( 'NONE',  ( 16.64821571380337772, 3.734651121118245154, 18.50655187082627862 ) ) ;
#2624 = CARTESIAN_POINT ( 'NONE',  ( -27.03074382657074537, 6.449748410230984774, 47.21042702067971675 ) ) ;
#2625 = ORIENTED_EDGE ( 'NONE', *, *, #17830, .F. ) ;
#2626 = CARTESIAN_POINT ( 'NONE',  ( 15.55638214359055205, -6.928938690483699148, 20.14907003336613656 ) ) ;
#2627 = VERTEX_POINT ( 'NONE', #26083 ) ;
#2628 = ADVANCED_FACE ( 'NONE', ( #5184 ), #7209, .F. ) ;
#2629 = EDGE_LOOP ( 'NONE', ( #21905, #1400, #4052, #5248 ) ) ;
#2630 = CARTESIAN_POINT ( 'NONE',  ( 32.06000616748023901, 24.34448380653289234, 30.63959652465332439 ) ) ;
#2631 = LINE ( 'NONE', #2790, #8152 ) ;
#2632 = CYLINDRICAL_SURFACE ( 'NONE', #30688, 0.7500000000000006661 ) ;
#2633 = B_SPLINE_CURVE_WITH_KNOTS ( 'NONE', 3,
 ( #2001, #18845, #19145, #9170, #13706, #18539, #28189, #6986, #16496, #26015, #11522, #21006, #30526, #28817, #14760, #24433 ),
 .UNSPECIFIED., .F., .F.,
 ( 4, 2, 2, 2, 2, 2, 2, 4 ),
 ( 0.5000000000000000000, 0.6250000000000001110, 0.6875000000000001110, 0.7187500000000002220, 0.7500000000000004441, 0.8125000000000002220, 0.8750000000000000000, 1.000000000000000000 ),
 .UNSPECIFIED. ) ;
#2634 = CARTESIAN_POINT ( 'NONE',  ( -20.51889442710595191, -36.16778909624833460, 29.42346760871654965 ) ) ;
#2635 = AXIS2_PLACEMENT_3D ( 'NONE', #25004, #29387, #3644 ) ;
#2636 = DIRECTION ( 'NONE',  ( -0.000000000000000000, -0.000000000000000000, 1.000000000000000000 ) ) ;
#2637 = CARTESIAN_POINT ( 'NONE',  ( 8.743977807160073112, 3.668292057956029861, 21.50000000000000000 ) ) ;
#2638 = ORIENTED_EDGE ( 'NONE', *, *, #21576, .T. ) ;
#2639 = AXIS2_PLACEMENT_3D ( 'NONE', #24872, #13169, #18314 ) ;
#2640 = CARTESIAN_POINT ( 'NONE',  ( -19.77235582619724497, 3.126546698941336189, 18.55820869691756769 ) ) ;
#2641 = DIRECTION ( 'NONE',  ( -0.000000000000000000, -1.000000000000000000, -0.000000000000000000 ) ) ;
#2642 = CARTESIAN_POINT ( 'NONE',  ( 37.99999999999999289, 90.00000000000001421, -69.50000000000000000 ) ) ;
#2643 = CARTESIAN_POINT ( 'NONE',  ( 31.56327786402390245, 10.34181101807379655, -16.55003854064094426 ) ) ;
#2644 = ORIENTED_EDGE ( 'NONE', *, *, #19672, .T. ) ;
#2645 = ORIENTED_EDGE ( 'NONE', *, *, #23070, .F. ) ;
#2646 = DIRECTION ( 'NONE',  ( -1.000000000000000000, 0.000000000000000000, 0.000000000000000000 ) ) ;
#2647 = AXIS2_PLACEMENT_3D ( 'NONE', #20182, #29706, #3977 ) ;
#2648 = DIRECTION ( 'NONE',  ( 1.000000000000000000, 0.000000000000000000, 0.000000000000000000 ) ) ;
#2649 = CARTESIAN_POINT ( 'NONE',  ( -6.543385983536391670, -6.301234758012574488, 21.50000000000000000 ) ) ;
#2650 = DIRECTION ( 'NONE',  ( -0.000000000000000000, -0.000000000000000000, -1.000000000000000000 ) ) ;
#2651 = DIRECTION ( 'NONE',  ( -0.7557495743542581579, -0.6548607339452852116, 0.000000000000000000 ) ) ;
#2652 = DIRECTION ( 'NONE',  ( -1.000000000000000000, 0.000000000000000000, 0.000000000000000000 ) ) ;
#2653 = ORIENTED_EDGE ( 'NONE', *, *, #27879, .F. ) ;
#2654 = MANIFOLD_SOLID_BREP ( 'Cut-Extrude13', #3869 ) ;
#2655 = VECTOR ( 'NONE', #25234, 1000.000000000000000 ) ;
#2656 = DIRECTION ( 'NONE',  ( -1.000000000000000000, 0.000000000000000000, 0.000000000000000000 ) ) ;
#2657 = CARTESIAN_POINT ( 'NONE',  ( 0.000000000000000000, 0.000000000000000000, 1.500000000000001332 ) ) ;
#2658 = EDGE_CURVE ( 'NONE', #16156, #16328, #1282, .T. ) ;
#2659 = CARTESIAN_POINT ( 'NONE',  ( -9.041888939645129852, 0.8750451464063455642, 21.50000000000000000 ) ) ;
#2660 = VERTEX_POINT ( 'NONE', #19530 ) ;
#2661 = CARTESIAN_POINT ( 'NONE',  ( -1.438332125858111432, 8.884323311075791096, 21.50000000000000000 ) ) ;
#2662 = AXIS2_PLACEMENT_3D ( 'NONE', #21189, #28233, #9363 ) ;
#2663 = ORIENTED_EDGE ( 'NONE', *, *, #13799, .F. ) ;
#2664 = CYLINDRICAL_SURFACE ( 'NONE', #18902, 32.50000000000000000 ) ;
#2665 = AXIS2_PLACEMENT_3D ( 'NONE', #19796, #19492, #7643 ) ;
#2666 = CARTESIAN_POINT ( 'NONE',  ( -0.8762659238204844048, -8.999114229549588728, -3.621320343559650379 ) ) ;
#2667 = CARTESIAN_POINT ( 'NONE',  ( -24.44496207165490276, 7.595930209050158588, -16.55003854064094426 ) ) ;
#2668 = ORIENTED_EDGE ( 'NONE', *, *, #18963, .F. ) ;
#2669 = CARTESIAN_POINT ( 'NONE',  ( 47.14142842854284510, 69.79466010243311302, 59.49999999999998579 ) ) ;
#2670 = EDGE_CURVE ( 'NONE', #477, #1863, #17345, .T. ) ;
#2671 = DIRECTION ( 'NONE',  ( 1.000000000000000000, 0.000000000000000000, 0.000000000000000000 ) ) ;
#2672 = ORIENTED_EDGE ( 'NONE', *, *, #5239, .T. ) ;
#2673 = CARTESIAN_POINT ( 'NONE',  ( 0.000000000000000000, -1.502314598737157848E-15, -9.000000000000001776 ) ) ;
#2674 = CARTESIAN_POINT ( 'NONE',  ( -9.169883732660077058, -9.268939115642981008, 24.50000000000000000 ) ) ;
#2675 = CARTESIAN_POINT ( 'NONE',  ( 0.3518703668723784928, -19.99690444156084723, 20.34789198813115263 ) ) ;
#2676 = ORIENTED_EDGE ( 'NONE', *, *, #19295, .F. ) ;
#2677 = CARTESIAN_POINT ( 'NONE',  ( 15.60425753239542956, -6.827323759751870114, 7.526951045817046548 ) ) ;
#2678 = EDGE_CURVE ( 'NONE', #1559, #5756, #14256, .T. ) ;
#2679 = CARTESIAN_POINT ( 'NONE',  ( -37.98493438988125348, -11.12428508575252728, -1.500000000000000000 ) ) ;
#2680 = CARTESIAN_POINT ( 'NONE',  ( -3.668292057955944152, 8.743977807160112192, 1.500000000000001332 ) ) ;
#2681 = EDGE_LOOP ( 'NONE', ( #7169, #22145, #23971, #18570 ) ) ;
#2682 = DIRECTION ( 'NONE',  ( -0.000000000000000000, -0.000000000000000000, -1.000000000000000000 ) ) ;
#2683 = EDGE_CURVE ( 'NONE', #27986, #27603, #13292, .T. ) ;
#2684 = AXIS2_PLACEMENT_3D ( 'NONE', #4117, #13647, #4419 ) ;
#2685 = CARTESIAN_POINT ( 'NONE',  ( 49.99999999999998579, 50.00000000000000000, 52.07879600563550326 ) ) ;
#2686 = CARTESIAN_POINT ( 'NONE',  ( -6.587096388939656322, -18.88412458026101248, 24.50000000000000000 ) ) ;
#2687 = CIRCLE ( 'NONE', #23024, 0.7499999999999997780 ) ;
#2688 = AXIS2_PLACEMENT_3D ( 'NONE', #14981, #7816, #8133 ) ;
#2689 = CARTESIAN_POINT ( 'NONE',  ( 4.049916833591940879, 16.55712665779027049, 7.652108011868850923 ) ) ;
#2690 = CARTESIAN_POINT ( 'NONE',  ( 34.07766914600081520, 21.40380666527109810, -1.500000000000000000 ) ) ;
#2691 = CARTESIAN_POINT ( 'NONE',  ( 8.840471615930072247, -1.687027447297460236, -1.500000000000001776 ) ) ;
#2692 = CARTESIAN_POINT ( 'NONE',  ( 37.14755456718950910, 5.754233978929971904, 37.49999999992148503 ) ) ;
#2693 = DIRECTION ( 'NONE',  ( 0.1423148382732746797, -0.9898214418809342385, 0.000000000000000000 ) ) ;
#2694 = ORIENTED_EDGE ( 'NONE', *, *, #22140, .F. ) ;
#2695 = LINE ( 'NONE', #14693, #30620 ) ;
#2696 = ORIENTED_EDGE ( 'NONE', *, *, #29078, .T. ) ;
#2697 = DIRECTION ( 'NONE',  ( -0.000000000000000000, 0.000000000000000000, 1.000000000000000000 ) ) ;
#2698 = CYLINDRICAL_SURFACE ( 'NONE', #27387, 3.559164065751841743 ) ;
#2699 = ORIENTED_EDGE ( 'NONE', *, *, #23180, .F. ) ;
#2700 = EDGE_CURVE ( 'NONE', #8580, #3764, #11300, .T. ) ;
#2701 = VERTEX_POINT ( 'NONE', #22173 ) ;
#2702 = ADVANCED_FACE ( 'NONE', ( #13295, #17657 ), #10167, .T. ) ;
#2703 = LINE ( 'NONE', #19225, #6778 ) ;
#2704 = ORIENTED_EDGE ( 'NONE', *, *, #23249, .T. ) ;
#2705 = PRODUCT_DEFINITION_SHAPE ( 'NONE', 'NONE',  #30872 ) ;
#2706 = EDGE_CURVE ( 'NONE', #19691, #14477, #14997, .T. ) ;
#2707 = ORIENTED_EDGE ( 'NONE', *, *, #10964, .F. ) ;
#2708 = ORIENTED_EDGE ( 'NONE', *, *, #16097, .T. ) ;
#2709 = CARTESIAN_POINT ( 'NONE',  ( -24.50428919468314959, -7.442132857256927636, 45.14840622132437886 ) ) ;
#2710 = CIRCLE ( 'NONE', #10186, 2.061368542273053883 ) ;
#2711 = EDGE_CURVE ( 'NONE', #23725, #7065, #19746, .T. ) ;
#2712 = CARTESIAN_POINT ( 'NONE',  ( 0.000000000000000000, 0.000000000000000000, 1.500000000000001332 ) ) ;
#2713 = EDGE_CURVE ( 'NONE', #26988, #12630, #8473, .T. ) ;
#2714 = CARTESIAN_POINT ( 'NONE',  ( -8.079801766074020009, -15.02755831366981099, 5.810767894563978686 ) ) ;
#2715 = CARTESIAN_POINT ( 'NONE',  ( 4.894722408918116940, 16.30505022503850299, 19.85270094495842130 ) ) ;
#2716 = CARTESIAN_POINT ( 'NONE',  ( 0.8008512464130190800, -20.00192252186467812, 18.44527579819791185 ) ) ;
#2717 = ORIENTED_EDGE ( 'NONE', *, *, #29979, .T. ) ;
#2718 = ADVANCED_FACE ( 'NONE', ( #3155 ), #29514, .F. ) ;
#2719 = DIRECTION ( 'NONE',  ( -0.000000000000000000, -0.000000000000000000, -1.000000000000000000 ) ) ;
#2720 = DIRECTION ( 'NONE',  ( -0.000000000000000000, -0.000000000000000000, 1.000000000000000000 ) ) ;
#2721 = CARTESIAN_POINT ( 'NONE',  ( 24.03057240117691862, 26.57182937991349903, -6.500000000000000888 ) ) ;
#2722 = CARTESIAN_POINT ( 'NONE',  ( 12.20325286834225054, 11.91007939804258164, 18.37415474056476938 ) ) ;
#2723 = DIRECTION ( 'NONE',  ( 0.000000000000000000, 0.000000000000000000, 1.000000000000000000 ) ) ;
#2724 = EDGE_CURVE ( 'NONE', #2309, #20990, #15232, .T. ) ;
#2725 = ORIENTED_EDGE ( 'NONE', *, *, #6905, .F. ) ;
#2726 = CYLINDRICAL_SURFACE ( 'NONE', #25269, 0.7500000000000006661 ) ;
#2727 = DIRECTION ( 'NONE',  ( 0.000000000000000000, 0.000000000000000000, -1.000000000000000000 ) ) ;
#2728 = CARTESIAN_POINT ( 'NONE',  ( -5.978582532085230383, 19.10413086404602723, 5.652196082364320695 ) ) ;
#2729 = ADVANCED_FACE ( 'NONE', ( #3302 ), #29195, .T. ) ;
#2730 = CARTESIAN_POINT ( 'NONE',  ( -19.93487782419341059, 1.613472484145544117, 6.149077423860693337 ) ) ;
#2731 = DIRECTION ( 'NONE',  ( -1.000000000000000000, 0.000000000000000000, 0.000000000000000000 ) ) ;
#2732 = DIRECTION ( 'NONE',  ( 1.000000000000000000, 0.000000000000000000, 0.000000000000000000 ) ) ;
#2733 = CARTESIAN_POINT ( 'NONE',  ( -32.60829997825918980, -13.18983524832147936, 35.60092001944732232 ) ) ;
#2734 = EDGE_LOOP ( 'NONE', ( #21039, #4845, #11777, #25394 ) ) ;
#2735 = ORIENTED_EDGE ( 'NONE', *, *, #27082, .T. ) ;
#2736 = CARTESIAN_POINT ( 'NONE',  ( -11.82521593960875528, 5.400395169024524655, 1.500000000000001332 ) ) ;
#2737 = CIRCLE ( 'NONE', #21140, 9.084132297865673777 ) ;
#2738 = FACE_OUTER_BOUND ( 'NONE', #21954, .T. ) ;
#2739 = CARTESIAN_POINT ( 'NONE',  ( -13.02230393242516371, 10.97666050933785975, 7.500898271101006820 ) ) ;
#2740 = CARTESIAN_POINT ( 'NONE',  ( 11.52514311384751089, -16.34582042812247238, 20.22386025856690139 ) ) ;
#2741 = ORIENTED_EDGE ( 'NONE', *, *, #12392, .F. ) ;
#2742 = DIRECTION ( 'NONE',  ( 1.000000000000000000, 0.000000000000000000, 0.000000000000000000 ) ) ;
#2743 = FACE_BOUND ( 'NONE', #20323, .T. ) ;
#2744 = FACE_OUTER_BOUND ( 'NONE', #10004, .T. ) ;
#2745 = ADVANCED_FACE ( 'NONE', ( #15301 ), #3467, .F. ) ;
#2746 = ORIENTED_EDGE ( 'NONE', *, *, #29772, .T. ) ;
#2747 = EDGE_CURVE ( 'NONE', #1188, #20273, #17259, .T. ) ;
#2748 = CARTESIAN_POINT ( 'NONE',  ( 12.30878326772641884, 11.79452912058117775, 7.652108011868850035 ) ) ;
#2749 = CARTESIAN_POINT ( 'NONE',  ( 6.632267977001171655E-15, -7.573738413550481496, 4.881900264494505315 ) ) ;
#2750 = EDGE_CURVE ( 'NONE', #28599, #15594, #13606, .T. ) ;
#2751 = CARTESIAN_POINT ( 'NONE',  ( -26.39612953643615256, 31.29397724899363809, 29.91504862403774467 ) ) ;
#2752 = ORIENTED_EDGE ( 'NONE', *, *, #25397, .F. ) ;
#2753 = CARTESIAN_POINT ( 'NONE',  ( -29.61203839202723032, -15.40012917324033381, 41.62281023987518580 ) ) ;
#2754 = ADVANCED_FACE ( 'NONE', ( #1595 ), #8922, .F. ) ;
#2755 = LINE ( 'NONE', #12267, #2593 ) ;
#2756 = CARTESIAN_POINT ( 'NONE',  ( 18.46022885586396356, 39.25482954210340125, -16.49999999999999645 ) ) ;
#2757 = ORIENTED_EDGE ( 'NONE', *, *, #10591, .F. ) ;
#2758 = CARTESIAN_POINT ( 'NONE',  ( -15.39438215884103656, -7.285634741961049876, 7.500898271101006820 ) ) ;
#2759 = CIRCLE ( 'NONE', #12737, 0.7500000000000006661 ) ;
#2760 = FACE_OUTER_BOUND ( 'NONE', #14871, .T. ) ;
#2761 = CARTESIAN_POINT ( 'NONE',  ( 26.31795596221988376, 10.51822134874671022, 1.500000000000000000 ) ) ;
#2762 = DIRECTION ( 'NONE',  ( 0.000000000000000000, 0.000000000000000000, 1.000000000000000000 ) ) ;
#2763 = LINE ( 'NONE', #7914, #10783 ) ;
#2764 = CARTESIAN_POINT ( 'NONE',  ( -9.041888939645131629, 0.8750451464063454532, -1.500000000000001776 ) ) ;
#2765 = CARTESIAN_POINT ( 'NONE',  ( 37.87340355726868779, -10.14209321046124934, 14.07067178332522239 ) ) ;
#2766 = DIRECTION ( 'NONE',  ( -0.000000000000000000, -0.000000000000000000, -1.000000000000000000 ) ) ;
#2767 = ORIENTED_EDGE ( 'NONE', *, *, #20964, .T. ) ;
#2768 = MANIFOLD_SOLID_BREP ( 'Boss-Extrude1', #19793 ) ;
#2769 = DIRECTION ( 'NONE',  ( -1.000000000000000000, 0.000000000000000000, 0.000000000000000000 ) ) ;
#2770 = CARTESIAN_POINT ( 'NONE',  ( 5.291489565152560637, 19.28730510418394317, 5.652196082369965069 ) ) ;
#2771 = ORIENTED_EDGE ( 'NONE', *, *, #19128, .T. ) ;
#2772 = VERTEX_POINT ( 'NONE', #18122 ) ;
#2773 = CARTESIAN_POINT ( 'NONE',  ( -4.163336342344337027E-14, -1.387778780781445676E-14, 1.500000000000000000 ) ) ;
#2774 = EDGE_CURVE ( 'NONE', #15471, #8734, #18703, .T. ) ;
#2775 = CARTESIAN_POINT ( 'NONE',  ( -9.910680102653831369, 49.01306433446774946, -66.30206827149085314 ) ) ;
#2776 = ORIENTED_EDGE ( 'NONE', *, *, #7868, .F. ) ;
#2777 = EDGE_CURVE ( 'NONE', #16205, #30019, #23085, .T. ) ;
#2778 = CARTESIAN_POINT ( 'NONE',  ( 0.000000000000000000, -1.502314598737157848E-15, -9.000000000000001776 ) ) ;
#2779 = CARTESIAN_POINT ( 'NONE',  ( -10.71492722147446131, -16.90904491356049988, 5.670038381137163519 ) ) ;
#2780 = ORIENTED_EDGE ( 'NONE', *, *, #26439, .F. ) ;
#2781 = CARTESIAN_POINT ( 'NONE',  ( 16.02447511960549775, -5.858916503155148447, 18.50655187082627862 ) ) ;
#2782 = CARTESIAN_POINT ( 'NONE',  ( 19.57334175050933567, 4.193940174973931789, 19.36813350477385143 ) ) ;
#2783 = AXIS2_PLACEMENT_3D ( 'NONE', #10452, #24794, #3433 ) ;
#2784 = CARTESIAN_POINT ( 'NONE',  ( 39.99999999999998579, 90.00000000000001421, 52.49999999999999289 ) ) ;
#2785 = EDGE_LOOP ( 'NONE', ( #7545, #15397, #16742, #26570, #2825, #18043, #18666, #5261, #18183, #2212, #30049, #12946, #28144, #12594, #5941, #25114, #642, #26416, #14017, #22966, #13161, #25380, #8556, #5844, #30157, #15989, #2771, #29412, #264, #5315, #3402, #11302, #8012, #16424, #13465, #17720, #23164, #4953, #14913, #11508, #1543, #13383, #11078, #21358, #19015, #1706, #9184, #29602, #23286, #3211, #26176, #13722, #29710, #23357, #17012, #7602, #1472, #9361, #9914, #29202, #28662, #2303, #8298, #4741, #19269, #28525, #18303, #16905, #28327, #15076, #15954, #1237, #3116, #19448, #25267, #27921, #15400, #13152, #23373, #15189, #4461, #15161, #21555, #3551, #12990, #5832, #27207, #10991, #30658, #6470, #21210, #24368, #13252 ) ) ;
#2786 = FACE_OUTER_BOUND ( 'NONE', #9152, .T. ) ;
#2787 = VERTEX_POINT ( 'NONE', #26971 ) ;
#2788 = EDGE_LOOP ( 'NONE', ( #2617, #20175, #12784, #1406 ) ) ;
#2789 = CARTESIAN_POINT ( 'NONE',  ( -6.934698339095106689, 18.77804097180239751, 19.47783254395485031 ) ) ;
#2790 = CARTESIAN_POINT ( 'NONE',  ( 0.000000000000000000, 80.00000000000000000, 50.49999999999998579 ) ) ;
#2791 = CARTESIAN_POINT ( 'NONE',  ( -19.54426622602688468, 37.07991288358297055, 1.499999999999999778 ) ) ;
#2792 = CIRCLE ( 'NONE', #4278, 50.00000000000000000 ) ;
#2793 = PLANE ( 'NONE',  #12044 ) ;
#2794 = DIRECTION ( 'NONE',  ( -1.000000000000000000, 0.000000000000000000, 0.000000000000000000 ) ) ;
#2795 = DIRECTION ( 'NONE',  ( 1.000000000000000000, 0.000000000000000000, 0.000000000000000000 ) ) ;
#2796 = EDGE_LOOP ( 'NONE', ( #17529, #23908, #24244, #26508 ) ) ;
#2797 = CARTESIAN_POINT ( 'NONE',  ( 9.007065134480614077, -14.44288896217592821, 6.755862304746362845 ) ) ;
#2798 = CARTESIAN_POINT ( 'NONE',  ( -30.18521284010790851, 26.91230962269908034, 8.856508891382476989 ) ) ;
#2799 = VECTOR ( 'NONE', #4047, 1000.000000000000000 ) ;
#2800 = CARTESIAN_POINT ( 'NONE',  ( 2.703030265324084080, -12.75514121382991384, 1.500000000000001332 ) ) ;
#2801 = ORIENTED_EDGE ( 'NONE', *, *, #7673, .F. ) ;
#2802 = ORIENTED_EDGE ( 'NONE', *, *, #2700, .T. ) ;
#2803 = CYLINDRICAL_SURFACE ( 'NONE', #1387, 0.7499999999999988898 ) ;
#2804 = CARTESIAN_POINT ( 'NONE',  ( -8.637616862297813114, 3.912171961292039590, 21.50000000000000000 ) ) ;
#2805 = DIRECTION ( 'NONE',  ( 0.000000000000000000, 0.000000000000000000, -1.000000000000000000 ) ) ;
#2806 = DIRECTION ( 'NONE',  ( 1.000000000000000000, 0.000000000000000000, 0.000000000000000000 ) ) ;
#2807 = AXIS2_PLACEMENT_3D ( 'NONE', #3105, #743, #29145 ) ;
#2808 = AXIS2_PLACEMENT_3D ( 'NONE', #12680, #24831, #10481 ) ;
#2809 = DIRECTION ( 'NONE',  ( -0.000000000000000000, -0.000000000000000000, 1.000000000000000000 ) ) ;
#2810 = VERTEX_POINT ( 'NONE', #10580 ) ;
#2811 = MANIFOLD_SOLID_BREP ( 'Cut-Extrude25', #25765 ) ;
#2812 = ORIENTED_EDGE ( 'NONE', *, *, #4404, .T. ) ;
#2813 = CARTESIAN_POINT ( 'NONE',  ( -27.19745787981435825, -25.87981526613175021, 34.49999999999998579 ) ) ;
#2814 = CARTESIAN_POINT ( 'NONE',  ( -17.81689967073718961, -9.086958408757471517, 18.47531940416305929 ) ) ;
#2815 = CARTESIAN_POINT ( 'NONE',  ( 5.204170427930421283E-15, -44.07656352898514740, -16.50000000000000000 ) ) ;
#2816 = ORIENTED_EDGE ( 'NONE', *, *, #20210, .T. ) ;
#2817 = AXIS2_PLACEMENT_3D ( 'NONE', #30042, #10704, #17717 ) ;
#2818 = CARTESIAN_POINT ( 'NONE',  ( 12.77540468287706155, 11.25967455357098856, 7.429667576816606278 ) ) ;
#2819 = ORIENTED_EDGE ( 'NONE', *, *, #4616, .T. ) ;
#2820 = FACE_BOUND ( 'NONE', #5046, .T. ) ;
#2821 = AXIS2_PLACEMENT_3D ( 'NONE', #13960, #27697, #20956 ) ;
#2822 = CARTESIAN_POINT ( 'NONE',  ( 16.70106355290392486, 3.455140589318408395, 20.34789198813114197 ) ) ;
#2823 = AXIS2_PLACEMENT_3D ( 'NONE', #19081, #25384, #23019 ) ;
#2824 = FACE_OUTER_BOUND ( 'NONE', #13856, .T. ) ;
#2825 = ORIENTED_EDGE ( 'NONE', *, *, #4464, .T. ) ;
#2826 = FACE_OUTER_BOUND ( 'NONE', #17698, .T. ) ;
#2827 = CARTESIAN_POINT ( 'NONE',  ( -24.03057240117691862, 26.57182937991348481, -1.500000000000001332 ) ) ;
#2828 = FACE_OUTER_BOUND ( 'NONE', #10800, .T. ) ;
#2829 = AXIS2_PLACEMENT_3D ( 'NONE', #27971, #11280, #16257 ) ;
#2830 = VECTOR ( 'NONE', #4942, 1000.000000000000000 ) ;
#2831 = FACE_OUTER_BOUND ( 'NONE', #19525, .T. ) ;
#2832 = ORIENTED_EDGE ( 'NONE', *, *, #5159, .T. ) ;
#2833 = CARTESIAN_POINT ( 'NONE',  ( 25.41654339919795902, 6.509636863629522097, 48.76343458312116041 ) ) ;
#2834 = DIRECTION ( 'NONE',  ( -0.000000000000000000, -0.000000000000000000, -1.000000000000000000 ) ) ;
#2835 = CIRCLE ( 'NONE', #10815, 50.00000000000000000 ) ;
#2836 = CARTESIAN_POINT ( 'NONE',  ( -13.22505861668184046, -42.10773672057003125, -19.50000000000000355 ) ) ;
#2837 = CARTESIAN_POINT ( 'NONE',  ( 40.05520497557499482, 7.028746409576331011, -16.50000000000000000 ) ) ;
#2838 = VERTEX_POINT ( 'NONE', #10894 ) ;
#2839 = CARTESIAN_POINT ( 'NONE',  ( -17.59891439103366295, -9.538503746949027473, 19.36813350477385143 ) ) ;
#2840 = CARTESIAN_POINT ( 'NONE',  ( 0.000000000000000000, 0.000000000000000000, 1.500000000000001332 ) ) ;
#2841 = AXIS2_PLACEMENT_3D ( 'NONE', #29655, #26695, #8292 ) ;
#2842 = CARTESIAN_POINT ( 'NONE',  ( -15.00000000000004086, 1.571475800653548713E-14, 77.49999999999998579 ) ) ;
#2843 = CARTESIAN_POINT ( 'NONE',  ( -1.073881485057738949, -0.9711784013061123266, -1.500000000000000000 ) ) ;
#2844 = CARTESIAN_POINT ( 'NONE',  ( -39.83602371821034183, 11.57901747687032490, -19.50000000000000355 ) ) ;
#2845 = DIRECTION ( 'NONE',  ( 0.000000000000000000, -1.132880637372608986E-16, 1.000000000000000000 ) ) ;
#2846 = EDGE_CURVE ( 'NONE', #25535, #4436, #15712, .T. ) ;
#2847 = CARTESIAN_POINT ( 'NONE',  ( 38.96845262021057010, 1.827616164893528961, 32.22212046549758924 ) ) ;
#2848 = EDGE_CURVE ( 'NONE', #24160, #16362, #1227, .T. ) ;
#2849 = DIRECTION ( 'NONE',  ( -1.000000000000000000, 0.000000000000000000, 0.000000000000000000 ) ) ;
#2850 = ORIENTED_EDGE ( 'NONE', *, *, #13038, .F. ) ;
#2851 = DIRECTION ( 'NONE',  ( 0.000000000000000000, 0.000000000000000000, 1.000000000000000000 ) ) ;
#2852 = VERTEX_POINT ( 'NONE', #25230 ) ;
#2853 = AXIS2_PLACEMENT_3D ( 'NONE', #12741, #29431, #29274 ) ;
#2854 = DIRECTION ( 'NONE',  ( -0.000000000000000000, -0.000000000000000000, -1.000000000000000000 ) ) ;
#2855 = LINE ( 'NONE', #5194, #24404 ) ;
#2856 = ORIENTED_EDGE ( 'NONE', *, *, #15096, .T. ) ;
#2857 = VERTEX_POINT ( 'NONE', #6209 ) ;
#2858 = AXIS2_PLACEMENT_3D ( 'NONE', #17489, #27011, #324 ) ;
#2859 = CARTESIAN_POINT ( 'NONE',  ( -37.99999999999999289, 70.00000000000000000, -22.50000000000001421 ) ) ;
#2860 = AXIS2_PLACEMENT_3D ( 'NONE', #5277, #28834, #7311 ) ;
#2861 = EDGE_LOOP ( 'NONE', ( #28394, #10437, #4508, #19072 ) ) ;
#2862 = ORIENTED_EDGE ( 'NONE', *, *, #24030, .F. ) ;
#2863 = CARTESIAN_POINT ( 'NONE',  ( 0.06889080212830860084, -17.02733034922398758, 18.63641924841378028 ) ) ;
#2864 = CARTESIAN_POINT ( 'NONE',  ( -8.026378865559991027, 38.50914575096116010, 34.49999999999998579 ) ) ;
#2865 = CARTESIAN_POINT ( 'NONE',  ( 0.000000000000000000, -8.043452525345523162E-15, -16.50000000000000000 ) ) ;
#2866 = FACE_OUTER_BOUND ( 'NONE', #24748, .T. ) ;
#2867 = CARTESIAN_POINT ( 'NONE',  ( -23.20738078402527549, 23.09073189384302793, -16.50001200000000168 ) ) ;
#2868 = ORIENTED_EDGE ( 'NONE', *, *, #15299, .T. ) ;
#2869 = CARTESIAN_POINT ( 'NONE',  ( -40.00000000000002842, 80.00000000000001421, 22.49999999999983302 ) ) ;
#2870 = CARTESIAN_POINT ( 'NONE',  ( 11.46038621610576236, -42.28394141292588415, -16.50000000000000000 ) ) ;
#2871 = CARTESIAN_POINT ( 'NONE',  ( 14.74216733233971866, 13.54174064842195691, 18.37415474056476938 ) ) ;
#2872 = FACE_BOUND ( 'NONE', #7887, .T. ) ;
#2873 = CIRCLE ( 'NONE', #22303, 7.500000000000013323 ) ;
#2874 = ORIENTED_EDGE ( 'NONE', *, *, #26738, .F. ) ;
#2875 = VECTOR ( 'NONE', #15795, 1000.000000000000000 ) ;
#2876 = CIRCLE ( 'NONE', #20316, 3.000000000000002665 ) ;
#2877 = CARTESIAN_POINT ( 'NONE',  ( -42.49999999999998579, 50.00000000000000000, 12.49999999999999112 ) ) ;
#2878 = CARTESIAN_POINT ( 'NONE',  ( -5.069257791428325888, 7.538175180318473778, 21.50000000000000000 ) ) ;
#2879 = CARTESIAN_POINT ( 'NONE',  ( -6.656778417335411646, 18.87854210339738970, 7.366751648393900176 ) ) ;
#2880 = LINE ( 'NONE', #12404, #29231 ) ;
#2881 = CARTESIAN_POINT ( 'NONE',  ( -8.413215745754975217, 3.196529495465474380, 1.500000000000001332 ) ) ;
#2882 = EDGE_CURVE ( 'NONE', #28303, #23905, #15716, .T. ) ;
#2883 = ADVANCED_FACE ( 'NONE', ( #1536 ), #27117, .T. ) ;
#2884 = B_SPLINE_CURVE_WITH_KNOTS ( 'NONE', 3,
 ( #25506, #3824, #27686, #13349, #16136, #4129, #25653, #4270, #13798, #23299, #2709, #19085 ),
 .UNSPECIFIED., .F., .F.,
 ( 4, 2, 2, 2, 2, 4 ),
 ( 2.975219550372212526E-07, 0.0009689891316535818779, 0.001937680741352126390, 0.002906372351050671120, 0.003390718155899948363, 0.003875063960749225173 ),
 .UNSPECIFIED. ) ;
#2885 = CARTESIAN_POINT ( 'NONE',  ( -18.15569024355516703, -8.431866758338669499, 18.36582235739946611 ) ) ;
#2886 = CARTESIAN_POINT ( 'NONE',  ( 15.57266529552203416, 38.96488032230103471, 1.500000000000000000 ) ) ;
#2887 = AXIS2_PLACEMENT_3D ( 'NONE', #100, #12263, #26458 ) ;
#2888 = EDGE_LOOP ( 'NONE', ( #25502, #20285, #18915 ) ) ;
#2889 = ORIENTED_EDGE ( 'NONE', *, *, #11376, .T. ) ;
#2890 = CARTESIAN_POINT ( 'NONE',  ( 29.61203839202723032, 15.40012917324034092, 37.38016955275583797 ) ) ;
#2891 = EDGE_CURVE ( 'NONE', #25287, #18178, #3562, .T. ) ;
#2892 = CARTESIAN_POINT ( 'NONE',  ( -11.46182693247433804, -1.387778780781445676E-14, 1.500000000000000000 ) ) ;
#2893 = CARTESIAN_POINT ( 'NONE',  ( -12.81275022540756581, 11.20978530020977004, 7.176035686813569292 ) ) ;
#2894 = EDGE_CURVE ( 'NONE', #27397, #4887, #20563, .T. ) ;
#2895 = CARTESIAN_POINT ( 'NONE',  ( 13.00999358272542850, -0.8602714556717643291, 24.50000000000000000 ) ) ;
#2896 = ORIENTED_EDGE ( 'NONE', *, *, #7446, .T. ) ;
#2897 = SHAPE_DEFINITION_REPRESENTATION ( #11653, #23229 ) ;
#2898 = FACE_BOUND ( 'NONE', #13547, .T. ) ;
#2899 = CARTESIAN_POINT ( 'NONE',  ( 4.082218581380957723, 16.54825969530613961, 5.651989602109218858 ) ) ;
#2900 = VECTOR ( 'NONE', #14038, 1000.000000000000114 ) ;
#2901 = EDGE_CURVE ( 'NONE', #4862, #27728, #17918, .T. ) ;
#2902 = ORIENTED_EDGE ( 'NONE', *, *, #8502, .F. ) ;
#2903 = CARTESIAN_POINT ( 'NONE',  ( 4.731053074881896414, 16.35701261131971407, 18.63641924841378028 ) ) ;
#2904 = CIRCLE ( 'NONE', #400, 9.482273699623480212 ) ;
#2905 = CARTESIAN_POINT ( 'NONE',  ( -8.752572334588103686, 2.431858781452820306, 21.50000000000000000 ) ) ;
#2906 = ADVANCED_FACE ( 'NONE', ( #15089 ), #21142, .F. ) ;
#2907 = VECTOR ( 'NONE', #22583, 1000.000000000000000 ) ;
#2908 = CYLINDRICAL_SURFACE ( 'NONE', #25297, 7.500000000000013323 ) ;
#2909 = CARTESIAN_POINT ( 'NONE',  ( -39.06789089969338846, -0.5117148525053366592, 32.25338167081577012 ) ) ;
#2910 = ORIENTED_EDGE ( 'NONE', *, *, #3708, .T. ) ;
#2911 = CARTESIAN_POINT ( 'NONE',  ( -33.42925964089140933, 11.06161099612212695, -16.55003854064094426 ) ) ;
#2912 = EDGE_CURVE ( 'NONE', #30328, #18557, #9016, .T. ) ;
#2913 = DIRECTION ( 'NONE',  ( -0.000000000000000000, -0.000000000000000000, -1.000000000000000000 ) ) ;
#2914 = VECTOR ( 'NONE', #7549, 1000.000000000000227 ) ;
#2915 = ORIENTED_EDGE ( 'NONE', *, *, #25460, .F. ) ;
#2916 = CARTESIAN_POINT ( 'NONE',  ( -15.34842816977634428, -7.387654668753818932, 5.749228751562096562 ) ) ;
#2917 = FACE_BOUND ( 'NONE', #16843, .T. ) ;
#2918 = CARTESIAN_POINT ( 'NONE',  ( 8.413215745754998309, -3.196529495465417980, 21.50000000000000000 ) ) ;
#2919 = CARTESIAN_POINT ( 'NONE',  ( -22.58267429318971864, 26.57182937991348481, 26.54355021145562787 ) ) ;
#2920 = CARTESIAN_POINT ( 'NONE',  ( -6.301234758012549619, 6.543385983536412098, 21.50000000000000000 ) ) ;
#2921 = DIRECTION ( 'NONE',  ( -0.000000000000000000, -0.000000000000000000, 1.000000000000000000 ) ) ;
#2922 = DIRECTION ( 'NONE',  ( -1.000000000000000000, 0.000000000000000000, -0.000000000000000000 ) ) ;
#2923 = ORIENTED_EDGE ( 'NONE', *, *, #7801, .F. ) ;
#2924 = ADVANCED_FACE ( 'NONE', ( #11512 ), #27736, .T. ) ;
#2925 = AXIS2_PLACEMENT_3D ( 'NONE', #23780, #18658, #16162 ) ;
#2926 = EDGE_CURVE ( 'NONE', #13104, #10035, #23491, .T. ) ;
#2927 = MANIFOLD_SOLID_BREP ( 'Cut-Extrude26', #14306 ) ;
#2928 = VECTOR ( 'NONE', #11011, 1000.000000000000000 ) ;
#2929 = CARTESIAN_POINT ( 'NONE',  ( -28.37932450449293853, 10.51822134874671022, 1.500000000000000000 ) ) ;
#2930 = CARTESIAN_POINT ( 'NONE',  ( -10.00000000000004263, 1.387778780781445676E-14, 1.500000000000000000 ) ) ;
#2931 = AXIS2_PLACEMENT_3D ( 'NONE', #27902, #7138, #23498 ) ;
#2932 = ORIENTED_EDGE ( 'NONE', *, *, #28839, .T. ) ;
#2933 = CIRCLE ( 'NONE', #7924, 0.7500000000000006661 ) ;
#2934 = ADVANCED_FACE ( 'NONE', ( #30661 ), #11361, .T. ) ;
#2935 = EDGE_LOOP ( 'NONE', ( #18951, #15081, #30148, #25140 ) ) ;
#2936 = DIRECTION ( 'NONE',  ( -0.000000000000000000, -0.000000000000000000, 1.000000000000000000 ) ) ;
#2937 = CARTESIAN_POINT ( 'NONE',  ( -14.90305376050273267, 47.72777027336211120, -53.03111353900148117 ) ) ;
#2938 = EDGE_CURVE ( 'NONE', #15816, #23899, #5708, .T. ) ;
#2939 = ORIENTED_EDGE ( 'NONE', *, *, #28576, .F. ) ;
#2940 = AXIS2_PLACEMENT_3D ( 'NONE', #21597, #18970, #2584 ) ;
#2941 = CARTESIAN_POINT ( 'NONE',  ( 12.88134121443596847, 11.13293444107316610, 19.96783386855779341 ) ) ;
#2942 = CARTESIAN_POINT ( 'NONE',  ( -9.272241372864392872, -14.27765368465080265, 7.176035686813569292 ) ) ;
#2943 = ADVANCED_FACE ( 'NONE', ( #16027 ), #30379, .F. ) ;
#2944 = ORIENTED_EDGE ( 'NONE', *, *, #19013, .T. ) ;
#2945 = CARTESIAN_POINT ( 'NONE',  ( 16.19384365167807971, -5.424445124423259657, 19.47783254395485031 ) ) ;
#2946 = CARTESIAN_POINT ( 'NONE',  ( -15.34307810681595186, 12.82926163924265950, 20.34789198813115263 ) ) ;
#2947 = CARTESIAN_POINT ( 'NONE',  ( 0.000000000000000000, 0.000000000000000000, 0.000000000000000000 ) ) ;
#2948 = ORIENTED_EDGE ( 'NONE', *, *, #14661, .F. ) ;
#2949 = DIRECTION ( 'NONE',  ( -0.000000000000000000, -0.000000000000000000, -1.000000000000000000 ) ) ;
#2950 = ORIENTED_EDGE ( 'NONE', *, *, #17613, .T. ) ;
#2951 = AXIS2_PLACEMENT_3D ( 'NONE', #22402, #11018, #15373 ) ;
#2952 = AXIS2_PLACEMENT_3D ( 'NONE', #29409, #14440, #696 ) ;
#2953 = VERTEX_POINT ( 'NONE', #20547 ) ;
#2954 = ADVANCED_FACE ( 'NONE', ( #25692 ), #28180, .F. ) ;
#2955 = CARTESIAN_POINT ( 'NONE',  ( 10.11194158890137729, 41.13960854804319212, 28.95784450080078898 ) ) ;
#2956 = CARTESIAN_POINT ( 'NONE',  ( -6.449126838413864249, 15.81136745782586672, 19.69140814234746273 ) ) ;
#2957 = CARTESIAN_POINT ( 'NONE',  ( -17.98703099176684006, -8.745510052321849415, 7.652108011868850923 ) ) ;
#2958 = EDGE_CURVE ( 'NONE', #15108, #3647, #8323, .T. ) ;
#2959 = VECTOR ( 'NONE', #26841, 1000.000000000000000 ) ;
#2960 = CARTESIAN_POINT ( 'NONE',  ( -7.669844488642329594, -15.25924058316908649, 19.25672174529527325 ) ) ;
#2961 = CARTESIAN_POINT ( 'NONE',  ( -29.46596134976465109, 27.84982784967258240, 30.27354135555054171 ) ) ;
#2962 = CARTESIAN_POINT ( 'NONE',  ( 19.74328841314636307, 3.194145055459935101, 20.34789198813115263 ) ) ;
#2963 = DIRECTION ( 'NONE',  ( -0.000000000000000000, -0.000000000000000000, 1.000000000000000000 ) ) ;
#2964 = CARTESIAN_POINT ( 'NONE',  ( -19.87987511945007313, 2.346632672767392958, 5.661398277488801867 ) ) ;
#2965 = AXIS2_PLACEMENT_3D ( 'NONE', #4053, #13580, #23058 ) ;
#2966 = CARTESIAN_POINT ( 'NONE',  ( -28.10697575488836364, 29.46351030971690932, 14.10614635148330898 ) ) ;
#2967 = PLANE ( 'NONE',  #23352 ) ;
#2968 = ORIENTED_EDGE ( 'NONE', *, *, #8843, .T. ) ;
#2969 = ORIENTED_EDGE ( 'NONE', *, *, #16012, .F. ) ;
#2970 = DIRECTION ( 'NONE',  ( -1.000000000000000000, 0.000000000000000000, 0.000000000000000000 ) ) ;
#2971 = PRODUCT_DEFINITION_SHAPE ( 'NONE', 'NONE',  #30870 ) ;
#2972 = CARTESIAN_POINT ( 'NONE',  ( 27.03074382657074537, -6.449748410230991880, 47.21042702067962438 ) ) ;
#2973 = CARTESIAN_POINT ( 'NONE',  ( -15.27764744547075182, -7.543477926807485190, 7.626437579292365321 ) ) ;
#2974 = CIRCLE ( 'NONE', #24375, 20.00000000000000000 ) ;
#2975 = LINE ( 'NONE', #615, #6934 ) ;
#2976 = ORIENTED_EDGE ( 'NONE', *, *, #14850, .T. ) ;
#2977 = DIRECTION ( 'NONE',  ( 1.000000000000000000, 0.000000000000000000, 0.000000000000000000 ) ) ;
#2978 = FACE_BOUND ( 'NONE', #6436, .T. ) ;
#2979 = CARTESIAN_POINT ( 'NONE',  ( 19.88003893156456670, 2.345734461008499583, 6.111214848085761986 ) ) ;
#2980 = ORIENTED_EDGE ( 'NONE', *, *, #15496, .T. ) ;
#2981 = CARTESIAN_POINT ( 'NONE',  ( 15.31432103507273546, 12.89133701742166771, 7.429667576816606278 ) ) ;
#2982 = VERTEX_POINT ( 'NONE', #7132 ) ;
#2983 = CARTESIAN_POINT ( 'NONE',  ( 15.84193441942129077, -6.296838616230743924, 7.652108011868850035 ) ) ;
#2984 = DIRECTION ( 'NONE',  ( 1.000000000000000000, 0.000000000000000000, 0.000000000000000000 ) ) ;
#2985 = CIRCLE ( 'NONE', #17437, 2.061368542273053883 ) ;
#2986 = DIRECTION ( 'NONE',  ( 0.000000000000000000, 0.000000000000000000, 1.000000000000000000 ) ) ;
#2987 = ORIENTED_EDGE ( 'NONE', *, *, #2137, .F. ) ;
#2988 = CARTESIAN_POINT ( 'NONE',  ( 4.772488686130579971, 19.44046140540703504, 5.810767894563978686 ) ) ;
#2989 = CARTESIAN_POINT ( 'NONE',  ( -8.840471615930058036, 1.687027447297517080, -1.500000000000001776 ) ) ;
#2990 = CARTESIAN_POINT ( 'NONE',  ( -4.622016212553093695, -12.19167610014704906, 24.50000000000000000 ) ) ;
#2991 = CARTESIAN_POINT ( 'NONE',  ( 29.03395105464274195, 23.44066905138924284, 34.50000000000000000 ) ) ;
#2992 = ADVANCED_FACE ( 'NONE', ( #7750 ), #26782, .F. ) ;
#2993 = CARTESIAN_POINT ( 'NONE',  ( 30.31220697679117038, 11.23460505553742550, 1.500000000000000000 ) ) ;
#2994 = CARTESIAN_POINT ( 'NONE',  ( -19.54426622602688468, -37.07991288358296345, -1.499999999999999778 ) ) ;
#2995 = CARTESIAN_POINT ( 'NONE',  ( 0.000000000000000000, 0.000000000000000000, -1.500000000000001332 ) ) ;
#2996 = ORIENTED_EDGE ( 'NONE', *, *, #16605, .T. ) ;
#2997 = DIRECTION ( 'NONE',  ( 0.000000000000000000, 0.000000000000000000, 1.000000000000000000 ) ) ;
#2998 = AXIS2_PLACEMENT_3D ( 'NONE', #26524, #28710, #7187 ) ;
#2999 = CARTESIAN_POINT ( 'NONE',  ( -13.83904721019128381, 9.990416291640222823, 18.64703902303423178 ) ) ;
#3000 = CYLINDRICAL_SURFACE ( 'NONE', #14301, 0.7500000000000006661 ) ;
#3001 = ORIENTED_EDGE ( 'NONE', *, *, #27898, .T. ) ;
#3002 = CARTESIAN_POINT ( 'NONE',  ( 29.54181686732680845, -27.74713163033052865, 9.373611838719332567 ) ) ;
#3003 = CARTESIAN_POINT ( 'NONE',  ( -43.65325914805313801, 67.82531758386231502, 61.81444568807134488 ) ) ;
#3004 = DIRECTION ( 'NONE',  ( -0.000000000000000000, -0.000000000000000000, 1.000000000000000000 ) ) ;
#3005 = DIRECTION ( 'NONE',  ( 0.000000000000000000, 0.000000000000000000, 1.000000000000000000 ) ) ;
#3006 = CARTESIAN_POINT ( 'NONE',  ( 37.98493438989863336, -11.12428508576153341, -1.500000000000000000 ) ) ;
#3007 = DIRECTION ( 'NONE',  ( 1.000000000000000000, 0.000000000000000000, 0.000000000000000000 ) ) ;
#3008 = CARTESIAN_POINT ( 'NONE',  ( 16.87575838019271757, 2.225846228045831321, 6.910395520694542881 ) ) ;
#3009 = LINE ( 'NONE', #21872, #30467 ) ;
#3010 = VERTEX_POINT ( 'NONE', #5410 ) ;
#3011 = DIRECTION ( 'NONE',  ( -0.000000000000000000, -0.000000000000000000, -1.000000000000000000 ) ) ;
#3012 = ORIENTED_EDGE ( 'NONE', *, *, #18180, .F. ) ;
#3013 = CARTESIAN_POINT ( 'NONE',  ( -23.07950435457408034, -11.74770253185616298, 44.86091080599459247 ) ) ;
#3014 = CARTESIAN_POINT ( 'NONE',  ( 0.000000000000000000, 0.000000000000000000, 1.500000000000001332 ) ) ;
#3015 = EDGE_LOOP ( 'NONE', ( #2324, #15455, #1577, #2558, #11670, #8360 ) ) ;
#3016 = EDGE_LOOP ( 'NONE', ( #29920, #15554 ) ) ;
#3017 = CARTESIAN_POINT ( 'NONE',  ( -9.660978277356432997, -17.51194513905169714, 6.919864475265763204 ) ) ;
#3018 = ORIENTED_EDGE ( 'NONE', *, *, #23926, .F. ) ;
#3019 = AXIS2_PLACEMENT_3D ( 'NONE', #14015, #30689, #7469 ) ;
#3020 = VERTEX_POINT ( 'NONE', #17098 ) ;
#3021 = ORIENTED_EDGE ( 'NONE', *, *, #16237, .F. ) ;
#3022 = CARTESIAN_POINT ( 'NONE',  ( -39.52380524535562500, 7.028748154183637631, -1.499999999999999556 ) ) ;
#3023 = DIRECTION ( 'NONE',  ( 0.000000000000000000, 0.000000000000000000, -1.000000000000000000 ) ) ;
#3024 = CARTESIAN_POINT ( 'NONE',  ( 0.7836604620899301210, -17.02735026737548552, 5.652196082368483587 ) ) ;
#3025 = CARTESIAN_POINT ( 'NONE',  ( -3.640207617113898841, 7.856594496258241023, -3.621320343559650379 ) ) ;
#3026 = DIRECTION ( 'NONE',  ( 1.000000000000000000, 0.000000000000000000, 0.000000000000000000 ) ) ;
#3027 = ORIENTED_EDGE ( 'NONE', *, *, #6894, .F. ) ;
#3028 = CARTESIAN_POINT ( 'NONE',  ( -10.62668044795002942, -16.94375577056505122, 7.652108011868850035 ) ) ;
#3029 = CARTESIAN_POINT ( 'NONE',  ( 0.000000000000000000, 0.000000000000000000, 1.500000000000001332 ) ) ;
#3030 = LINE ( 'NONE', #27197, #25696 ) ;
#3031 = DIRECTION ( 'NONE',  ( 0.000000000000000000, 0.000000000000000000, 1.000000000000000000 ) ) ;
#3032 = VERTEX_POINT ( 'NONE', #16643 ) ;
#3033 = DIRECTION ( 'NONE',  ( 1.000000000000000000, 0.000000000000000000, -0.000000000000000000 ) ) ;
#3034 = CARTESIAN_POINT ( 'NONE',  ( -50.00000000000000000, -50.00000000000000000, 59.49999999999999289 ) ) ;
#3035 = CARTESIAN_POINT ( 'NONE',  ( -4.776122516674677878E-15, -42.50000000000000000, 37.50000000000000000 ) ) ;
#3036 = CARTESIAN_POINT ( 'NONE',  ( 11.64616783614240880, -16.28139325077859212, 5.872146474157316831 ) ) ;
#3037 = CIRCLE ( 'NONE', #15993, 9.482273699623480212 ) ;
#3038 = VECTOR ( 'NONE', #12443, 1000.000000000000000 ) ;
#3039 = FACE_OUTER_BOUND ( 'NONE', #2044, .T. ) ;
#3040 = ORIENTED_EDGE ( 'NONE', *, *, #25557, .F. ) ;
#3041 = ORIENTED_EDGE ( 'NONE', *, *, #21813, .F. ) ;
#3042 = CARTESIAN_POINT ( 'NONE',  ( 57.49999999999998579, -50.00000000000000000, 12.49999999999999112 ) ) ;
#3043 = LINE ( 'NONE', #10373, #10161 ) ;
#3044 = CARTESIAN_POINT ( 'NONE',  ( -15.13676175850366512, 13.09931225869579308, 7.595116371587256054 ) ) ;
#3045 = DIRECTION ( 'NONE',  ( -1.000000000000000000, 0.000000000000000000, 0.000000000000000000 ) ) ;
#3046 = ORIENTED_EDGE ( 'NONE', *, *, #14327, .F. ) ;
#3047 = PRODUCT_CONTEXT ( 'NONE', #24920, 'mechanical' ) ;
#3048 = CARTESIAN_POINT ( 'NONE',  ( 49.99999999999998579, 90.00000000000001421, 22.49999999999999289 ) ) ;
#3049 = LINE ( 'NONE', #12418, #16687 ) ;
#3050 = VERTEX_POINT ( 'NONE', #4776 ) ;
#3051 = DIRECTION ( 'NONE',  ( -0.000000000000000000, -0.000000000000000000, -1.000000000000000000 ) ) ;
#3052 = CARTESIAN_POINT ( 'NONE',  ( 3.662523238938590442, -12.47340865698848056, 1.500000000000001332 ) ) ;
#3053 = DIRECTION ( 'NONE',  ( 0.000000000000000000, 0.000000000000000000, -1.000000000000000000 ) ) ;
#3054 = CARTESIAN_POINT ( 'NONE',  ( -24.74483793516321484, -32.88075240386160658, 29.75196967776350832 ) ) ;
#3055 = ORIENTED_EDGE ( 'NONE', *, *, #15547, .T. ) ;
#3056 = CARTESIAN_POINT ( 'NONE',  ( -37.16608720827707657, -65.00000000000000000, 12.49999999999999112 ) ) ;
#3057 = PRODUCT_RELATED_PRODUCT_CATEGORY ( 'part', '', ( #26888 ) ) ;
#3058 = B_SPLINE_CURVE_WITH_KNOTS ( 'NONE', 3,
 ( #5346, #19221, #7387, #21710 ),
 .UNSPECIFIED., .F., .F.,
 ( 4, 4 ),
 ( 3.018024802580205417E-07, 0.007932103453629112816 ),
 .UNSPECIFIED. ) ;
#3059 = CIRCLE ( 'NONE', #7036, 0.7500000000000004441 ) ;
#3060 = CARTESIAN_POINT ( 'NONE',  ( 5.184529477212510784, 43.72990366966700293, -16.50000000000000000 ) ) ;
#3061 = CARTESIAN_POINT ( 'NONE',  ( -19.69679205574297498, 3.469720661875630885, 19.60917204426171168 ) ) ;
#3062 = VERTEX_POINT ( 'NONE', #14915 ) ;
#3063 = FACE_OUTER_BOUND ( 'NONE', #14383, .T. ) ;
#3064 = PLANE ( 'NONE',  #10811 ) ;
#3065 = EDGE_CURVE ( 'NONE', #15686, #4883, #21170, .T. ) ;
#3066 = DIRECTION ( 'NONE',  ( -1.156482317317871725E-15, 1.000000000000000000, 0.000000000000000000 ) ) ;
#3067 = CARTESIAN_POINT ( 'NONE',  ( -37.99999999999999289, 209.2686044187655909, -22.50000000000000711 ) ) ;
#3068 = PLANE ( 'NONE',  #24267 ) ;
#3069 = CARTESIAN_POINT ( 'NONE',  ( 37.79362409831109915, -10.49224821554092735, 11.60540311995022833 ) ) ;
#3070 = CARTESIAN_POINT ( 'NONE',  ( 0.000000000000000000, 12.49999999999999289, -16.50000000000000000 ) ) ;
#3071 = EDGE_LOOP ( 'NONE', ( #28632, #29334, #17079, #4765 ) ) ;
#3072 = AXIS2_PLACEMENT_3D ( 'NONE', #8414, #30384, #20407 ) ;
#3073 = DIRECTION ( 'NONE',  ( 0.000000000000000000, 0.000000000000000000, -1.000000000000000000 ) ) ;
#3074 = CARTESIAN_POINT ( 'NONE',  ( 6.364020599487797192, -6.482337650448430466, 21.50000000000000000 ) ) ;
#3075 = ADVANCED_FACE ( 'NONE', ( #21464, #14750, #10079, #559, #2917, #18990 ), #258, .F. ) ;
#3076 = ORIENTED_EDGE ( 'NONE', *, *, #19874, .T. ) ;
#3077 = ORIENTED_EDGE ( 'NONE', *, *, #5666, .F. ) ;
#3078 = EDGE_CURVE ( 'NONE', #20938, #6747, #12437, .T. ) ;
#3079 = DIRECTION ( 'NONE',  ( -1.000000000000000000, 0.000000000000000000, 0.000000000000000000 ) ) ;
#3080 = CARTESIAN_POINT ( 'NONE',  ( -14.23021073309091733, 47.93387744827222718, -59.84518500609045333 ) ) ;
#3081 =( NAMED_UNIT ( * ) PLANE_ANGLE_UNIT ( ) SI_UNIT ( $, .RADIAN. ) );
#3082 = EDGE_LOOP ( 'NONE', ( #30567, #28647, #13272, #27650 ) ) ;
#3083 = CIRCLE ( 'NONE', #25993, 9.084132297865673777 ) ;
#3084 = CARTESIAN_POINT ( 'NONE',  ( -24.42252949794886163, -29.12958095736449593, 27.50000000000000355 ) ) ;
#3085 = CARTESIAN_POINT ( 'NONE',  ( 15.53918631077679180, 12.61944498292910488, 19.11611934778430921 ) ) ;
#3086 = CARTESIAN_POINT ( 'NONE',  ( -11.29739510359497245, -16.52539200402570785, 7.080843742048788414 ) ) ;
#3087 = ORIENTED_EDGE ( 'NONE', *, *, #30388, .T. ) ;
#3088 = CARTESIAN_POINT ( 'NONE',  ( -16.90489691178406062, 2.092419235659074506, 7.557577766377196582 ) ) ;
#3089 = CARTESIAN_POINT ( 'NONE',  ( 18.08129319977582838, -8.548428815984333795, 5.849008070840543638 ) ) ;
#3090 = DIRECTION ( 'NONE',  ( -0.8412535328311804284, 0.5406408174555987767, 0.000000000000000000 ) ) ;
#3091 = ORIENTED_EDGE ( 'NONE', *, *, #11882, .T. ) ;
#3092 = DIRECTION ( 'NONE',  ( 0.000000000000000000, 0.000000000000000000, -1.000000000000000000 ) ) ;
#3093 = EDGE_CURVE ( 'NONE', #23779, #12979, #11296, .T. ) ;
#3094 = ORIENTED_EDGE ( 'NONE', *, *, #13534, .F. ) ;
#3095 = EDGE_CURVE ( 'NONE', #10630, #4361, #28500, .T. ) ;
#3096 = VECTOR ( 'NONE', #3650, 1000.000000000000000 ) ;
#3097 = EDGE_CURVE ( 'NONE', #28559, #9226, #24111, .T. ) ;
#3098 = CARTESIAN_POINT ( 'NONE',  ( 25.20647278166642735, 28.20479727972634265, 27.50000000000001066 ) ) ;
#3099 = ORIENTED_EDGE ( 'NONE', *, *, #24475, .T. ) ;
#3100 = EDGE_CURVE ( 'NONE', #14341, #26022, #2604, .T. ) ;
#3101 = CARTESIAN_POINT ( 'NONE',  ( 38.98831344968873935, -1.224499394254795703, 32.22844543117250993 ) ) ;
#3102 = CARTESIAN_POINT ( 'NONE',  ( -6.938992678473724141, 18.77645360485810144, 19.25672174529527325 ) ) ;
#3103 = CARTESIAN_POINT ( 'NONE',  ( -14.82920317518825293, 13.44671003463071735, 19.96783386855779341 ) ) ;
#3104 = CIRCLE ( 'NONE', #29941, 9.482273699623480212 ) ;
#3105 = CARTESIAN_POINT ( 'NONE',  ( -4.608906612435655248, -7.730328572437724866, -1.500000000000002665 ) ) ;
#3106 = EDGE_CURVE ( 'NONE', #15032, #27003, #14455, .T. ) ;
#3107 = CARTESIAN_POINT ( 'NONE',  ( -36.55886824564901616, 15.02606788761555379, 31.54031350539812806 ) ) ;
#3108 = LINE ( 'NONE', #24769, #14010 ) ;
#3109 = CARTESIAN_POINT ( 'NONE',  ( -24.35970437652574105, -13.37404834226503070, 42.96778633356041865 ) ) ;
#3110 = VERTEX_POINT ( 'NONE', #12273 ) ;
#3111 = ADVANCED_FACE ( 'NONE', ( #9931 ), #3064, .F. ) ;
#3112 = CARTESIAN_POINT ( 'NONE',  ( -19.90092023446657521, 2.162276205174161081, 5.704143890883081269 ) ) ;
#3113 = CARTESIAN_POINT ( 'NONE',  ( 32.02497887436175006, -18.15461798050466413, 34.49999999999999289 ) ) ;
#3114 = CARTESIAN_POINT ( 'NONE',  ( 19.87928744571104289, 2.194067154482769677, 6.781503518395076036 ) ) ;
#3115 = ORIENTED_EDGE ( 'NONE', *, *, #21996, .T. ) ;
#3116 = ORIENTED_EDGE ( 'NONE', *, *, #1601, .T. ) ;
#3117 = DIRECTION ( 'NONE',  ( -0.000000000000000000, -0.000000000000000000, 1.000000000000000000 ) ) ;
#3118 = AXIS2_PLACEMENT_3D ( 'NONE', #7454, #26318, #14463 ) ;
#3119 = CARTESIAN_POINT ( 'NONE',  ( -4.163336342344337027E-14, 1.387778780781445676E-14, 1.500000000000000000 ) ) ;
#3120 = ORIENTED_EDGE ( 'NONE', *, *, #18921, .F. ) ;
#3121 = DIRECTION ( 'NONE',  ( 0.000000000000000000, 0.000000000000000000, 1.000000000000000000 ) ) ;
#3122 = DIRECTION ( 'NONE',  ( 1.000000000000000000, 0.000000000000000000, 0.000000000000000000 ) ) ;
#3123 = CARTESIAN_POINT ( 'NONE',  ( -38.00000000000000000, 65.00000000000000000, -7.533656238527846826E-15 ) ) ;
#3124 = ADVANCED_FACE ( 'NONE', ( #1191 ), #17710, .F. ) ;
#3125 = ORIENTED_EDGE ( 'NONE', *, *, #26838, .F. ) ;
#3126 = DIRECTION ( 'NONE',  ( -0.3598999890241658117, -0.9329908884337538844, 0.000000000000000000 ) ) ;
#3127 = DIRECTION ( 'NONE',  ( -1.000000000000000000, 0.000000000000000000, 0.000000000000000000 ) ) ;
#3128 = CARTESIAN_POINT ( 'NONE',  ( 16.86769344895232337, 2.296683858978091575, 6.211014596808754007 ) ) ;
#3129 = ORIENTED_EDGE ( 'NONE', *, *, #29186, .T. ) ;
#3130 = CARTESIAN_POINT ( 'NONE',  ( 15.55295851173241672, 12.60248606922869463, 6.755862304746362845 ) ) ;
#3131 = EDGE_CURVE ( 'NONE', #25497, #6824, #26753, .T. ) ;
#3132 = ORIENTED_EDGE ( 'NONE', *, *, #10484, .F. ) ;
#3133 = CARTESIAN_POINT ( 'NONE',  ( 18.55936137128098196, -7.500557692851355540, 7.500147780736496017 ) ) ;
#3134 = ADVANCED_FACE ( 'NONE', ( #22686 ), #27231, .F. ) ;
#3135 = CARTESIAN_POINT ( 'NONE',  ( -33.42925964089140933, 11.06161099612212695, 39.78814634291943264 ) ) ;
#3136 = CARTESIAN_POINT ( 'NONE',  ( -24.85846090629200589, 6.933313039714898984, 44.95040115368838229 ) ) ;
#3137 = ORIENTED_EDGE ( 'NONE', *, *, #11882, .F. ) ;
#3138 = AXIS2_PLACEMENT_3D ( 'NONE', #27047, #24858, #15169 ) ;
#3139 = CARTESIAN_POINT ( 'NONE',  ( -4.163336342344337027E-14, 1.387778780781445676E-14, 1.500000000000000000 ) ) ;
#3140 = AXIS2_PLACEMENT_3D ( 'NONE', #24833, #1596, #8612 ) ;
#3141 = CARTESIAN_POINT ( 'NONE',  ( 39.99999999999998579, 80.00000000000001421, 52.49999999999999289 ) ) ;
#3142 = CARTESIAN_POINT ( 'NONE',  ( -21.71568325578193637, 0.000000000000000000, 1.500000000000000000 ) ) ;
#3143 = DIRECTION ( 'NONE',  ( -0.000000000000000000, -0.000000000000000000, -1.000000000000000000 ) ) ;
#3144 = CARTESIAN_POINT ( 'NONE',  ( -23.69412710310941961, 29.84645176427129698, 27.50000000000001066 ) ) ;
#3145 = CARTESIAN_POINT ( 'NONE',  ( 9.135582339684646058, -14.36547911245297549, 19.87181966307587544 ) ) ;
#3146 = VERTEX_POINT ( 'NONE', #3687 ) ;
#3147 = CARTESIAN_POINT ( 'NONE',  ( -25.88640477275121299, -6.345529225273951468, 48.34755156421752531 ) ) ;
#3148 = CARTESIAN_POINT ( 'NONE',  ( -23.96732207939035675, 33.98584080153585774, -1.500000000000000000 ) ) ;
#3149 = DIRECTION ( 'NONE',  ( 1.000000000000000000, 0.000000000000000000, 0.000000000000000000 ) ) ;
#3150 = ORIENTED_EDGE ( 'NONE', *, *, #24456, .F. ) ;
#3151 = CARTESIAN_POINT ( 'NONE',  ( 30.28907500942318620, -26.77591773196712310, 8.779599968084907502 ) ) ;
#3152 = CARTESIAN_POINT ( 'NONE',  ( 0.000000000000000000, 0.000000000000000000, 1.500000000000001332 ) ) ;
#3153 = B_SPLINE_SURFACE_WITH_KNOTS ( 'NONE', 3, 1, ( 
 ( #24341, #3283 ),
 ( #19362, #19197 ),
 ( #5012, #7362 ),
 ( #24019, #28883 ),
 ( #5163, #24173 ),
 ( #12348, #10005 ),
 ( #2988, #27773 ),
 ( #8595, #22925 ),
 ( #5942, #19976 ),
 ( #20440, #29813 ),
 ( #24808, #3755 ),
 ( #3919, #3598 ),
 ( #13275, #15440 ),
 ( #10941, #6086 ),
 ( #8455, #18100 ),
 ( #952, #22615 ),
 ( #13121, #20286 ),
 ( #8284, #6402 ),
 ( #10617, #29496 ),
 ( #27618, #6241 ),
 ( #17800, #1573 ),
 ( #27465, #11080 ),
 ( #5783, #15749 ),
 ( #3445, #20577 ),
 ( #8131, #30103 ),
 ( #18253, #22767 ),
 ( #15922, #13586 ),
 ( #12966, #27314 ),
 ( #1263, #10463 ),
 ( #17640, #24961 ),
 ( #20130, #27157 ) ),
 .UNSPECIFIED., .F., .F., .F.,
 ( 4, 3, 3, 3, 3, 3, 3, 3, 3, 3, 4 ),
 ( 2, 2 ),
 ( 0.4999999998345677765, 0.5360336730431942698, 0.5907651151589017324, 0.6456034593241839481, 0.6998270958050443191, 0.7529536536315944995, 0.8052385063053264513, 0.8575343587103996246, 0.9106564858195047574, 0.9648414833209688624, 1.000000006602610014 ),
 ( 0.000000000000000000, 1.000000000000000000 ),
 .UNSPECIFIED. ) ;
#3154 = CARTESIAN_POINT ( 'NONE',  ( -14.67655575066035567, 13.58671083542089164, 19.21471108562413832 ) ) ;
#3155 = FACE_OUTER_BOUND ( 'NONE', #15975, .T. ) ;
#3156 = CARTESIAN_POINT ( 'NONE',  ( -13.22505861668333083, 42.10773672057167261, -19.50000000000000355 ) ) ;
#3157 = CARTESIAN_POINT ( 'NONE',  ( -0.9621688436940066813, -9.033033306777454641, 13.22130136205108641 ) ) ;
#3158 = AXIS2_PLACEMENT_3D ( 'NONE', #18234, #10916, #20419 ) ;
#3159 = DIRECTION ( 'NONE',  ( 0.000000000000000000, -1.132880637372608986E-16, 1.000000000000000000 ) ) ;
#3160 = EDGE_CURVE ( 'NONE', #5226, #1513, #29453, .T. ) ;
#3162 = AXIS2_PLACEMENT_3D ( 'NONE', #22289, #1247, #22905 ) ;
#3161 = CARTESIAN_POINT ( 'NONE',  ( 19.72123249184183180, 3.330269068327012416, 5.652912763329821288 ) ) ;
#3163 = ORIENTED_EDGE ( 'NONE', *, *, #21544, .F. ) ;
#3164 = EDGE_CURVE ( 'NONE', #7313, #12572, #3448, .T. ) ;
#3165 = CARTESIAN_POINT ( 'NONE',  ( 33.25198513809822742, -23.59839681648444554, -8.166573414591441704 ) ) ;
#3166 = CARTESIAN_POINT ( 'NONE',  ( -1.438332125858111432, 8.884323311075791096, 1.500000000000001332 ) ) ;
#3167 = DIRECTION ( 'NONE',  ( 0.000000000000000000, 0.000000000000000000, -1.000000000000000000 ) ) ;
#3168 = VERTEX_POINT ( 'NONE', #3533 ) ;
#3169 = VERTEX_POINT ( 'NONE', #8369 ) ;
#3170 = DIRECTION ( 'NONE',  ( 0.5406408174555974444, 0.8412535328311813165, 0.000000000000000000 ) ) ;
#3171 = EDGE_LOOP ( 'NONE', ( #8120, #8402, #16204, #20861 ) ) ;
#3172 = ORIENTED_EDGE ( 'NONE', *, *, #29040, .T. ) ;
#3173 = DIRECTION ( 'NONE',  ( 1.000000000000000000, 0.000000000000000000, 0.000000000000000000 ) ) ;
#3174 = LINE ( 'NONE', #15164, #5307 ) ;
#3175 = MANIFOLD_SOLID_BREP ( 'Boss-Extrude22', #18321 ) ;
#3176 = CARTESIAN_POINT ( 'NONE',  ( 39.52380524535562500, 7.028748154183637631, -6.500000000000000888 ) ) ;
#3177 = CARTESIAN_POINT ( 'NONE',  ( -37.98866957712698422, 9.615774924837397819, 13.14437204739174447 ) ) ;
#3178 = CARTESIAN_POINT ( 'NONE',  ( -19.54426622602688113, -37.07991288358296345, 1.499999999999999778 ) ) ;
#3179 = VERTEX_POINT ( 'NONE', #29427 ) ;
#3180 = VECTOR ( 'NONE', #5263, 1000.000000000000114 ) ;
#3181 = CARTESIAN_POINT ( 'NONE',  ( 2.431858781452735485, 8.752572334588128555, -1.500000000000000666 ) ) ;
#3182 = DIRECTION ( 'NONE',  ( 0.000000000000000000, -0.000000000000000000, -1.000000000000000000 ) ) ;
#3183 = DIRECTION ( 'NONE',  ( 0.6548607339452889864, 0.7557495743542548272, 0.000000000000000000 ) ) ;
#3184 = PLANE ( 'NONE',  #25082 ) ;
#3185 = VERTEX_POINT ( 'NONE', #23452 ) ;
#3186 = VECTOR ( 'NONE', #22517, 1000.000000000000000 ) ;
#3187 = CARTESIAN_POINT ( 'NONE',  ( -9.272241372864389319, -14.27765368465079554, 19.87181966307587544 ) ) ;
#3188 = PLANE ( 'NONE',  #23740 ) ;
#3189 = CARTESIAN_POINT ( 'NONE',  ( -6.889674169070709731, 18.79461648230378046, 6.341840715582230281 ) ) ;
#3190 = CARTESIAN_POINT ( 'NONE',  ( 11.94417982595701488, -16.06366807669216357, 6.782048567692550378 ) ) ;
#3191 = CARTESIAN_POINT ( 'NONE',  ( 2.552544031601107211, 42.49999999998228617, -1.500000000000000000 ) ) ;
#3192 = CARTESIAN_POINT ( 'NONE',  ( 33.41032657756569080, -9.567127522732027600, 36.00434311239766316 ) ) ;
#3193 = ORIENTED_EDGE ( 'NONE', *, *, #21172, .F. ) ;
#3194 = ORIENTED_EDGE ( 'NONE', *, *, #11481, .T. ) ;
#3195 = LINE ( 'NONE', #2892, #25607 ) ;
#3196 = CARTESIAN_POINT ( 'NONE',  ( -14.69323076807464723, 13.59505578765952549, 6.530762810602277924 ) ) ;
#3197 = DIRECTION ( 'NONE',  ( -0.000000000000000000, -0.000000000000000000, -1.000000000000000000 ) ) ;
#3198 = EDGE_LOOP ( 'NONE', ( #19255, #16334, #11393, #10706 ) ) ;
#3199 = CARTESIAN_POINT ( 'NONE',  ( 15.79886199502268695, -6.395730384537282376, 18.34777357837152323 ) ) ;
#3200 = CARTESIAN_POINT ( 'NONE',  ( -40.00000000000002842, 80.00000000000001421, 22.49999999999983302 ) ) ;
#3201 = VECTOR ( 'NONE', #9905, 1000.000000000000000 ) ;
#3202 = EDGE_LOOP ( 'NONE', ( #14173, #21790, #16560, #10752 ) ) ;
#3203 = DIRECTION ( 'NONE',  ( -0.000000000000000000, -0.000000000000000000, 1.000000000000000000 ) ) ;
#3204 = CARTESIAN_POINT ( 'NONE',  ( 49.99999999999998579, -50.00000000000000000, 52.07879600563550326 ) ) ;
#3205 = CARTESIAN_POINT ( 'NONE',  ( -7.671759676023388153, -15.25818751172876553, 19.47952243369110192 ) ) ;
#3206 = CARTESIAN_POINT ( 'NONE',  ( -34.24553848958673541, -20.37971379545431105, 31.04075131429937073 ) ) ;
#3207 = ORIENTED_EDGE ( 'NONE', *, *, #28683, .T. ) ;
#3208 = DIRECTION ( 'NONE',  ( 0.000000000000000000, 1.000000000000000000, 0.000000000000000000 ) ) ;
#3209 = DIRECTION ( 'NONE',  ( 0.000000000000000000, 0.000000000000000000, 1.000000000000000000 ) ) ;
#3210 = CYLINDRICAL_SURFACE ( 'NONE', #17248, 20.00000000000000355 ) ;
#3211 = ORIENTED_EDGE ( 'NONE', *, *, #22111, .T. ) ;
#3212 = DIRECTION ( 'NONE',  ( 0.000000000000000000, -1.000000000000000000, 0.000000000000000000 ) ) ;
#3213 = DIRECTION ( 'NONE',  ( -0.000000000000000000, -0.000000000000000000, -1.000000000000000000 ) ) ;
#3214 =( NAMED_UNIT ( * ) SI_UNIT ( $, .STERADIAN. ) SOLID_ANGLE_UNIT ( ) );
#3215 = PRODUCT_DEFINITION_SHAPE ( 'NONE', 'NONE',  #30863 ) ;
#3216 = CARTESIAN_POINT ( 'NONE',  ( -3.469446951953614189E-15, -30.50000000000000711, 1.500000000000000000 ) ) ;
#3217 = CARTESIAN_POINT ( 'NONE',  ( -26.80246859415415273, 7.028748154183637631, -1.499999999999999556 ) ) ;
#3218 = CARTESIAN_POINT ( 'NONE',  ( 126.5359999999999872, 0.000000000000000000, 0.000000000000000000 ) ) ;
#3219 = VECTOR ( 'NONE', #27139, 1000.000000000000000 ) ;
#3220 = CARTESIAN_POINT ( 'NONE',  ( 37.66982319287888004, -11.00826088415979775, 11.23380626198473387 ) ) ;
#3221 = CYLINDRICAL_SURFACE ( 'NONE', #20837, 12.50000000000000000 ) ;
#3222 = ORIENTED_EDGE ( 'NONE', *, *, #6966, .T. ) ;
#3223 = CARTESIAN_POINT ( 'NONE',  ( 19.49999999999992539, 1.626584906615178899E-14, 62.49999999999999289 ) ) ;
#3224 = CARTESIAN_POINT ( 'NONE',  ( 4.507962051892418387, 19.48556068265256513, 6.037995405461189513 ) ) ;
#3225 = ORIENTED_EDGE ( 'NONE', *, *, #3454, .F. ) ;
#3226 = EDGE_CURVE ( 'NONE', #28141, #26677, #14733, .T. ) ;
#3227 = CARTESIAN_POINT ( 'NONE',  ( -7.114862909856333850, 41.83185039483213075, 20.27422947789757046 ) ) ;
#3228 = CARTESIAN_POINT ( 'NONE',  ( -48.64405085385531180, 18.29172496293576344, 24.50000000000000355 ) ) ;
#3229 = ORIENTED_EDGE ( 'NONE', *, *, #29002, .F. ) ;
#3230 = CARTESIAN_POINT ( 'NONE',  ( -35.98785884342813546, 1.199078351611056137, 27.50000000000001066 ) ) ;
#3231 = CARTESIAN_POINT ( 'NONE',  ( 12.91913032519423865, 11.08701612049549823, 19.87181966307587544 ) ) ;
#3232 = ORIENTED_EDGE ( 'NONE', *, *, #68, .T. ) ;
#3233 = EDGE_CURVE ( 'NONE', #16129, #1286, #28681, .T. ) ;
#3234 = CARTESIAN_POINT ( 'NONE',  ( 13.88429941593329531, 16.69721919943964039, -1.500000000000000000 ) ) ;
#3235 = CARTESIAN_POINT ( 'NONE',  ( 16.73141127408299411, 3.267558643021993614, 20.34789198813115263 ) ) ;
#3236 = DIRECTION ( 'NONE',  ( 0.000000000000000000, -1.132880637372608986E-16, 1.000000000000000000 ) ) ;
#3237 = ORIENTED_EDGE ( 'NONE', *, *, #12204, .T. ) ;
#3238 = CARTESIAN_POINT ( 'NONE',  ( -4.950721362025076289, 16.29421905982281871, 20.14907003336613300 ) ) ;
#3239 = CIRCLE ( 'NONE', #17169, 0.7499999999999997780 ) ;
#3240 = LINE ( 'NONE', #906, #8862 ) ;
#3241 = VERTEX_POINT ( 'NONE', #15992 ) ;
#3242 = EDGE_CURVE ( 'NONE', #14300, #23449, #28183, .T. ) ;
#3243 = CARTESIAN_POINT ( 'NONE',  ( 0.000000000000000000, 80.00000000000000000, 50.49999999999998579 ) ) ;
#3244 = CARTESIAN_POINT ( 'NONE',  ( 19.70397673731431709, 3.532048315275338357, 5.704143890883081269 ) ) ;
#3245 = DIRECTION ( 'NONE',  ( 0.000000000000000000, 0.000000000000000000, 1.000000000000000000 ) ) ;
#3246 = CARTESIAN_POINT ( 'NONE',  ( -10.14013680258725891, -17.25966085745527678, 18.44527579819791185 ) ) ;
#3247 = CARTESIAN_POINT ( 'NONE',  ( -29.06340618096728434, 28.34784734514725812, 30.22145900126884754 ) ) ;
#3248 = CARTESIAN_POINT ( 'NONE',  ( -4.776122516674677878E-15, -42.50000000000000000, 32.26246401786215046 ) ) ;
#3249 = CARTESIAN_POINT ( 'NONE',  ( -8.546423435383418976, -14.74799740001549786, 18.34798005863078885 ) ) ;
#3250 = EDGE_LOOP ( 'NONE', ( #27903, #20834, #20462, #18701 ) ) ;
#3251 = DIRECTION ( 'NONE',  ( 0.000000000000000000, 0.000000000000000000, 1.000000000000000000 ) ) ;
#3252 = CARTESIAN_POINT ( 'NONE',  ( -32.98805937973593672, 22.67054169308932288, 8.000000000000003553 ) ) ;
#3253 = DIRECTION ( 'NONE',  ( -0.000000000000000000, -1.000000000000000000, -0.000000000000000000 ) ) ;
#3254 = VERTEX_POINT ( 'NONE', #11614 ) ;
#3255 = ORIENTED_EDGE ( 'NONE', *, *, #18875, .T. ) ;
#3256 = AXIS2_PLACEMENT_3D ( 'NONE', #24841, #22801, #10967 ) ;
#3257 = CARTESIAN_POINT ( 'NONE',  ( 18.23136487193858102, -8.223889151411999165, 18.37250658438899009 ) ) ;
#3258 = EDGE_CURVE ( 'NONE', #4676, #624, #19205, .T. ) ;
#3259 = CARTESIAN_POINT ( 'NONE',  ( 10.27753383451899438, -17.15735655630021128, 6.386539667786106378 ) ) ;
#3260 = EDGE_CURVE ( 'NONE', #27498, #8808, #6482, .T. ) ;
#3261 = CARTESIAN_POINT ( 'NONE',  ( -4.163336342344337027E-14, 1.387778780781445676E-14, 24.50000000000000000 ) ) ;
#3262 = ORIENTED_EDGE ( 'NONE', *, *, #23694, .T. ) ;
#3263 = DIRECTION ( 'NONE',  ( 0.000000000000000000, 0.000000000000000000, 1.000000000000000000 ) ) ;
#3264 = CARTESIAN_POINT ( 'NONE',  ( 39.99999999999998579, 80.00000000000001421, 27.49999999999998934 ) ) ;
#3265 = DIRECTION ( 'NONE',  ( -0.000000000000000000, -0.000000000000000000, -1.000000000000000000 ) ) ;
#3266 = EDGE_LOOP ( 'NONE', ( #24974, #25472 ) ) ;
#3267 = EDGE_CURVE ( 'NONE', #8258, #29295, #30236, .T. ) ;
#3268 = CARTESIAN_POINT ( 'NONE',  ( -37.16608720827707657, -36.86186943028246787, 57.49999999999999289 ) ) ;
#3269 = AXIS2_PLACEMENT_3D ( 'NONE', #6130, #8777, #6450 ) ;
#3270 = CARTESIAN_POINT ( 'NONE',  ( -20.71335220384823117, 27.86167394782616213, -16.50000600000000262 ) ) ;
#3271 = CARTESIAN_POINT ( 'NONE',  ( 16.87335920545514867, 2.247671665613723668, 6.310736198168394928 ) ) ;
#3272 = ORIENTED_EDGE ( 'NONE', *, *, #23873, .T. ) ;
#3273 = B_SPLINE_CURVE_WITH_KNOTS ( 'NONE', 3,
 ( #14912, #25036, #22395, #24416, #26933, #15052, #5862, #3061, #12582, #10075, #12734, #870, #3529, #27396, #27227, #17559, #7907, #13046 ),
 .UNSPECIFIED., .F., .F.,
 ( 4, 2, 2, 2, 2, 2, 2, 2, 4 ),
 ( 0.003174295595554305679, 0.003570702171545538008, 0.003967108747536769904, 0.004363515323528002234, 0.004759921899519234563, 0.005156328475510466025, 0.005552735051501698355, 0.005949141627492930684, 0.006345548203484163013 ),
 .UNSPECIFIED. ) ;
#3274 = CARTESIAN_POINT ( 'NONE',  ( 27.03074382657074537, 6.449748410230989215, 47.21042702067963148 ) ) ;
#3275 = EDGE_LOOP ( 'NONE', ( #23322, #11740, #13472, #3657 ) ) ;
#3276 = ADVANCED_FACE ( 'NONE', ( #20816, #25355 ), #16144, .T. ) ;
#3277 = CARTESIAN_POINT ( 'NONE',  ( 25.48568755041062417, 12.36160011285428872, 1.500000000000001332 ) ) ;
#3278 = DIRECTION ( 'NONE',  ( 1.000000000000000000, 0.000000000000000000, 0.000000000000000000 ) ) ;
#3279 = ADVANCED_FACE ( 'NONE', ( #1952 ), #27998, .F. ) ;
#3280 = ORIENTED_EDGE ( 'NONE', *, *, #9923, .F. ) ;
#3282 = EDGE_CURVE ( 'NONE', #24053, #16046, #17235, .T. ) ;
#3281 = CIRCLE ( 'NONE', #15728, 9.482273699623480212 ) ;
#3283 = CARTESIAN_POINT ( 'NONE',  ( 4.045241160498771471, 16.55840174588941238, 5.652196082364323360 ) ) ;
#3284 = DIRECTION ( 'NONE',  ( 0.000000000000000000, 0.000000000000000000, -1.000000000000000000 ) ) ;
#3285 = DIRECTION ( 'NONE',  ( 1.000000000000000000, 0.000000000000000000, 0.000000000000000000 ) ) ;
#3286 = CARTESIAN_POINT ( 'NONE',  ( 5.090001874368171642, 39.11868163644495411, 34.49999999999999289 ) ) ;
#3287 = AXIS2_PLACEMENT_3D ( 'NONE', #9817, #19330, #3251 ) ;
#3288 = CARTESIAN_POINT ( 'NONE',  ( -35.89043209166185022, -3.548455793344783338, 34.73498294778838869 ) ) ;
#3289 = CARTESIAN_POINT ( 'NONE',  ( 9.027514758752761992, -14.43064536408542509, 19.56050940960062690 ) ) ;
#3290 = CARTESIAN_POINT ( 'NONE',  ( 31.10273980501927227, 15.38400267427140200, 40.30072466179758806 ) ) ;
#3291 = ORIENTED_EDGE ( 'NONE', *, *, #14151, .T. ) ;
#3292 = CARTESIAN_POINT ( 'NONE',  ( -24.44496207165490276, -7.595930209050158588, 49.40206402021039622 ) ) ;
#3293 = CARTESIAN_POINT ( 'NONE',  ( -13.43037651602831950, 10.49991632925268625, 18.34838970509067479 ) ) ;
#3294 = AXIS2_PLACEMENT_3D ( 'NONE', #17421, #18036, #8372 ) ;
#3295 = DIRECTION ( 'NONE',  ( 1.000000000000000000, 4.440892098500626162E-15, 0.000000000000000000 ) ) ;
#3296 = VERTEX_POINT ( 'NONE', #21107 ) ;
#3297 = LINE ( 'NONE', #22471, #18767 ) ;
#3298 = EDGE_CURVE ( 'NONE', #24948, #30496, #6763, .T. ) ;
#3299 = CARTESIAN_POINT ( 'NONE',  ( -44.60412845616029642, 68.57966488780255077, 61.38406448208059629 ) ) ;
#3300 = ADVANCED_FACE ( 'NONE', ( #1799 ), #10759, .T. ) ;
#3301 = CARTESIAN_POINT ( 'NONE',  ( 37.99999999999999289, 90.00000000000001421, -34.50000000000000000 ) ) ;
#3302 = FACE_OUTER_BOUND ( 'NONE', #18032, .T. ) ;
#3303 = CARTESIAN_POINT ( 'NONE',  ( -8.419710366748644148, 7.777014463793872956, 1.500000000000000000 ) ) ;
#3304 = EDGE_CURVE ( 'NONE', #10421, #30261, #25815, .T. ) ;
#3305 = CYLINDRICAL_SURFACE ( 'NONE', #20358, 0.7500000000000006661 ) ;
#3306 = AXIS2_PLACEMENT_3D ( 'NONE', #14798, #24620, #7488 ) ;
#3307 = CARTESIAN_POINT ( 'NONE',  ( 5.060094141397912360, 42.14075867279367316, 28.87075318537528190 ) ) ;
#3308 = ORIENTED_EDGE ( 'NONE', *, *, #6548, .T. ) ;
#3309 = VECTOR ( 'NONE', #19863, 1000.000000000000000 ) ;
#3310 = EDGE_CURVE ( 'NONE', #526, #16582, #9751, .T. ) ;
#3311 = CIRCLE ( 'NONE', #16750, 0.7500000000000006661 ) ;
#3312 = CARTESIAN_POINT ( 'NONE',  ( -33.48610676296128474, -10.91424270342314529, 35.53783135159724793 ) ) ;
#3313 = LINE ( 'NONE', #980, #26168 ) ;
#3314 = ORIENTED_EDGE ( 'NONE', *, *, #20782, .F. ) ;
#3315 = EDGE_LOOP ( 'NONE', ( #23654, #10716, #18880, #14033 ) ) ;
#3316 = EDGE_CURVE ( 'NONE', #7486, #18819, #13809, .T. ) ;
#3317 = DIRECTION ( 'NONE',  ( -1.000000000000000000, 0.000000000000000000, 0.000000000000000000 ) ) ;
#3318 = VECTOR ( 'NONE', #2247, 1000.000000000000000 ) ;
#3319 = ORIENTED_EDGE ( 'NONE', *, *, #16402, .T. ) ;
#3320 = CARTESIAN_POINT ( 'NONE',  ( 42.49999999999998579, -50.00000000000000000, -87.50000000000000000 ) ) ;
#3321 = COLOUR_RGB ( '',0.7921568627450980005, 0.8196078431372548767, 0.9333333333333333481 ) ;
#3322 = CARTESIAN_POINT ( 'NONE',  ( -9.996178806698672759, 37.96205643617683023, 34.49999999999998579 ) ) ;
#3323 = B_SPLINE_CURVE_WITH_KNOTS ( 'NONE', 3,
 ( #17499, #22325, #965, #29507, #8144, #20735 ),
 .UNSPECIFIED., .F., .F.,
 ( 4, 2, 4 ),
 ( 2.111164903073641161E-07, 0.0003706953849294931068, 0.0007411796533686788348 ),
 .UNSPECIFIED. ) ;
#3324 = CARTESIAN_POINT ( 'NONE',  ( 10.18506332983503349, -29.04537757311073420, 1.500000000000000000 ) ) ;
#3325 = CARTESIAN_POINT ( 'NONE',  ( -37.98737094879278686, 9.621865500938454829, 12.81607210702588340 ) ) ;
#3326 = VECTOR ( 'NONE', #3203, 1000.000000000000000 ) ;
#3327 = VECTOR ( 'NONE', #27041, 1000.000000000000000 ) ;
#3328 = CARTESIAN_POINT ( 'NONE',  ( -22.58267429318971864, 26.57182937991348481, -1.500000000000001332 ) ) ;
#3329 = CARTESIAN_POINT ( 'NONE',  ( 0.000000000000000000, 0.000000000000000000, 1.500000000000001332 ) ) ;
#3330 = CARTESIAN_POINT ( 'NONE',  ( 1.009606305713755203, -17.02204649693582539, 5.678370764302467677 ) ) ;
#3331 = CARTESIAN_POINT ( 'NONE',  ( -25.07950435457407323, -11.50806656539752737, -16.55003854064094426 ) ) ;
#3332 = ORIENTED_EDGE ( 'NONE', *, *, #3333, .F. ) ;
#3333 = EDGE_CURVE ( 'NONE', #540, #1715, #28315, .T. ) ;
#3334 = VECTOR ( 'NONE', #30663, 1000.000000000000000 ) ;
#3335 = EDGE_CURVE ( 'NONE', #17560, #863, #18380, .T. ) ;
#3336 = CARTESIAN_POINT ( 'NONE',  ( -11.28665222577991756, -16.53262428680031704, 18.90679857307105749 ) ) ;
#3337 = DIRECTION ( 'NONE',  ( -0.000000000000000000, -0.000000000000000000, -1.000000000000000000 ) ) ;
#3338 = FACE_OUTER_BOUND ( 'NONE', #7004, .T. ) ;
#3339 = CARTESIAN_POINT ( 'NONE',  ( 11.83189508704695214, -16.14673651688228162, 6.131018562779544823 ) ) ;
#3340 = CARTESIAN_POINT ( 'NONE',  ( 31.18700685317242716, 26.11823559933198879, -1.500000000000000000 ) ) ;
#3341 = CARTESIAN_POINT ( 'NONE',  ( -8.840471615930058036, 1.687027447297517080, 21.50000000000000000 ) ) ;
#3342 = VECTOR ( 'NONE', #12977, 1000.000000000000114 ) ;
#3343 = VERTEX_POINT ( 'NONE', #9438 ) ;
#3344 = ORIENTED_EDGE ( 'NONE', *, *, #7324, .F. ) ;
#3345 = CARTESIAN_POINT ( 'NONE',  ( 0.3563104543936100876, -6.049278984716131013, -7.522341449313008965 ) ) ;
#3346 = CARTESIAN_POINT ( 'NONE',  ( -31.18700685316100163, -26.11823559932341610, -1.500000000000000000 ) ) ;
#3347 = CARTESIAN_POINT ( 'NONE',  ( -0.2228332965694262147, -42.50627663705900261, 28.83920636888621658 ) ) ;
#3348 = CARTESIAN_POINT ( 'NONE',  ( -0.02429396239064400553, -17.02566277817059159, 6.031926333436653742 ) ) ;
#3349 = VERTEX_POINT ( 'NONE', #19556 ) ;
#3350 = CONTEXT_DEPENDENT_SHAPE_REPRESENTATION ( #24555, #18630 ) ;
#3351 = LINE ( 'NONE', #22381, #13193 ) ;
#3352 = FACE_OUTER_BOUND ( 'NONE', #30849, .T. ) ;
#3353 = AXIS2_PLACEMENT_3D ( 'NONE', #25352, #13355, #20660 ) ;
#3354 = VERTEX_POINT ( 'NONE', #9891 ) ;
#3355 = CARTESIAN_POINT ( 'NONE',  ( 37.16608720827707657, 65.00000000000000000, 15.49999999999998579 ) ) ;
#3356 = CARTESIAN_POINT ( 'NONE',  ( 23.17581250239727808, -34.50630206824672541, -1.499999999999999778 ) ) ;
#3357 = CARTESIAN_POINT ( 'NONE',  ( -32.76876142772501055, -23.05949818548782915, 34.65609885376971278 ) ) ;
#3358 = ORIENTED_EDGE ( 'NONE', *, *, #26402, .F. ) ;
#3359 = CARTESIAN_POINT ( 'NONE',  ( -4.100931858250869588, 19.90478481566557178, 1.500000000000000000 ) ) ;
#3360 = AXIS2_PLACEMENT_3D ( 'NONE', #18000, #24385, #10506 ) ;
#3361 = DIRECTION ( 'NONE',  ( -0.000000000000000000, -0.000000000000000000, 1.000000000000000000 ) ) ;
#3362 = CIRCLE ( 'NONE', #7356, 0.7500000000000006661 ) ;
#3363 = DIRECTION ( 'NONE',  ( 0.3598999890241665334, 0.9329908884337535513, 0.000000000000000000 ) ) ;
#3364 = DIRECTION ( 'NONE',  ( 0.000000000000000000, 0.000000000000000000, -1.000000000000000000 ) ) ;
#3365 = AXIS2_PLACEMENT_3D ( 'NONE', #15998, #25517, #3994 ) ;
#3366 = ORIENTED_EDGE ( 'NONE', *, *, #22090, .F. ) ;
#3367 = CARTESIAN_POINT ( 'NONE',  ( -18.20229063954115034, -8.330696590476666330, 5.701226463332907279 ) ) ;
#3368 = CARTESIAN_POINT ( 'NONE',  ( 12.69259498030721289, 11.35795912669135177, 20.22273502201483808 ) ) ;
#3369 = CARTESIAN_POINT ( 'NONE',  ( 15.57266529552203416, 38.96488032230103471, -1.500000000000000000 ) ) ;
#3370 = VECTOR ( 'NONE', #14525, 1000.000000000000114 ) ;
#3371 = FACE_OUTER_BOUND ( 'NONE', #22200, .T. ) ;
#3372 = VECTOR ( 'NONE', #28060, 1000.000000000000000 ) ;
#3373 = DIRECTION ( 'NONE',  ( -0.000000000000000000, -0.000000000000000000, 1.000000000000000000 ) ) ;
#3374 = AXIS2_PLACEMENT_3D ( 'NONE', #25137, #13303, #5658 ) ;
#3375 = CIRCLE ( 'NONE', #20798, 0.7500000000000006661 ) ;
#3377 = ADVANCED_FACE ( 'NONE', ( #216 ), #20595, .T. ) ;
#3376 = CARTESIAN_POINT ( 'NONE',  ( -38.00000000000000000, 80.00000000000000000, 15.49999999999998579 ) ) ;
#3378 = PLANE ( 'NONE',  #6557 ) ;
#3379 = FACE_BOUND ( 'NONE', #5857, .T. ) ;
#3380 = ORIENTED_EDGE ( 'NONE', *, *, #1052, .F. ) ;
#3381 = CARTESIAN_POINT ( 'NONE',  ( 35.86437274510301165, -3.536632535698085000, 34.72985588596458939 ) ) ;
#3382 = DIRECTION ( 'NONE',  ( -0.000000000000000000, -0.000000000000000000, -1.000000000000000000 ) ) ;
#3383 = VERTEX_POINT ( 'NONE', #8173 ) ;
#3384 = ORIENTED_EDGE ( 'NONE', *, *, #24867, .F. ) ;
#3385 = DIRECTION ( 'NONE',  ( 0.000000000000000000, 0.000000000000000000, -1.000000000000000000 ) ) ;
#3386 = DIRECTION ( 'NONE',  ( 1.000000000000000000, 0.000000000000000000, 0.000000000000000000 ) ) ;
#3387 = AXIS2_PLACEMENT_3D ( 'NONE', #21191, #7179, #21364 ) ;
#3388 = CARTESIAN_POINT ( 'NONE',  ( -6.651921343684833232, 49.55749932660967971, -68.45349145285689474 ) ) ;
#3389 = VECTOR ( 'NONE', #28499, 1000.000000000000000 ) ;
#3390 = CARTESIAN_POINT ( 'NONE',  ( -35.57943149391982018, 6.143871028500258902, 27.50000000000000711 ) ) ;
#3391 = CIRCLE ( 'NONE', #11875, 2.061368542273053883 ) ;
#3392 = CARTESIAN_POINT ( 'NONE',  ( 13.00026995858111079, 10.98778251907842218, 19.11611934778430921 ) ) ;
#3393 = ORIENTED_EDGE ( 'NONE', *, *, #18153, .F. ) ;
#3394 = ORIENTED_EDGE ( 'NONE', *, *, #19459, .F. ) ;
#3395 = CARTESIAN_POINT ( 'NONE',  ( -19.80066175015358354, 2.942692509523777922, 7.557577766377196582 ) ) ;
#3396 = CARTESIAN_POINT ( 'NONE',  ( 19.72466756933792809, 3.412884783584985815, 20.32367522806703874 ) ) ;
#3397 = AXIS2_PLACEMENT_3D ( 'NONE', #19127, #28495, #28795 ) ;
#3398 = CARTESIAN_POINT ( 'NONE',  ( 40.56744461766400178, 1.008925180279410139, -16.50000000000000000 ) ) ;
#3399 = ORIENTED_EDGE ( 'NONE', *, *, #6115, .T. ) ;
#3400 = VECTOR ( 'NONE', #29683, 1000.000000000000114 ) ;
#3401 = CARTESIAN_POINT ( 'NONE',  ( 0.000000000000000000, -2.435693370351110282E-15, 21.50000000000000355 ) ) ;
#3402 = ORIENTED_EDGE ( 'NONE', *, *, #5973, .T. ) ;
#3403 = DIRECTION ( 'NONE',  ( 0.000000000000000000, 1.000000000000000000, -0.000000000000000000 ) ) ;
#3404 = EDGE_LOOP ( 'NONE', ( #25073, #1401, #3581, #18257, #26796, #15185, #9678, #9859, #11224, #26072, #16671, #534, #335, #23589, #5816, #30130, #28609, #20043, #22288, #9616, #21858, #17373, #5302, #7145, #17610, #15610, #17048, #1393, #16611, #14155, #14862, #18230, #16761, #17005, #27766, #9497 ) ) ;
#3405 = FILL_AREA_STYLE_COLOUR ( '', #2264 ) ;
#3406 =( GEOMETRIC_REPRESENTATION_CONTEXT ( 3 ) GLOBAL_UNCERTAINTY_ASSIGNED_CONTEXT ( ( #6119 ) ) GLOBAL_UNIT_ASSIGNED_CONTEXT ( ( #26801, #5577, #24588 ) ) REPRESENTATION_CONTEXT ( 'NONE', 'WORKASPACE' ) );
#3407 = CYLINDRICAL_SURFACE ( 'NONE', #1649, 0.7500000000000006661 ) ;
#3408 = B_SPLINE_SURFACE_WITH_KNOTS ( 'NONE', 3, 1, ( 
 ( #23871, #28875 ),
 ( #22146, #17004 ),
 ( #26678, #16700 ),
 ( #7507, #26849 ),
 ( #26527, #5003 ),
 ( #5472, #12179 ),
 ( #2981, #2818 ),
 ( #7805, #26377 ),
 ( #12653, #21992 ),
 ( #19504, #16862 ),
 ( #12340, #771 ),
 ( #17157, #10294 ),
 ( #14663, #10141 ),
 ( #3130, #19189 ),
 ( #21842, #19808 ),
 ( #24486, #2516 ),
 ( #623, #19647 ),
 ( #29168, #26209 ),
 ( #4844, #14516 ),
 ( #14361, #21520 ),
 ( #7351, #17317 ),
 ( #24010, #22301 ),
 ( #1256, #10457 ),
 ( #20275, #29802 ),
 ( #22759, #13269 ),
 ( #24641, #25263 ),
 ( #15590, #8274 ),
 ( #5935, #10611 ),
 ( #8445, #11074 ),
 ( #13114, #20122 ),
 ( #27148, #17951 ) ),
 .UNSPECIFIED., .F., .F., .F.,
 ( 4, 3, 3, 3, 3, 3, 3, 3, 3, 3, 4 ),
 ( 2, 2 ),
 ( 0.000000000000000000, 0.05425176834609633791, 0.1085332949128352958, 0.1623767749169382768, 0.2157504826133063158, 0.2688657508888171455, 0.3218907763505476360, 0.3749548578363336993, 0.4282048033836242107, 0.4818374082110501444, 0.4999999999131656825 ),
 ( 0.000000000000000000, 1.000000000000000000 ),
 .UNSPECIFIED. ) ;
#3409 = CARTESIAN_POINT ( 'NONE',  ( 19.66622914841314085, 3.734651121118246042, 5.810767894563978686 ) ) ;
#3410 = CARTESIAN_POINT ( 'NONE',  ( -25.64627119138473788, 23.40052582045089480, -16.50000000000000000 ) ) ;
#3411 = AXIS2_PLACEMENT_3D ( 'NONE', #19597, #27554, #27238 ) ;
#3412 = CARTESIAN_POINT ( 'NONE',  ( -10.46366670609033633, -17.06541516851461893, 20.34789198813115263 ) ) ;
#3413 = CARTESIAN_POINT ( 'NONE',  ( -70.00000000000000000, -50.00000000000000000, 12.49999999999999112 ) ) ;
#3414 = CARTESIAN_POINT ( 'NONE',  ( 9.958038337755681368, 17.34466697471553331, 24.50000000000000000 ) ) ;
#3415 = DIRECTION ( 'NONE',  ( 1.000000000000000000, 0.000000000000000000, 0.000000000000000000 ) ) ;
#3416 = VERTEX_POINT ( 'NONE', #5830 ) ;
#3417 = CARTESIAN_POINT ( 'NONE',  ( 10.25620417238948434, -17.19090129355371843, 6.641371103590088865 ) ) ;
#3418 = CARTESIAN_POINT ( 'NONE',  ( 11.30587609449920272, -16.51930395566530407, 18.37415474056476938 ) ) ;
#3419 = CIRCLE ( 'NONE', #5405, 0.7500000000000006661 ) ;
#3420 = CARTESIAN_POINT ( 'NONE',  ( 0.7083562926195153819, -9.056472324687609543, -1.500000000000002887 ) ) ;
#3421 = ORIENTED_EDGE ( 'NONE', *, *, #25207, .F. ) ;
#3422 = ORIENTED_EDGE ( 'NONE', *, *, #23671, .T. ) ;
#3423 = CARTESIAN_POINT ( 'NONE',  ( 18.33599632111990374, -7.986941774664180649, 20.34789198813115263 ) ) ;
#3424 = CARTESIAN_POINT ( 'NONE',  ( 8.260402557893151254, 8.184276679720483116, 1.500000000000000000 ) ) ;
#3425 = CARTESIAN_POINT ( 'NONE',  ( -12.86767874445213877, -1.850092897552710225, 1.500000000000001332 ) ) ;
#3426 = ORIENTED_EDGE ( 'NONE', *, *, #25169, .F. ) ;
#3427 = DIRECTION ( 'NONE',  ( -0.000000000000000000, 1.000000000000000000, -0.000000000000000000 ) ) ;
#3428 = CARTESIAN_POINT ( 'NONE',  ( -37.99999999999999289, 90.00000000000001421, -69.49999999999998579 ) ) ;
#3429 = DIRECTION ( 'NONE',  ( 0.000000000000000000, 0.000000000000000000, 1.000000000000000000 ) ) ;
#3430 = AXIS2_PLACEMENT_3D ( 'NONE', #4613, #4152, #14261 ) ;
#3431 = ORIENTED_EDGE ( 'NONE', *, *, #17583, .T. ) ;
#3432 = MANIFOLD_SOLID_BREP ( 'Fillet1', #26783 ) ;
#3433 = DIRECTION ( 'NONE',  ( -1.000000000000000000, 0.000000000000000000, 0.000000000000000000 ) ) ;
#3434 = VECTOR ( 'NONE', #28812, 1000.000000000000000 ) ;
#3435 = FACE_OUTER_BOUND ( 'NONE', #2408, .T. ) ;
#3436 = CARTESIAN_POINT ( 'NONE',  ( 19.86411046155384952, 2.477959627222518613, 7.359006845440219102 ) ) ;
#3437 = ORIENTED_EDGE ( 'NONE', *, *, #3078, .F. ) ;
#3438 = DIRECTION ( 'NONE',  ( 0.000000000000000000, 0.000000000000000000, 1.000000000000000000 ) ) ;
#3439 = EDGE_LOOP ( 'NONE', ( #6605, #15249, #21286, #2969 ) ) ;
#3440 = CARTESIAN_POINT ( 'NONE',  ( 3.469446951953614189E-15, 30.50000000000000000, 24.50000000000000000 ) ) ;
#3441 = DIRECTION ( 'NONE',  ( 0.000000000000000000, 1.132880637372608986E-16, -1.000000000000000000 ) ) ;
#3442 = AXIS2_PLACEMENT_3D ( 'NONE', #1815, #20675, #30495 ) ;
#3443 = ORIENTED_EDGE ( 'NONE', *, *, #953, .F. ) ;
#3444 = EDGE_CURVE ( 'NONE', #23323, #8258, #3030, .T. ) ;
#3445 = CARTESIAN_POINT ( 'NONE',  ( 4.690664460087337950, 19.46058373524397922, 7.441806358946449151 ) ) ;
#3446 = ADVANCED_FACE ( 'NONE', ( #22042 ), #5519, .T. ) ;
#3447 = CARTESIAN_POINT ( 'NONE',  ( -26.80246859415415273, -7.028748154183637631, -1.499999999999999556 ) ) ;
#3448 = B_SPLINE_CURVE_WITH_KNOTS ( 'NONE', 3,
 ( #12587, #5706, #29268, #1339, #8061, #17565, #26938, #15366, #27548, #15056, #6174, #15201, #10857, #10397, #7911, #24727 ),
 .UNSPECIFIED., .F., .F.,
 ( 4, 2, 2, 2, 2, 2, 2, 4 ),
 ( 0.5000000000000000000, 0.6250000000000004441, 0.6875000000000007772, 0.7187500000000008882, 0.7500000000000009992, 0.8125000000000007772, 0.8750000000000005551, 1.000000000000000000 ),
 .UNSPECIFIED. ) ;
#3449 = CARTESIAN_POINT ( 'NONE',  ( 7.488956955540398752, 5.141690706682901180, 21.50000000000000000 ) ) ;
#3450 = VECTOR ( 'NONE', #17861, 1000.000000000000000 ) ;
#3451 = EDGE_CURVE ( 'NONE', #15220, #21044, #12860, .T. ) ;
#3452 = LINE ( 'NONE', #958, #4921 ) ;
#3453 = DIRECTION ( 'NONE',  ( -0.000000000000000000, -0.000000000000000000, -1.000000000000000000 ) ) ;
#3454 = EDGE_CURVE ( 'NONE', #16680, #16446, #9263, .T. ) ;
#3455 = CARTESIAN_POINT ( 'NONE',  ( 31.79204601741444947, 14.90874471747209107, 39.88609648712689904 ) ) ;
#3456 = EDGE_LOOP ( 'NONE', ( #12164, #17444, #17665, #3705 ) ) ;
#3457 = ADVANCED_FACE ( 'NONE', ( #8025 ), #27584, .T. ) ;
#3458 = CARTESIAN_POINT ( 'NONE',  ( 6.301234758012599357, -6.543385983536367689, 13.22130136205108819 ) ) ;
#3459 = VECTOR ( 'NONE', #29508, 1000.000000000000000 ) ;
#3460 = CARTESIAN_POINT ( 'NONE',  ( -15.92677741484700071, 12.12620433921149399, 19.79423548914561692 ) ) ;
#3461 = DIRECTION ( 'NONE',  ( 0.000000000000000000, -0.000000000000000000, -1.000000000000000000 ) ) ;
#3462 = DIRECTION ( 'NONE',  ( 0.000000000000000000, 0.000000000000000000, 1.000000000000000000 ) ) ;
#3463 = ORIENTED_EDGE ( 'NONE', *, *, #5222, .F. ) ;
#3465 = EDGE_CURVE ( 'NONE', #8846, #28935, #25201, .T. ) ;
#3464 = DIRECTION ( 'NONE',  ( 1.000000000000000000, 0.000000000000000000, 0.000000000000000000 ) ) ;
#3466 = CARTESIAN_POINT ( 'NONE',  ( -24.02316098943739675, -13.21662147465773707, 47.58119960047616814 ) ) ;
#3467 = PLANE ( 'NONE',  #17748 ) ;
#3468 = DIRECTION ( 'NONE',  ( -0.000000000000000000, 0.000000000000000000, 1.000000000000000000 ) ) ;
#3469 = AXIS2_PLACEMENT_3D ( 'NONE', #3779, #22794, #16088 ) ;
#3470 = EDGE_CURVE ( 'NONE', #20725, #4577, #2283, .T. ) ;
#3471 = DIRECTION ( 'NONE',  ( 1.000000000000000000, 0.000000000000000000, 0.000000000000000000 ) ) ;
#3472 = EDGE_CURVE ( 'NONE', #5139, #19648, #29859, .T. ) ;
#3473 = CARTESIAN_POINT ( 'NONE',  ( 10.34195653711237739, 41.08375821880306233, 34.57657180301586664 ) ) ;
#3474 = ORIENTED_EDGE ( 'NONE', *, *, #4046, .T. ) ;
#3475 = AXIS2_PLACEMENT_3D ( 'NONE', #20573, #2015, #30548 ) ;
#3476 = CARTESIAN_POINT ( 'NONE',  ( -3.662523238938586001, -12.47340865698848056, 1.500000000000001332 ) ) ;
#3477 = ORIENTED_EDGE ( 'NONE', *, *, #25581, .T. ) ;
#3478 = FACE_OUTER_BOUND ( 'NONE', #11529, .T. ) ;
#3479 = FACE_OUTER_BOUND ( 'NONE', #22300, .T. ) ;
#3480 = ORIENTED_EDGE ( 'NONE', *, *, #26926, .T. ) ;
#3481 = ORIENTED_EDGE ( 'NONE', *, *, #29812, .F. ) ;
#3482 = CARTESIAN_POINT ( 'NONE',  ( 24.03057240117690441, -26.57182937991349903, 1.500000000000001332 ) ) ;
#3483 = DIRECTION ( 'NONE',  ( -1.000000000000000000, -0.000000000000000000, -0.000000000000000000 ) ) ;
#3484 = EDGE_LOOP ( 'NONE', ( #27494, #3612, #15011, #16440 ) ) ;
#3485 = FACE_OUTER_BOUND ( 'NONE', #4334, .T. ) ;
#3486 = EDGE_CURVE ( 'NONE', #15921, #14016, #18002, .T. ) ;
#3487 = CARTESIAN_POINT ( 'NONE',  ( 1.000000000000008438, 13.00000000000001421, 1.500000000000001332 ) ) ;
#3488 = EDGE_CURVE ( 'NONE', #19482, #29057, #16717, .T. ) ;
#3489 = CARTESIAN_POINT ( 'NONE',  ( 25.48568755041062417, 12.36160011285428872, 1.500000000000000000 ) ) ;
#3490 = EDGE_CURVE ( 'NONE', #12630, #30261, #7258, .T. ) ;
#3491 = CARTESIAN_POINT ( 'NONE',  ( 1.492780340587499928E-15, -12.18947652193949693, 27.94260272410217638 ) ) ;
#3492 = PRESENTATION_LAYER_ASSIGNMENT (  '', '', ( #27897 ) ) ;
#3493 = CARTESIAN_POINT ( 'NONE',  ( -26.36764545593177544, -31.31467416275353344, 1.500000000000000000 ) ) ;
#3494 = EDGE_CURVE ( 'NONE', #21278, #4066, #5448, .T. ) ;
#3495 = CARTESIAN_POINT ( 'NONE',  ( -11.25351117620538943, -16.53363456493219630, 6.144783687052517429 ) ) ;
#3496 = DIRECTION ( 'NONE',  ( 0.000000000000000000, 0.000000000000000000, -1.000000000000000000 ) ) ;
#3497 = CARTESIAN_POINT ( 'NONE',  ( 11.99367014178016255, 12.13468339478709623, 20.19593175699879595 ) ) ;
#3498 = FACE_OUTER_BOUND ( 'NONE', #18843, .T. ) ;
#3499 = VERTEX_POINT ( 'NONE', #19777 ) ;
#3500 = EDGE_CURVE ( 'NONE', #10117, #26490, #26497, .T. ) ;
#3501 = AXIS2_PLACEMENT_3D ( 'NONE', #13064, #22553, #25054 ) ;
#3502 = CARTESIAN_POINT ( 'NONE',  ( -9.011666854301582319, -14.45189732017202289, 20.19668224736330941 ) ) ;
#3503 = CARTESIAN_POINT ( 'NONE',  ( 3.648422002868280778, 32.24090100849873863, 28.87075318537527480 ) ) ;
#3504 = ADVANCED_FACE ( 'NONE', ( #5284 ), #2632, .F. ) ;
#3505 = CARTESIAN_POINT ( 'NONE',  ( -4.697473163530037077, 16.36296782919469806, 7.156916968540302904 ) ) ;
#3506 = EDGE_CURVE ( 'NONE', #28205, #11519, #20211, .T. ) ;
#3507 = DIRECTION ( 'NONE',  ( -1.000000000000000000, 0.000000000000000000, 0.000000000000000000 ) ) ;
#3508 = CARTESIAN_POINT ( 'NONE',  ( -32.28307784207223108, 8.475829241206282560, 37.38016955275591613 ) ) ;
#3509 = EDGE_LOOP ( 'NONE', ( #9046, #22635 ) ) ;
#3510 = ORIENTED_EDGE ( 'NONE', *, *, #19853, .F. ) ;
#3511 = CARTESIAN_POINT ( 'NONE',  ( 14.88222593340885958, 13.36111339922579155, 7.652108011868850035 ) ) ;
#3512 = CARTESIAN_POINT ( 'NONE',  ( 5.374868878254059013, -44.10336124695543703, -19.50000000000000355 ) ) ;
#3513 = CARTESIAN_POINT ( 'NONE',  ( -15.13937296497744356, 13.09668952202108905, 5.701226463332907279 ) ) ;
#3514 = CARTESIAN_POINT ( 'NONE',  ( 127.5000000000000000, 0.000000000000000000, 5.035999999999999588 ) ) ;
#3515 = ORIENTED_EDGE ( 'NONE', *, *, #2115, .F. ) ;
#3516 = CONTEXT_DEPENDENT_SHAPE_REPRESENTATION ( #12584, #7443 ) ;
#3517 = AXIS2_PLACEMENT_3D ( 'NONE', #29672, #17356, #13147 ) ;
#3518 = CARTESIAN_POINT ( 'NONE',  ( 3.262081159888216675, 16.75658363656790328, 6.037360021877313798 ) ) ;
#3519 = CARTESIAN_POINT ( 'NONE',  ( -35.76344986165604212, -22.29344514668547461, -19.50000000000000355 ) ) ;
#3520 = EDGE_CURVE ( 'NONE', #20845, #19924, #5128, .T. ) ;
#3521 = ORIENTED_EDGE ( 'NONE', *, *, #9530, .T. ) ;
#3522 = DIRECTION ( 'NONE',  ( -0.000000000000000000, -0.000000000000000000, 1.000000000000000000 ) ) ;
#3523 = ADVANCED_FACE ( 'NONE', ( #26824 ), #18689, .F. ) ;
#3524 = FACE_OUTER_BOUND ( 'NONE', #10803, .T. ) ;
#3525 = CARTESIAN_POINT ( 'NONE',  ( -18.69039966852829693, -32.51582865032699488, 37.49999999996209255 ) ) ;
#3526 = VERTEX_POINT ( 'NONE', #7325 ) ;
#3527 = CARTESIAN_POINT ( 'NONE',  ( 11.83518757993566339, -16.12237520560631765, 6.149077423860702218 ) ) ;
#3528 = FACE_BOUND ( 'NONE', #12397, .T. ) ;
#3529 = CARTESIAN_POINT ( 'NONE',  ( -19.72722132040463094, 3.293256439147196790, 18.72886616302735163 ) ) ;
#3530 = VERTEX_POINT ( 'NONE', #12310 ) ;
#3531 = CARTESIAN_POINT ( 'NONE',  ( -4.163336342344337027E-14, 1.387778780781445676E-14, 1.500000000000000000 ) ) ;
#3532 = CARTESIAN_POINT ( 'NONE',  ( 30.50204315964899493, 15.53056155674292071, 36.52918211141452787 ) ) ;
#3533 = CARTESIAN_POINT ( 'NONE',  ( -4.375757216953428294E-15, -39.50000000000000000, 27.50000000000000355 ) ) ;
#3534 = LINE ( 'NONE', #13198, #25242 ) ;
#3535 = CIRCLE ( 'NONE', #10496, 1.000000000000004441 ) ;
#3536 = CARTESIAN_POINT ( 'NONE',  ( -17.06581907267832321, 0.6464955982388042033, 6.521906765011496354 ) ) ;
#3537 = CARTESIAN_POINT ( 'NONE',  ( 7.548823014270642950, -5.738360882149975417, 1.500000000000001332 ) ) ;
#3538 = CARTESIAN_POINT ( 'NONE',  ( 49.99999999999998579, 90.00000000000001421, -75.50000000000001421 ) ) ;
#3539 = CARTESIAN_POINT ( 'NONE',  ( 4.608906612435600181, 7.730328572437758616, -3.621320343559650379 ) ) ;
#3540 = CARTESIAN_POINT ( 'NONE',  ( 32.44949699048085989, -8.540025205420066712, 41.44554437670149127 ) ) ;
#3541 = CARTESIAN_POINT ( 'NONE',  ( -8.661893131430954185, -14.67663382381789816, 20.34789198813115618 ) ) ;
#3542 = EDGE_LOOP ( 'NONE', ( #28191, #26156, #18227, #7416, #17416 ) ) ;
#3543 = VERTEX_POINT ( 'NONE', #10112 ) ;
#3544 = CARTESIAN_POINT ( 'NONE',  ( -35.76344986165604212, -22.29344514668547461, -19.50000000000000355 ) ) ;
#3545 = CYLINDRICAL_SURFACE ( 'NONE', #26347, 0.7500000000000004441 ) ;
#3546 = ORIENTED_EDGE ( 'NONE', *, *, #29235, .T. ) ;
#3547 = CARTESIAN_POINT ( 'NONE',  ( -35.00000000000000000, 70.00000000000000000, -22.50000000000003908 ) ) ;
#3548 = DIRECTION ( 'NONE',  ( 0.000000000000000000, 0.000000000000000000, 1.000000000000000000 ) ) ;
#3549 = ADVANCED_FACE ( 'NONE', ( #21815 ), #24829, .T. ) ;
#3550 = ORIENTED_EDGE ( 'NONE', *, *, #30763, .T. ) ;
#3551 = ORIENTED_EDGE ( 'NONE', *, *, #4438, .T. ) ;
#3552 = CARTESIAN_POINT ( 'NONE',  ( -16.83923888061477925, 2.503175730361749896, 7.176035686813569292 ) ) ;
#3553 = CARTESIAN_POINT ( 'NONE',  ( -8.303920738747237351, -3.683253992019803746, 21.50000000000000000 ) ) ;
#3554 = VECTOR ( 'NONE', #5605, 1000.000000000000000 ) ;
#3555 = CARTESIAN_POINT ( 'NONE',  ( -8.579043560828049308, -14.72784502467622936, 18.34777357837151968 ) ) ;
#3556 = FACE_BOUND ( 'NONE', #28413, .T. ) ;
#3557 = VERTEX_POINT ( 'NONE', #13406 ) ;
#3558 = FACE_OUTER_BOUND ( 'NONE', #4510, .T. ) ;
#3559 = ORIENTED_EDGE ( 'NONE', *, *, #3500, .F. ) ;
#3560 = CARTESIAN_POINT ( 'NONE',  ( 8.999114229549594057, -0.1262659238204522361, 21.50000000000000000 ) ) ;
#3561 = ORIENTED_EDGE ( 'NONE', *, *, #9780, .F. ) ;
#3562 = LINE ( 'NONE', #7945, #13243 ) ;
#3563 = CARTESIAN_POINT ( 'NONE',  ( 8.890978711956464053, -41.40418588057009686, 28.93512758870527790 ) ) ;
#3564 = CARTESIAN_POINT ( 'NONE',  ( 19.68627777834516124, 3.628879393376895024, 7.559636331181775581 ) ) ;
#3565 = FACE_OUTER_BOUND ( 'NONE', #17971, .T. ) ;
#3566 = CARTESIAN_POINT ( 'NONE',  ( 1.743352590880599795, -16.98718212385438520, 6.329955581934035180 ) ) ;
#3567 = CARTESIAN_POINT ( 'NONE',  ( -40.00000000000002842, 80.00000000000001421, 47.50000000000014921 ) ) ;
#3568 = CARTESIAN_POINT ( 'NONE',  ( -15.57266529552203416, 38.96488032230103471, 1.500000000000000000 ) ) ;
#3569 = FACE_BOUND ( 'NONE', #20676, .T. ) ;
#3570 = EDGE_LOOP ( 'NONE', ( #14317, #13434, #22569, #18053 ) ) ;
#3571 = DIRECTION ( 'NONE',  ( -1.000000000000000000, 0.000000000000000000, 0.000000000000000000 ) ) ;
#3572 = ADVANCED_BREP_SHAPE_REPRESENTATION ( '', ( #2927, #7396 ), #10404 ) ;
#3573 = CARTESIAN_POINT ( 'NONE',  ( 10.31307689846358144, -13.59231953480259314, 18.50655187082627862 ) ) ;
#3574 = AXIS2_PLACEMENT_3D ( 'NONE', #3838, #20518, #15205 ) ;
#3575 = CARTESIAN_POINT ( 'NONE',  ( 0.7220001660362483920, 9.454746441592963180, 13.00000000000000178 ) ) ;
#3576 = VERTEX_POINT ( 'NONE', #13244 ) ;
#3577 = ORIENTED_EDGE ( 'NONE', *, *, #8074, .T. ) ;
#3578 = CARTESIAN_POINT ( 'NONE',  ( 43.00084836024851143, 68.73816704320454107, 12.95563330655122769 ) ) ;
#3579 = DIRECTION ( 'NONE',  ( 0.000000000000000000, 0.000000000000000000, 1.000000000000000000 ) ) ;
#3580 = CARTESIAN_POINT ( 'NONE',  ( -33.16313691975489064, -7.028748154183637631, -1.500000000000000000 ) ) ;
#3581 = ORIENTED_EDGE ( 'NONE', *, *, #15915, .F. ) ;
#3582 = DIRECTION ( 'NONE',  ( -1.000000000000000000, -0.000000000000000000, -0.000000000000000000 ) ) ;
#3583 = DIRECTION ( 'NONE',  ( 0.000000000000000000, -0.000000000000000000, -1.000000000000000000 ) ) ;
#3584 = CARTESIAN_POINT ( 'NONE',  ( 6.262360769054548193, 18.99428434097457341, 6.781503518395073371 ) ) ;
#3585 = ORIENTED_EDGE ( 'NONE', *, *, #24255, .F. ) ;
#3586 = VECTOR ( 'NONE', #6850, 1000.000000000000000 ) ;
#3587 = DIRECTION ( 'NONE',  ( 0.000000000000000000, 0.000000000000000000, -1.000000000000000000 ) ) ;
#3588 = CARTESIAN_POINT ( 'NONE',  ( 0.000000000000000000, 5.590849009245238754, -1.500000000000000000 ) ) ;
#3589 = LINE ( 'NONE', #5627, #4488 ) ;
#3590 = VERTEX_POINT ( 'NONE', #27740 ) ;
#3591 = CARTESIAN_POINT ( 'NONE',  ( -1.073881485057447405, -0.9711784013058452070, -1.500000000000000000 ) ) ;
#3592 = ORIENTED_EDGE ( 'NONE', *, *, #3131, .F. ) ;
#3593 = FACE_OUTER_BOUND ( 'NONE', #29538, .T. ) ;
#3594 = CYLINDRICAL_SURFACE ( 'NONE', #29842, 5.000000000000004441 ) ;
#3595 = CIRCLE ( 'NONE', #10069, 1.000000000000007772 ) ;
#3596 = ORIENTED_EDGE ( 'NONE', *, *, #7636, .F. ) ;
#3597 = VERTEX_POINT ( 'NONE', #22890 ) ;
#3598 = CARTESIAN_POINT ( 'NONE',  ( 3.146565092309296929, 16.78275473100424264, 6.233981582756856987 ) ) ;
#3599 = DIRECTION ( 'NONE',  ( 0.000000000000000000, 0.000000000000000000, 1.000000000000000000 ) ) ;
#3600 = CARTESIAN_POINT ( 'NONE',  ( 5.783356563690329466, 19.14595685992715346, 20.22277707861861984 ) ) ;
#3601 = APPLICATION_CONTEXT ( 'automotive_design' ) ;
#3602 = CARTESIAN_POINT ( 'NONE',  ( -31.18890335284658732, 19.89223002944919116, 34.80090346875805096 ) ) ;
#3603 = CARTESIAN_POINT ( 'NONE',  ( 10.83635815962788129, -16.83143582838889074, 18.39701043959520987 ) ) ;
#3604 = CARTESIAN_POINT ( 'NONE',  ( 22.94541271837968566, 35.03073867843525591, -6.499999999999999112 ) ) ;
#3605 = ORIENTED_EDGE ( 'NONE', *, *, #27343, .T. ) ;
#3606 = AXIS2_PLACEMENT_3D ( 'NONE', #16561, #16417, #28123 ) ;
#3607 = DIRECTION ( 'NONE',  ( 1.000000000000000000, 0.000000000000000000, 0.000000000000000000 ) ) ;
#3608 = CARTESIAN_POINT ( 'NONE',  ( 17.94577521512061580, -8.869393445417760091, 6.974106381145714018 ) ) ;
#3609 = CARTESIAN_POINT ( 'NONE',  ( -15.70110224921265818, 12.41706793386162211, 18.50655187082627862 ) ) ;
#3610 = LINE ( 'NONE', #17812, #3342 ) ;
#3611 = EDGE_LOOP ( 'NONE', ( #18236, #15064, #11627, #15783 ) ) ;
#3612 = ORIENTED_EDGE ( 'NONE', *, *, #4449, .F. ) ;
#3613 = DIRECTION ( 'NONE',  ( -0.000000000000000000, -0.000000000000000000, 1.000000000000000000 ) ) ;
#3614 = CARTESIAN_POINT ( 'NONE',  ( 2.516121109503181241, 8.728722367416590799, 21.50000000000000000 ) ) ;
#3615 = CARTESIAN_POINT ( 'NONE',  ( -4.596254364928607394, 16.38944764646977603, 19.56050940960062690 ) ) ;
#3616 = SURFACE_STYLE_USAGE ( .BOTH. , #5496 ) ;
#3617 = LINE ( 'NONE', #3303, #2171 ) ;
#3618 = EDGE_CURVE ( 'NONE', #26330, #27411, #29134, .T. ) ;
#3619 = CARTESIAN_POINT ( 'NONE',  ( 39.99999999999998579, 80.00000000000001421, 57.49999999999998579 ) ) ;
#3620 = CARTESIAN_POINT ( 'NONE',  ( 18.96813378833590846, 37.14367329901003245, 34.51897858957566001 ) ) ;
#3621 = PRODUCT_DEFINITION ( 'UNKNOWN', '', #23831, #30100 ) ;
#3622 = ORIENTED_EDGE ( 'NONE', *, *, #15918, .T. ) ;
#3623 = AXIS2_PLACEMENT_3D ( 'NONE', #3476, #13145, #24840 ) ;
#3624 = DIRECTION ( 'NONE',  ( -0.000000000000000000, -0.000000000000000000, -1.000000000000000000 ) ) ;
#3625 = CARTESIAN_POINT ( 'NONE',  ( 32.19782014694307293, 14.25394737442116444, 39.78814634291936159 ) ) ;
#3626 = CARTESIAN_POINT ( 'NONE',  ( 25.07950435457407323, -11.50806656539753270, -16.55003854064094426 ) ) ;
#3627 = EDGE_LOOP ( 'NONE', ( #25027, #11175, #18096, #17252 ) ) ;
#3628 = AXIS2_PLACEMENT_3D ( 'NONE', #19070, #9558, #28590 ) ;
#3629 = VECTOR ( 'NONE', #13122, 1000.000000000000000 ) ;
#3630 = ORIENTED_EDGE ( 'NONE', *, *, #14923, .T. ) ;
#3631 = CARTESIAN_POINT ( 'NONE',  ( -40.00000000000002842, 80.00000000000001421, 22.49999999999983302 ) ) ;
#3632 = EDGE_CURVE ( 'NONE', #17044, #7581, #5794, .T. ) ;
#3633 = AXIS2_PLACEMENT_3D ( 'NONE', #26985, #5610, #15106 ) ;
#3634 = B_SPLINE_CURVE_WITH_KNOTS ( 'NONE', 3,
 ( #20918, #9082, #18600, #6732, #1296, #3791, #10810, #20324, #28414, #25763, #9387, #19196, #18905, #19, #4544, #11571, #23878, #18743, #11887, #2049, #14051, #4394, #30588, #7039, #14944, #4853, #14201, #23557, #12034, #24454, #21211, #11720, #21527, #21382, #30741, #13913, #9227, #16706, #9685, #28721, #28259, #19048, #2203, #2521, #16547, #26066, #16400, #4697, #3098, #23709, #14369, #166, #25915, #7774, #6885, #21065, #12616, #9532, #5441, #17283, #2358, #22109, #28565, #7194, #26216, #26815, #19769, #738 ),
 .UNSPECIFIED., .F., .F.,
 ( 4, 2, 2, 2, 2, 2, 2, 2, 2, 2, 2, 2, 2, 2, 2, 2, 2, 2, 2, 2, 2, 2, 2, 2, 2, 2, 2, 2, 2, 2, 2, 2, 2, 4 ),
 ( 0.000000000000000000, 0.007385865967851777160, 0.01107879895177766617, 0.01477173193570355432, 0.02215759790355534276, 0.02400406439551829724, 0.02585053088748124478, 0.02954346387140714680, 0.03323639685533304883, 0.03508286334729599637, 0.03692932983925895085, 0.04431519580711074102, 0.04616166229907370244, 0.04800812879103664998, 0.05170106177496255201, 0.05908692774281434912, 0.06093339423477729666, 0.06277986072674023033, 0.06647279371066613929, 0.07385865967851792946, 0.07570512617048090476, 0.07755159266244385230, 0.08124452564636976126, 0.08863039161422160694, 0.09047685810618456836, 0.09232332459814752978, 0.09601625758207343875, 0.09970919056599936159, 0.1015556570579623091, 0.1034021235499252567, 0.1107879895177770330, 0.1144809225017029281, 0.1163273889936658617, 0.1181738554856288231 ),
 .UNSPECIFIED. ) ;
#3635 = CARTESIAN_POINT ( 'NONE',  ( 52.16608720827707657, -36.86186943028246787, 57.49999999999999289 ) ) ;
#3636 = VERTEX_POINT ( 'NONE', #27122 ) ;
#3637 = CARTESIAN_POINT ( 'NONE',  ( -23.22298177193101765, -35.92225147532004570, -14.83329744750909995 ) ) ;
#3638 = DIRECTION ( 'NONE',  ( 0.000000000000000000, 1.000000000000000000, 0.000000000000000000 ) ) ;
#3639 = LINE ( 'NONE', #22647, #4104 ) ;
#3640 = CARTESIAN_POINT ( 'NONE',  ( -37.48217255283579874, 11.74471995787475187, 15.19832840420940734 ) ) ;
#3641 = CYLINDRICAL_SURFACE ( 'NONE', #22791, 4.999999999999997335 ) ;
#3642 = ADVANCED_FACE ( 'NONE', ( #10433 ), #22430, .F. ) ;
#3643 = CARTESIAN_POINT ( 'NONE',  ( 0.000000000000000000, -1.307826893540337417E-14, 27.94260272410217638 ) ) ;
#3644 = DIRECTION ( 'NONE',  ( -1.000000000000000000, 0.000000000000000000, 1.369518533665900065E-16 ) ) ;
#3645 = CARTESIAN_POINT ( 'NONE',  ( 12.30878326772640996, 11.79452912058117242, 20.34789198813115263 ) ) ;
#3646 = CARTESIAN_POINT ( 'NONE',  ( 2.168404344971008868E-16, 30.50000000000000000, 24.50000000000000000 ) ) ;
#3647 = VERTEX_POINT ( 'NONE', #10736 ) ;
#3648 = CARTESIAN_POINT ( 'NONE',  ( -10.98804681698542574, -16.73276138505788779, 20.19668224736330941 ) ) ;
#3649 = CARTESIAN_POINT ( 'NONE',  ( -15.16517292768934944, -7.781889190071453299, 7.652108011868850035 ) ) ;
#3650 = DIRECTION ( 'NONE',  ( 5.125319360840571077E-16, -1.000000000000000000, 0.000000000000000000 ) ) ;
#3651 = AXIS2_PLACEMENT_3D ( 'NONE', #19018, #4514, #14022 ) ;
#3652 = CARTESIAN_POINT ( 'NONE',  ( 11.48757468322166808, -16.39371511241312618, 5.749491821935610147 ) ) ;
#3653 = AXIS2_PLACEMENT_3D ( 'NONE', #26908, #17225, #5224 ) ;
#3654 = CARTESIAN_POINT ( 'NONE',  ( -9.056472324687613096, -0.7083562926194845177, -1.500000000000001776 ) ) ;
#3655 = CARTESIAN_POINT ( 'NONE',  ( -33.18396177295070260, 9.163667207889121258, 36.33144972432103970 ) ) ;
#3656 = EDGE_LOOP ( 'NONE', ( #26090, #21109, #18977, #7393 ) ) ;
#3657 = ORIENTED_EDGE ( 'NONE', *, *, #25723, .F. ) ;
#3658 = CARTESIAN_POINT ( 'NONE',  ( 0.8038475772931101826, -5.196152422707025487, -9.000000000000000000 ) ) ;
#3659 = CARTESIAN_POINT ( 'NONE',  ( 19.64114023396890829, 37.13592150528549496, -1.500000000000000000 ) ) ;
#3660 = ADVANCED_FACE ( 'NONE', ( #20244 ), #29771, .T. ) ;
#3661 = EDGE_CURVE ( 'NONE', #25063, #23409, #21716, .T. ) ;
#3663 = CARTESIAN_POINT ( 'NONE',  ( -7.548823014270604759, 5.738360882150024267, 13.00000000000000178 ) ) ;
#3662 = B_SPLINE_CURVE_WITH_KNOTS ( 'NONE', 3,
 ( #11603, #26682, #7661, #24012, #21523, #19358, #5312, #14520, #13945, #9842 ),
 .UNSPECIFIED., .F., .F.,
 ( 4, 3, 3, 4 ),
 ( -0.005033671592849668641, 0.000000000000000000, 0.005033946531780089662, 0.01006789358107974472 ),
 .UNSPECIFIED. ) ;
#3664 = EDGE_LOOP ( 'NONE', ( #19235, #27641, #25367 ) ) ;
#3665 = CARTESIAN_POINT ( 'NONE',  ( 3.113107691802094124, 16.79024107225297513, 6.329955581934033404 ) ) ;
#3666 = CARTESIAN_POINT ( 'NONE',  ( 12.56641067637329812, 40.32935944495179115, -1.500000000000000000 ) ) ;
#3667 = CARTESIAN_POINT ( 'NONE',  ( -11.37681265597469960, -16.47072995046971755, 6.641371103590088865 ) ) ;
#3668 = ADVANCED_FACE ( 'NONE', ( #11364 ), #1840, .T. ) ;
#3669 = VERTEX_POINT ( 'NONE', #2284 ) ;
#3670 = ADVANCED_FACE ( 'NONE', ( #25857 ), #4027, .F. ) ;
#3671 = B_SPLINE_SURFACE_WITH_KNOTS ( 'NONE', 3, 1, ( 
 ( #4653, #7614 ),
 ( #7467, #24129 ),
 ( #21483, #19310 ),
 ( #7305, #4797 ),
 ( #6995, #21330 ),
 ( #14776, #16966 ),
 ( #14309, #2781 ),
 ( #23825, #2474 ),
 ( #14473, #11990 ),
 ( #30846, #16817 ),
 ( #28522, #24295 ),
 ( #7153, #12295 ),
 ( #125, #19007 ),
 ( #581, #12142 ),
 ( #439, #23975 ),
 ( #9491, #16664 ),
 ( #10101, #2945 ),
 ( #23660, #28373 ),
 ( #19157, #4964 ),
 ( #16507, #2622 ),
 ( #21643, #14156 ),
 ( #278, #9797 ),
 ( #28830, #21800 ),
 ( #26485, #9955 ),
 ( #19463, #13075 ),
 ( #27105, #899 ),
 ( #10570, #1366 ),
 ( #22102, #29291 ),
 ( #5434, #29599 ),
 ( #5890, #26961 ),
 ( #29748, #27257 ) ),
 .UNSPECIFIED., .F., .F., .F.,
 ( 4, 3, 3, 3, 3, 3, 3, 3, 3, 3, 4 ),
 ( 2, 2 ),
 ( 0.4999999998345686647, 0.5360336730431939367, 0.5907651151589012883, 0.6456034593241830599, 0.6998270958050434309, 0.7529536536315937223, 0.8052385063053260073, 0.8575343587103997356, 0.9106564858195042023, 0.9648414833209685293, 1.000000006602610236 ),
 ( 0.000000000000000000, 1.000000000000000000 ),
 .UNSPECIFIED. ) ;
#3672 = VECTOR ( 'NONE', #12552, 1000.000000000000000 ) ;
#3673 = DIRECTION ( 'NONE',  ( 0.000000000000000000, 0.000000000000000000, 1.000000000000000000 ) ) ;
#3674 = CARTESIAN_POINT ( 'NONE',  ( 19.59831178344208169, 3.989367808977733354, 19.96797677718664232 ) ) ;
#3675 = ORIENTED_EDGE ( 'NONE', *, *, #6937, .F. ) ;
#3676 = ADVANCED_FACE ( 'NONE', ( #13701 ), #20857, .F. ) ;
#3677 = DIRECTION ( 'NONE',  ( -1.000000000000000000, 0.000000000000000000, 0.000000000000000000 ) ) ;
#3678 = CIRCLE ( 'NONE', #4661, 20.00000000000000000 ) ;
#3679 = EDGE_CURVE ( 'NONE', #11709, #22434, #4291, .T. ) ;
#3680 = AXIS2_PLACEMENT_3D ( 'NONE', #27292, #1407, #18087 ) ;
#3681 = DIRECTION ( 'NONE',  ( -0.3598999890241650346, 0.9329908884337541064, 0.000000000000000000 ) ) ;
#3682 = CARTESIAN_POINT ( 'NONE',  ( -3.683253992019773992, 8.303920738747248009, 21.50000000000000000 ) ) ;
#3683 = FACE_OUTER_BOUND ( 'NONE', #7046, .T. ) ;
#3684 = ORIENTED_EDGE ( 'NONE', *, *, #13760, .F. ) ;
#3685 = CARTESIAN_POINT ( 'NONE',  ( 12.35846533491530685, 11.73919094685904341, 20.34789198813115263 ) ) ;
#3686 = ADVANCED_FACE ( 'NONE', ( #30520 ), #18839, .F. ) ;
#3687 = CARTESIAN_POINT ( 'NONE',  ( -8.546423435383420752, -14.74799740001550141, 5.652196082368483587 ) ) ;
#3688 = CARTESIAN_POINT ( 'NONE',  ( -50.00000000000000000, 50.00000000000000000, 12.49999999999999112 ) ) ;
#3689 = CARTESIAN_POINT ( 'NONE',  ( -43.34097750826428097, 11.89502811014148342, -1.500000000000000444 ) ) ;
#3690 = DIRECTION ( 'NONE',  ( -1.000000000000000000, -0.000000000000000000, -0.000000000000000000 ) ) ;
#3691 = DIRECTION ( 'NONE',  ( 0.000000000000000000, 1.000000000000000000, 1.193512090021232842E-16 ) ) ;
#3692 = CARTESIAN_POINT ( 'NONE',  ( 9.999999999999959144, 1.510243460696181139E-14, 24.50000000000000000 ) ) ;
#3693 = CARTESIAN_POINT ( 'NONE',  ( 19.81789086666767119, 2.695592600026630148, 5.775318986477952166 ) ) ;
#3694 = CARTESIAN_POINT ( 'NONE',  ( 33.55224573311711822, -10.10291939066353351, 39.95985515795820930 ) ) ;
#3695 = DIRECTION ( 'NONE',  ( 4.565061778886335400E-17, 0.000000000000000000, -1.000000000000000000 ) ) ;
#3696 = EDGE_LOOP ( 'NONE', ( #28129, #2459, #12691, #30638 ) ) ;
#3697 = VERTEX_POINT ( 'NONE', #18532 ) ;
#3698 = CARTESIAN_POINT ( 'NONE',  ( 22.58267429318970443, -26.57182937991349903, 26.54355021145562787 ) ) ;
#3699 = VECTOR ( 'NONE', #21404, 1000.000000000000000 ) ;
#3700 = FACE_OUTER_BOUND ( 'NONE', #830, .T. ) ;
#3701 = ADVANCED_FACE ( 'NONE', ( #18676 ), #20697, .F. ) ;
#3702 = CARTESIAN_POINT ( 'NONE',  ( 0.07661102881317781443, 6.914460432017338398, 6.023803224821318913 ) ) ;
#3703 = CIRCLE ( 'NONE', #6670, 4.999999999999997335 ) ;
#3704 = EDGE_CURVE ( 'NONE', #8734, #15471, #6786, .T. ) ;
#3705 = ORIENTED_EDGE ( 'NONE', *, *, #14701, .T. ) ;
#3706 = SHAPE_REPRESENTATION_RELATIONSHIP ( 'NONE' , 'NONE' ,  #13696, #3572 ) ;
#3707 = DIRECTION ( 'NONE',  ( -0.000000000000000000, 1.132880637372608986E-16, -1.000000000000000000 ) ) ;
#3708 = EDGE_CURVE ( 'NONE', #17083, #8115, #14138, .T. ) ;
#3709 = DIRECTION ( 'NONE',  ( -1.000000000000000000, 0.000000000000000000, 0.000000000000000000 ) ) ;
#3710 = ORIENTED_EDGE ( 'NONE', *, *, #24779, .F. ) ;
#3711 = VERTEX_POINT ( 'NONE', #13852 ) ;
#3712 = CARTESIAN_POINT ( 'NONE',  ( -19.78525473782456601, 3.044038662852082133, 7.500898271101006820 ) ) ;
#3713 = CARTESIAN_POINT ( 'NONE',  ( 16.61573067466906650, 3.902325345048615279, 20.06253562465620632 ) ) ;
#3714 = DIRECTION ( 'NONE',  ( 1.000000000000000000, 0.000000000000000000, 0.000000000000000000 ) ) ;
#3715 = CARTESIAN_POINT ( 'NONE',  ( -10.80934979336458746, 35.92737112411883516, 37.49999999999869971 ) ) ;
#3716 = ORIENTED_EDGE ( 'NONE', *, *, #26503, .F. ) ;
#3717 = CARTESIAN_POINT ( 'NONE',  ( -5.393256883115301825, -14.81828060999315433, -0.6213203435596476032 ) ) ;
#3718 = ORIENTED_EDGE ( 'NONE', *, *, #21167, .F. ) ;
#3719 = DIRECTION ( 'NONE',  ( -0.000000000000000000, -0.000000000000000000, -1.000000000000000000 ) ) ;
#3720 = PLANE ( 'NONE',  #2365 ) ;
#3721 = EDGE_LOOP ( 'NONE', ( #8377, #22423, #28746, #15898 ) ) ;
#3722 = CIRCLE ( 'NONE', #9186, 20.00000000000000355 ) ;
#3723 = CARTESIAN_POINT ( 'NONE',  ( -15.34618031767423041, 12.82553819247484128, 18.34798005863227388 ) ) ;
#3724 = DIRECTION ( 'NONE',  ( -0.000000000000000000, -0.000000000000000000, 1.000000000000000000 ) ) ;
#3725 = CARTESIAN_POINT ( 'NONE',  ( 19.68435877536853340, 3.639270104310704745, 5.749491821935610147 ) ) ;
#3726 = DIRECTION ( 'NONE',  ( -0.000000000000000000, -0.000000000000000000, 1.000000000000000000 ) ) ;
#3727 = CARTESIAN_POINT ( 'NONE',  ( -10.33762405876901980, -17.14187335405549462, 20.32367522806703874 ) ) ;
#3728 = CARTESIAN_POINT ( 'NONE',  ( -4.937793815610304726, 6.974883619896852238, 21.50000000000000000 ) ) ;
#3729 = DIRECTION ( 'NONE',  ( 1.000000000000000000, 0.000000000000000000, 0.000000000000000000 ) ) ;
#3730 = DIRECTION ( 'NONE',  ( -1.000000000000000000, 0.000000000000000000, 0.000000000000000000 ) ) ;
#3731 = ORIENTED_EDGE ( 'NONE', *, *, #21200, .F. ) ;
#3732 = EDGE_CURVE ( 'NONE', #12560, #30628, #22769, .T. ) ;
#3733 = EDGE_CURVE ( 'NONE', #28942, #6434, #23641, .T. ) ;
#3734 = PLANE ( 'NONE',  #12264 ) ;
#3735 = CARTESIAN_POINT ( 'NONE',  ( 21.86019681245146629, -31.48592878035298170, 34.80090346875810781 ) ) ;
#3736 = ORIENTED_EDGE ( 'NONE', *, *, #15617, .T. ) ;
#3737 = ORIENTED_EDGE ( 'NONE', *, *, #11495, .T. ) ;
#3738 = CARTESIAN_POINT ( 'NONE',  ( 46.67303262113644990, 69.72284517594248143, 15.04469359926350336 ) ) ;
#3739 = DIRECTION ( 'NONE',  ( -1.000000000000000000, 0.000000000000000000, 0.000000000000000000 ) ) ;
#3740 = CARTESIAN_POINT ( 'NONE',  ( -5.369726540290508332, 19.28438192063506307, 5.862424720655265098 ) ) ;
#3741 = ORIENTED_EDGE ( 'NONE', *, *, #5727, .F. ) ;
#3742 = DIRECTION ( 'NONE',  ( 0.000000000000000000, 0.000000000000000000, -1.000000000000000000 ) ) ;
#3743 = CARTESIAN_POINT ( 'NONE',  ( -2.446529495465445958, -8.413215745754985875, -3.621320343559650379 ) ) ;
#3744 = VECTOR ( 'NONE', #4155, 1000.000000000000000 ) ;
#3745 = CARTESIAN_POINT ( 'NONE',  ( 24.14277784031759566, 13.29036922066994642, 47.44085139300341325 ) ) ;
#3746 = DIRECTION ( 'NONE',  ( -0.000000000000000000, -0.000000000000000000, 1.000000000000000000 ) ) ;
#3747 = CARTESIAN_POINT ( 'NONE',  ( 14.45824965121216010, 13.84471048730597786, 5.872146474157316831 ) ) ;
#3748 = CARTESIAN_POINT ( 'NONE',  ( -33.56830061431172396, -10.30497729095454851, 39.88583012291989149 ) ) ;
#3749 = ORIENTED_EDGE ( 'NONE', *, *, #15480, .T. ) ;
#3750 = DIRECTION ( 'NONE',  ( 0.000000000000000000, 0.000000000000000000, 1.000000000000000000 ) ) ;
#3751 = ORIENTED_EDGE ( 'NONE', *, *, #17241, .T. ) ;
#3752 = CARTESIAN_POINT ( 'NONE',  ( -3.640207617113898841, 7.856594496258241023, 21.50000000000000000 ) ) ;
#3753 = VERTEX_POINT ( 'NONE', #30223 ) ;
#3754 = ORIENTED_EDGE ( 'NONE', *, *, #20621, .T. ) ;
#3755 = CARTESIAN_POINT ( 'NONE',  ( 3.200917658998827964, 16.77053181957578332, 6.131018562779544823 ) ) ;
#3756 = DIRECTION ( 'NONE',  ( -1.000000000000000000, 0.000000000000000000, 0.000000000000000000 ) ) ;
#3757 = DIRECTION ( 'NONE',  ( 6.938893903907227392E-16, 0.000000000000000000, 1.000000000000000000 ) ) ;
#3758 = ORIENTED_EDGE ( 'NONE', *, *, #25426, .T. ) ;
#3759 =( BOUNDED_SURFACE ( )  B_SPLINE_SURFACE ( 3, 1, ( 
 ( #4545, #13914 ),
 ( #6734, #16245 ),
 ( #25916, #11431 ),
 ( #4855, #16401 ) ),
 .UNSPECIFIED., .F., .F., .T. ) 
 B_SPLINE_SURFACE_WITH_KNOTS ( ( 4, 4 ),
 ( 2, 2 ),
 ( 0.000000000000000000, 1.000000000000000000 ),
 ( 0.000000000000000000, 1.000000000000000000 ),
 .UNSPECIFIED. ) 
 GEOMETRIC_REPRESENTATION_ITEM ( )  RATIONAL_B_SPLINE_SURFACE ( (
 ( 1.000000000000000000, 1.000000000000000000),
 ( 0.3333333333333333703, 0.3333333333333333703),
 ( 0.3333333333333333703, 0.3333333333333333703),
 ( 1.000000000000000000, 1.000000000000000000) ) ) 
 REPRESENTATION_ITEM ( '' )  SURFACE ( )  );
#3760 = VECTOR ( 'NONE', #9073, 1000.000000000000227 ) ;
#3761 = CARTESIAN_POINT ( 'NONE',  ( -36.00000000000000000, 2.601438916704200466, 27.50000000000000355 ) ) ;
#3762 = CARTESIAN_POINT ( 'NONE',  ( 9.833055564703260032, -13.92194044488497084, 18.34777357837152323 ) ) ;
#3763 = CARTESIAN_POINT ( 'NONE',  ( 16.82340201860977302, 2.653416696629038007, 20.19668224736330941 ) ) ;
#3764 = VERTEX_POINT ( 'NONE', #18393 ) ;
#3765 = CARTESIAN_POINT ( 'NONE',  ( 32.28307784207223108, 8.475829241206289666, 37.38016955275583086 ) ) ;
#3766 = CARTESIAN_POINT ( 'NONE',  ( 15.38930515692759471, -7.273136567754737491, 6.530762810602277924 ) ) ;
#3767 = EDGE_CURVE ( 'NONE', #30269, #15581, #4172, .T. ) ;
#3768 = CARTESIAN_POINT ( 'NONE',  ( -15.95709955354364418, 12.08619843917606929, 6.341840715582230281 ) ) ;
#3769 = CARTESIAN_POINT ( 'NONE',  ( 4.414161002286802749, 19.52491365267160361, 19.79423548914561692 ) ) ;
#3770 = EDGE_LOOP ( 'NONE', ( #6397, #9480, #13738, #18719 ) ) ;
#3771 = VERTEX_POINT ( 'NONE', #26626 ) ;
#3772 = CARTESIAN_POINT ( 'NONE',  ( -35.00000000000000000, 90.00000000000001421, -22.50000000000002487 ) ) ;
#3773 = CARTESIAN_POINT ( 'NONE',  ( 31.56327786402390245, 10.34181101807379655, -16.55003854064094426 ) ) ;
#3774 = CARTESIAN_POINT ( 'NONE',  ( -2.703030265324078307, -12.75514121382991384, 1.500000000000001332 ) ) ;
#3775 = DIRECTION ( 'NONE',  ( -0.000000000000000000, 0.000000000000000000, 1.000000000000000000 ) ) ;
#3776 = DIRECTION ( 'NONE',  ( 0.000000000000000000, 0.000000000000000000, -1.000000000000000000 ) ) ;
#3777 = AXIS2_PLACEMENT_3D ( 'NONE', #6810, #28958, #5252 ) ;
#3778 = CARTESIAN_POINT ( 'NONE',  ( 1.000000000000008438, 16.48749217771910125, -0.6213203435596476032 ) ) ;
#3779 = CARTESIAN_POINT ( 'NONE',  ( 17.22181377297005866, 14.41708049311048789, 1.500000000000000000 ) ) ;
#3780 = ORIENTED_EDGE ( 'NONE', *, *, #9565, .T. ) ;
#3781 = PLANE ( 'NONE',  #3374 ) ;
#3782 = LINE ( 'NONE', #27643, #27161 ) ;
#3783 = FACE_OUTER_BOUND ( 'NONE', #27772, .T. ) ;
#3784 = ORIENTED_EDGE ( 'NONE', *, *, #21200, .T. ) ;
#3785 = CIRCLE ( 'NONE', #21176, 0.7499999999999988898 ) ;
#3786 = ORIENTED_EDGE ( 'NONE', *, *, #28796, .F. ) ;
#3787 = CARTESIAN_POINT ( 'NONE',  ( 9.590471615930072247, -1.687027447297460236, 21.50000000000000000 ) ) ;
#3788 = CIRCLE ( 'NONE', #9765, 37.60050224823048381 ) ;
#3789 = DIRECTION ( 'NONE',  ( 0.000000000000000000, -1.132880637372608986E-16, 1.000000000000000000 ) ) ;
#3790 = ORIENTED_EDGE ( 'NONE', *, *, #7461, .T. ) ;
#3791 = CARTESIAN_POINT ( 'NONE',  ( 12.09913007902929216, -37.22566656357093962, 27.50000000000001421 ) ) ;
#3792 = CARTESIAN_POINT ( 'NONE',  ( 11.28349294625599519, 48.71123628743529821, -64.89555161802378791 ) ) ;
#3793 = DIRECTION ( 'NONE',  ( 1.000000000000000000, 0.000000000000000000, 0.000000000000000000 ) ) ;
#3794 = DIRECTION ( 'NONE',  ( 1.000000000000000000, 0.000000000000000000, 0.000000000000000000 ) ) ;
#3795 = CARTESIAN_POINT ( 'NONE',  ( -24.03057240117690441, -26.57182937991348481, 26.54355021145563143 ) ) ;
#3796 = VECTOR ( 'NONE', #18793, 1000.000000000000000 ) ;
#3797 = CARTESIAN_POINT ( 'NONE',  ( -20.71335220384823117, -27.86167394782616213, -16.50000000000000000 ) ) ;
#3798 = CARTESIAN_POINT ( 'NONE',  ( 1.350727940147186112, -19.97202376558938752, 6.447548852708279377 ) ) ;
#3799 = EDGE_LOOP ( 'NONE', ( #20233, #10447, #19766, #14062 ) ) ;
#3800 = CARTESIAN_POINT ( 'NONE',  ( -10.97902775627723670, -16.73874854128740353, 18.49267272388512140 ) ) ;
#3801 = DIRECTION ( 'NONE',  ( -1.000000000000000000, 0.000000000000000000, -0.000000000000000000 ) ) ;
#3802 = CARTESIAN_POINT ( 'NONE',  ( -4.573988094335657451, 16.39521158297133141, 6.714907520933424578 ) ) ;
#3803 = VECTOR ( 'NONE', #4068, 1000.000000000000000 ) ;
#3804 = CARTESIAN_POINT ( 'NONE',  ( 11.23845335764779385, -16.56542118924665630, 7.643931100913408550 ) ) ;
#3805 = EDGE_CURVE ( 'NONE', #7334, #30279, #24208, .T. ) ;
#3806 = CARTESIAN_POINT ( 'NONE',  ( -2.687479363073305372, 44.39187623477332068, -19.50000000000000355 ) ) ;
#3807 = VECTOR ( 'NONE', #18243, 1000.000000000000000 ) ;
#3808 = CARTESIAN_POINT ( 'NONE',  ( 6.899999999999999467, 10.39230484541327471, 0.000000000000000000 ) ) ;
#3809 = ORIENTED_EDGE ( 'NONE', *, *, #14903, .F. ) ;
#3810 = LINE ( 'NONE', #10835, #25358 ) ;
#3811 = CARTESIAN_POINT ( 'NONE',  ( 23.96732207937828463, 33.98584080152456011, -1.500000000000000000 ) ) ;
#3812 = CARTESIAN_POINT ( 'NONE',  ( -0.2184780646694884920, -42.50603693459091659, 34.61341353021254008 ) ) ;
#3813 = CARTESIAN_POINT ( 'NONE',  ( 9.056472324687609543, 0.7083562926195455800, 21.50000000000000000 ) ) ;
#3814 = EDGE_LOOP ( 'NONE', ( #26252, #27150 ) ) ;
#3815 = FACE_OUTER_BOUND ( 'NONE', #29238, .T. ) ;
#3816 = AXIS2_PLACEMENT_3D ( 'NONE', #6664, #6522, #9022 ) ;
#3817 = CARTESIAN_POINT ( 'NONE',  ( 31.18700685317242716, 26.11823559933198879, -1.500000000000000000 ) ) ;
#3818 = CARTESIAN_POINT ( 'NONE',  ( -10.52280129341197323, -17.02885805942690567, 5.652196082367002994 ) ) ;
#3819 = AXIS2_PLACEMENT_3D ( 'NONE', #20597, #22942, #1731 ) ;
#3820 = EDGE_LOOP ( 'NONE', ( #8228, #19617, #18856, #20756, #29475, #27058 ) ) ;
#3821 = DIRECTION ( 'NONE',  ( 1.000000000000000000, 0.000000000000000000, -0.000000000000000000 ) ) ;
#3822 = CARTESIAN_POINT ( 'NONE',  ( -21.00812534432329315, -35.81422794740934279, 29.45837907140124656 ) ) ;
#3823 = VERTEX_POINT ( 'NONE', #7752 ) ;
#3824 = CARTESIAN_POINT ( 'NONE',  ( -26.81368379037234817, -6.366017791192965625, 43.19835251265433840 ) ) ;
#3825 = VECTOR ( 'NONE', #7196, 1000.000000000000000 ) ;
#3826 = AXIS2_PLACEMENT_3D ( 'NONE', #8062, #5707, #3066 ) ;
#3827 = CIRCLE ( 'NONE', #13302, 20.00000000000000000 ) ;
#3828 = CARTESIAN_POINT ( 'NONE',  ( -15.16517293421788537, -7.781889191988407006, 20.34789198813115263 ) ) ;
#3829 = CARTESIAN_POINT ( 'NONE',  ( 1.734723475976807094E-15, -44.07656352898514740, -6.500000000000000888 ) ) ;
#3830 = ORIENTED_EDGE ( 'NONE', *, *, #9612, .F. ) ;
#3831 = CARTESIAN_POINT ( 'NONE',  ( 64.99999999999998579, -36.86186943028246787, 97.07879600563551037 ) ) ;
#3832 = CARTESIAN_POINT ( 'NONE',  ( 12.88533868971568808, 11.12831076058098745, 19.96344307082653202 ) ) ;
#3833 = ADVANCED_FACE ( 'NONE', ( #12590 ), #23803, .F. ) ;
#3834 = CARTESIAN_POINT ( 'NONE',  ( 0.4897477184365084391, -19.99444548460946791, 18.34869673959212122 ) ) ;
#3835 = PLANE ( 'NONE',  #25725 ) ;
#3836 = CARTESIAN_POINT ( 'NONE',  ( -17.06384985643477847, 0.6725948717588426939, 6.392658652357120275 ) ) ;
#3837 = DIRECTION ( 'NONE',  ( 0.000000000000000000, -0.000000000000000000, 1.000000000000000000 ) ) ;
#3838 = CARTESIAN_POINT ( 'NONE',  ( 5.881244434206234217, 6.812559277181991391, 1.500000000000001332 ) ) ;
#3839 = AXIS2_PLACEMENT_3D ( 'NONE', #29893, #20367, #5557 ) ;
#3840 = DIRECTION ( 'NONE',  ( -0.000000000000000000, -0.000000000000000000, 1.000000000000000000 ) ) ;
#3841 = ADVANCED_FACE ( 'NONE', ( #416 ), #12441, .F. ) ;
#3842 = CARTESIAN_POINT ( 'NONE',  ( 9.117173258182925011, -14.37672153453698343, 7.156916968540298463 ) ) ;
#3843 = FACE_OUTER_BOUND ( 'NONE', #8490, .T. ) ;
#3844 = CARTESIAN_POINT ( 'NONE',  ( -9.228184491520634580, -14.30775539779752847, 19.96344307082651781 ) ) ;
#3845 = AXIS2_PLACEMENT_3D ( 'NONE', #29030, #10152, #7667 ) ;
#3846 = ORIENTED_EDGE ( 'NONE', *, *, #12257, .F. ) ;
#3847 = VERTEX_POINT ( 'NONE', #9627 ) ;
#3848 = CARTESIAN_POINT ( 'NONE',  ( 49.99999999999998579, -50.00000000000000000, 62.49999999999999289 ) ) ;
#3849 = DIRECTION ( 'NONE',  ( 1.000000000000000000, 0.000000000000000000, 0.000000000000000000 ) ) ;
#3850 = EDGE_CURVE ( 'NONE', #27558, #2772, #26201, .T. ) ;
#3851 = DIRECTION ( 'NONE',  ( -1.000000000000000000, 0.000000000000000000, 0.000000000000000000 ) ) ;
#3852 = ORIENTED_EDGE ( 'NONE', *, *, #5782, .F. ) ;
#3853 = CARTESIAN_POINT ( 'NONE',  ( 9.169883732660084164, -9.268939115642975679, 1.500000000000001332 ) ) ;
#3854 = EDGE_CURVE ( 'NONE', #13757, #21278, #24113, .T. ) ;
#3855 = CARTESIAN_POINT ( 'NONE',  ( 9.117173258235231614, -14.37672153450547619, 19.85270094495842130 ) ) ;
#3856 = EDGE_CURVE ( 'NONE', #23663, #21250, #2763, .T. ) ;
#3857 = VECTOR ( 'NONE', #16916, 1000.000000000000000 ) ;
#3858 = EDGE_LOOP ( 'NONE', ( #22277, #29955, #23055, #7847, #12844, #22784, #6492, #17892, #1547 ) ) ;
#3859 = ORIENTED_EDGE ( 'NONE', *, *, #19661, .T. ) ;
#3860 = CARTESIAN_POINT ( 'NONE',  ( -16.81737828845396265, 2.629481162813160022, 6.420335371522007506 ) ) ;
#3861 = VECTOR ( 'NONE', #12040, 1000.000000000000000 ) ;
#3862 = DIRECTION ( 'NONE',  ( 0.000000000000000000, -0.000000000000000000, 1.000000000000000000 ) ) ;
#3863 = AXIS2_PLACEMENT_3D ( 'NONE', #9359, #8436, #9821 ) ;
#3864 = CARTESIAN_POINT ( 'NONE',  ( 15.52007383991470135, 12.61466978257045746, 6.386539667786101937 ) ) ;
#3865 = CARTESIAN_POINT ( 'NONE',  ( -16.30640546663167356, 38.61508539432780651, 34.53478415730283757 ) ) ;
#3866 = EDGE_LOOP ( 'NONE', ( #512, #4687, #24905, #11331, #27886 ) ) ;
#3867 = CARTESIAN_POINT ( 'NONE',  ( 24.35970437652574816, -13.37404834226503958, 47.21042702067961727 ) ) ;
#3868 = ORIENTED_EDGE ( 'NONE', *, *, #1967, .F. ) ;
#3869 = CLOSED_SHELL ( 'NONE', ( #28448, #2503, #13583, #1756, #8857, #10128, #14330, #27072, #18523, #3075, #9353, #28639, #6406, #4777, #6909, #16272, #15303, #4583, #21564, #15221, #27786, #24242, #626, #1750, #15368, #25391, #20831, #21794, #15982, #23364, #9380, #8644, #8818, #20413, #8615, #9779, #23667, #27306, #5769, #29435, #25776, #12783, #18322, #8982, #7354, #30362, #5241, #3660, #17604, #1421, #24429, #721, #17780, #23893 ) ) ;
#3870 = CARTESIAN_POINT ( 'NONE',  ( -14.93254240672194122, -8.254432589262984621, 7.545655578832112909 ) ) ;
#3871 = CARTESIAN_POINT ( 'NONE',  ( -16.87879800891222359, 2.262652451654310060, 18.54473042795394733 ) ) ;
#3872 = AXIS2_PLACEMENT_3D ( 'NONE', #18899, #11257, #11880 ) ;
#3873 = ORIENTED_EDGE ( 'NONE', *, *, #2310, .F. ) ;
#3874 = TOROIDAL_SURFACE ( 'NONE', #21779, 7.000000000000000000, 3.000000000000000000 ) ;
#3875 = ADVANCED_FACE ( 'NONE', ( #5254 ), #26152, .F. ) ;
#3876 = CARTESIAN_POINT ( 'NONE',  ( -6.910239377218535317, 18.76835738875811899, 19.08830981656263859 ) ) ;
#3877 = EDGE_CURVE ( 'NONE', #26519, #8036, #4779, .T. ) ;
#3878 = CARTESIAN_POINT ( 'NONE',  ( 14.37255012589468883, -39.51473361311175125, 29.10561451833818225 ) ) ;
#3879 = CARTESIAN_POINT ( 'NONE',  ( 19.64806919293054932, 3.830191698062872074, 5.872146474157316831 ) ) ;
#3880 = VECTOR ( 'NONE', #20193, 1000.000000000000114 ) ;
#3881 = EDGE_CURVE ( 'NONE', #8417, #14704, #23959, .T. ) ;
#3882 = CARTESIAN_POINT ( 'NONE',  ( -9.736160311572513493, -17.49040459468425368, 19.79423548914561692 ) ) ;
#3883 = CARTESIAN_POINT ( 'NONE',  ( -22.58267429318970443, -26.57182937991348481, 26.54355021145562787 ) ) ;
#3884 = CARTESIAN_POINT ( 'NONE',  ( -17.02601880987613825, 1.106972870283159160, 18.50655187082627862 ) ) ;
#3885 = DIRECTION ( 'NONE',  ( 0.000000000000000000, 0.000000000000000000, -1.000000000000000000 ) ) ;
#3886 = ORIENTED_EDGE ( 'NONE', *, *, #15278, .T. ) ;
#3887 = ADVANCED_FACE ( 'NONE', ( #28653 ), #107, .T. ) ;
#3888 = CIRCLE ( 'NONE', #12866, 11.99999999999998934 ) ;
#3889 = CARTESIAN_POINT ( 'NONE',  ( -29.41946345040754096, 27.90099610680150377, 16.50653305109835500 ) ) ;
#3890 = CARTESIAN_POINT ( 'NONE',  ( 15.85884089648730289, -35.55173462727349687, 27.50000000000000355 ) ) ;
#3891 = AXIS2_PLACEMENT_3D ( 'NONE', #13671, #11016, #25361 ) ;
#3892 = ORIENTED_EDGE ( 'NONE', *, *, #24207, .T. ) ;
#3893 = ORIENTED_EDGE ( 'NONE', *, *, #3260, .F. ) ;
#3894 = CARTESIAN_POINT ( 'NONE',  ( 44.78385332603417623, 69.31632679361693761, 13.69377121817660914 ) ) ;
#3895 = CARTESIAN_POINT ( 'NONE',  ( -15.51517975927889736, 12.62116967784147548, 5.679672709359370408 ) ) ;
#3896 = ADVANCED_FACE ( 'NONE', ( #5100 ), #9935, .F. ) ;
#3897 = DIRECTION ( 'NONE',  ( -1.000000000000000000, 0.000000000000000000, 0.000000000000000000 ) ) ;
#3898 = EDGE_LOOP ( 'NONE', ( #13946, #30541, #21181, #4474, #3077, #19175 ) ) ;
#3899 = LINE ( 'NONE', #25099, #23576 ) ;
#3900 = AXIS2_PLACEMENT_3D ( 'NONE', #250, #16941, #19584 ) ;
#3901 = CARTESIAN_POINT ( 'NONE',  ( -12.85122823565992789, 11.16779817455389434, 6.031926333436658183 ) ) ;
#3902 = AXIS2_PLACEMENT_3D ( 'NONE', #15016, #5981, #23416 ) ;
#3903 = LINE ( 'NONE', #13426, #10959 ) ;
#3904 = VERTEX_POINT ( 'NONE', #19594 ) ;
#3905 = LINE ( 'NONE', #11674, #2799 ) ;
#3906 = CARTESIAN_POINT ( 'NONE',  ( -4.390207617113899730, 7.856594496258241023, -1.500000000000000888 ) ) ;
#3907 = ORIENTED_EDGE ( 'NONE', *, *, #7057, .F. ) ;
#3908 = DIRECTION ( 'NONE',  ( 1.000000000000000000, 0.000000000000000000, 0.000000000000000000 ) ) ;
#3909 = EDGE_LOOP ( 'NONE', ( #753, #20312, #1916, #931 ) ) ;
#3910 = VECTOR ( 'NONE', #17305, 1000.000000000000000 ) ;
#3911 = EDGE_CURVE ( 'NONE', #18592, #5755, #29213, .T. ) ;
#3912 = FACE_OUTER_BOUND ( 'NONE', #27376, .T. ) ;
#3913 = PRODUCT_DEFINITION_CONTEXT ( 'detailed design', #26935, 'design' ) ;
#3914 = CIRCLE ( 'NONE', #20355, 1.000000000000008438 ) ;
#3915 = EDGE_CURVE ( 'NONE', #26574, #5509, #26442, .T. ) ;
#3916 = ORIENTED_EDGE ( 'NONE', *, *, #22807, .T. ) ;
#3917 = ORIENTED_EDGE ( 'NONE', *, *, #6315, .F. ) ;
#3918 = B_SPLINE_CURVE_WITH_KNOTS ( 'NONE', 3,
 ( #25303, #13904, #23406, #3948, #25906, #30129, #30581, #11422, #20911, #30434, #20753, #9220, #9074, #8759, #6877, #4536, #23868, #476 ),
 .UNSPECIFIED., .F., .F.,
 ( 4, 2, 2, 2, 2, 2, 2, 2, 4 ),
 ( 0.003174295595554312618, 0.003570702171545547116, 0.003967108747536782047, 0.004363515323528016111, 0.004759921899519251043, 0.005156328475510485107, 0.005552735051501720039, 0.005949141627492954970, 0.006345548203484189034 ),
 .UNSPECIFIED. ) ;
#3919 = CARTESIAN_POINT ( 'NONE',  ( 4.400293182487617472, 19.52803631353506120, 6.233981582756856987 ) ) ;
#3920 = DIRECTION ( 'NONE',  ( 0.000000000000000000, 0.000000000000000000, 1.000000000000000000 ) ) ;
#3921 = DIRECTION ( 'NONE',  ( -0.000000000000000000, -0.000000000000000000, 1.000000000000000000 ) ) ;
#3922 = EDGE_LOOP ( 'NONE', ( #19589, #4316, #17440, #28748 ) ) ;
#3923 = VECTOR ( 'NONE', #6766, 1000.000000000000000 ) ;
#3924 = CARTESIAN_POINT ( 'NONE',  ( -4.677126025380971441, -39.24912351428226742, 27.49999999999999645 ) ) ;
#3925 = CARTESIAN_POINT ( 'NONE',  ( 11.02326084422093011, -16.70928013427648295, 18.35377592296120497 ) ) ;
#3926 = CARTESIAN_POINT ( 'NONE',  ( 19.87340826026480656, 2.401441585233817566, 19.96783386855779341 ) ) ;
#3927 = ORIENTED_EDGE ( 'NONE', *, *, #28055, .T. ) ;
#3928 = CARTESIAN_POINT ( 'NONE',  ( 14.88222593340886668, 13.36111339922579866, 20.34789198813115263 ) ) ;
#3929 = CARTESIAN_POINT ( 'NONE',  ( 17.92822150912323664, -8.904799031605449500, 6.530762810602277924 ) ) ;
#3930 = CARTESIAN_POINT ( 'NONE',  ( -13.72472375636738029, 10.13620556525982330, 5.810767894563978686 ) ) ;
#3931 = CARTESIAN_POINT ( 'NONE',  ( 4.045241160498761701, 16.55840174588940528, 18.34798005862662507 ) ) ;
#3932 = ORIENTED_EDGE ( 'NONE', *, *, #29834, .F. ) ;
#3933 = ORIENTED_EDGE ( 'NONE', *, *, #19011, .T. ) ;
#3934 = LINE ( 'NONE', #3772, #26256 ) ;
#3935 =( GEOMETRIC_REPRESENTATION_CONTEXT ( 3 ) GLOBAL_UNCERTAINTY_ASSIGNED_CONTEXT ( ( #26681 ) ) GLOBAL_UNIT_ASSIGNED_CONTEXT ( ( #27417, #20529, #25375 ) ) REPRESENTATION_CONTEXT ( 'NONE', 'WORKASPACE' ) );
#3936 = CARTESIAN_POINT ( 'NONE',  ( 10.29553672503491057, -13.60582241699094119, 7.545655578832112020 ) ) ;
#3937 = B_SPLINE_SURFACE_WITH_KNOTS ( 'NONE', 3, 1, ( 
 ( #28544, #28395 ),
 ( #30568, #23998 ),
 ( #19177, #2332 ),
 ( #18720, #4678 ),
 ( #28699, #14500 ),
 ( #301, #4827 ) ),
 .UNSPECIFIED., .F., .F., .F.,
 ( 4, 2, 4 ),
 ( 2, 2 ),
 ( 1.408367944307646891, 1.570796326794821507, 1.733224709277728426 ),
 ( 0.000000000000000000, 1.000000000000000000 ),
 .UNSPECIFIED. ) ;
#3938 = CARTESIAN_POINT ( 'NONE',  ( -5.002692087210951932, 19.38273059899790951, 19.45164628100866722 ) ) ;
#3939 = CARTESIAN_POINT ( 'NONE',  ( -37.99999999999999289, 90.00000000000001421, -75.50000000000000000 ) ) ;
#3940 = AXIS2_PLACEMENT_3D ( 'NONE', #5168, #28727, #21687 ) ;
#3941 = CARTESIAN_POINT ( 'NONE',  ( 0.000000000000000000, 0.000000000000000000, 1.500000000000001332 ) ) ;
#3942 = CARTESIAN_POINT ( 'NONE',  ( 1.000000000000008438, 16.48749217771910125, -0.6213203435596476032 ) ) ;
#3943 = CARTESIAN_POINT ( 'NONE',  ( 24.14264434021281858, -13.29031772318284865, 47.44099319989518193 ) ) ;
#3944 = ORIENTED_EDGE ( 'NONE', *, *, #395, .T. ) ;
#3945 = DIRECTION ( 'NONE',  ( 0.000000000000000000, 0.000000000000000000, 1.000000000000000000 ) ) ;
#3946 = AXIS2_PLACEMENT_3D ( 'NONE', #890, #1517, #24744 ) ;
#3947 = CARTESIAN_POINT ( 'NONE',  ( -4.163336342344337027E-14, -1.387778780781445676E-14, 1.500000000000000000 ) ) ;
#3948 = CARTESIAN_POINT ( 'NONE',  ( 19.81826808356699132, 2.692791747024146254, 20.22277707861861273 ) ) ;
#3949 = ORIENTED_EDGE ( 'NONE', *, *, #942, .F. ) ;
#3950 = ORIENTED_EDGE ( 'NONE', *, *, #25611, .F. ) ;
#3951 = FACE_OUTER_BOUND ( 'NONE', #16122, .T. ) ;
#3952 = AXIS2_PLACEMENT_3D ( 'NONE', #11741, #30768, #25935 ) ;
#3953 = CARTESIAN_POINT ( 'NONE',  ( -40.00000000000000000, 87.00000000000001421, 59.49999999999999289 ) ) ;
#3954 =( BOUNDED_SURFACE ( )  B_SPLINE_SURFACE ( 3, 1, ( 
 ( #26391, #12354 ),
 ( #19518, #12667 ),
 ( #5323, #2994 ),
 ( #15286, #12971 ) ),
 .UNSPECIFIED., .F., .F., .T. ) 
 B_SPLINE_SURFACE_WITH_KNOTS ( ( 4, 4 ),
 ( 2, 2 ),
 ( 0.000000000000000000, 1.000000000000000000 ),
 ( 0.000000000000000000, 1.000000000000000000 ),
 .UNSPECIFIED. ) 
 GEOMETRIC_REPRESENTATION_ITEM ( )  RATIONAL_B_SPLINE_SURFACE ( (
 ( 1.000000000000000000, 1.000000000000000000),
 ( 0.9908525036704132205, 0.9908525036704132205),
 ( 0.9908525036704132205, 0.9908525036704132205),
 ( 1.000000000000000000, 1.000000000000000000) ) ) 
 REPRESENTATION_ITEM ( '' )  SURFACE ( )  );
#3955 = ORIENTED_EDGE ( 'NONE', *, *, #2747, .T. ) ;
#3956 = CARTESIAN_POINT ( 'NONE',  ( -0.5297379638125898627, -19.99304770284714650, 7.156831654632817674 ) ) ;
#3957 = CARTESIAN_POINT ( 'NONE',  ( 10.95142783224707550, 48.78720750482332846, -65.26185492559442025 ) ) ;
#3958 = DIRECTION ( 'NONE',  ( -0.000000000000000000, 0.000000000000000000, 1.000000000000000000 ) ) ;
#3959 = DIRECTION ( 'NONE',  ( 0.000000000000000000, 0.000000000000000000, -1.000000000000000000 ) ) ;
#3960 = CARTESIAN_POINT ( 'NONE',  ( -32.60829997825918980, 13.18983524832148291, 35.60092001944733653 ) ) ;
#3961 = AXIS2_PLACEMENT_3D ( 'NONE', #3539, #13203, #24900 ) ;
#3962 = DIRECTION ( 'NONE',  ( -0.000000000000000000, -0.000000000000000000, -1.000000000000000000 ) ) ;
#3963 = CARTESIAN_POINT ( 'NONE',  ( 1.363408835038997236, -19.97112866468681602, 6.782048567692550378 ) ) ;
#3964 = EDGE_LOOP ( 'NONE', ( #10725, #2520 ) ) ;
#3965 = DIRECTION ( 'NONE',  ( 0.000000000000000000, 1.000000000000000000, 1.193512090021232842E-16 ) ) ;
#3966 = CARTESIAN_POINT ( 'NONE',  ( 0.000000000000000000, 0.000000000000000000, 1.500000000000001332 ) ) ;
#3967 = DIRECTION ( 'NONE',  ( -0.000000000000000000, 0.000000000000000000, 1.000000000000000000 ) ) ;
#3968 = CARTESIAN_POINT ( 'NONE',  ( -17.77309463542033541, -9.210542792609437868, 18.56793045041961321 ) ) ;
#3969 = CARTESIAN_POINT ( 'NONE',  ( 12.56641067637628240, -40.32935944494942504, -1.500000000000000000 ) ) ;
#3970 = B_SPLINE_CURVE_WITH_KNOTS ( 'NONE', 3,
 ( #19233, #18949, #16589, #19088, #4896, #19696, #674, #10502, #8494, #25001, #13156, #22037, #3640, #826, #10350, #29221, #29532, #20328, #7860, #1299, #3177, #3325, #12856, #17369, #29853, #22648, #24683, #22495, #24531, #27043, #15483, #19862, #10814, #20163, #29380, #8020, #8169, #17522, #1141, #5824, #992, #26729 ),
 .UNSPECIFIED., .F., .F.,
 ( 4, 2, 2, 2, 2, 2, 2, 2, 2, 2, 2, 2, 2, 2, 2, 2, 2, 2, 2, 2, 4 ),
 ( 0.02151600789256482779, 0.02343308447725669583, 0.02535016106194856386, 0.02918431423133229299, 0.03110139081602415062, 0.03301846740071601172, 0.03397700569306194573, 0.03493554398540787975, 0.03589408227775381377, 0.03637335142392678078, 0.03685262057009974779, 0.03733188971627271480, 0.03781115886244568874, 0.03876969715479162970, 0.03972823544713757066, 0.04068677373948351161, 0.04260385032417539353, 0.04452092690886727544, 0.04835508007825103927, 0.05027215666294292118, 0.05218923324763480309 ),
 .UNSPECIFIED. ) ;
#3971 = ORIENTED_EDGE ( 'NONE', *, *, #10885, .T. ) ;
#3972 = CARTESIAN_POINT ( 'NONE',  ( -2.081668171172168513E-14, 75.00000000000001421, 37.49999999999999289 ) ) ;
#3973 = CARTESIAN_POINT ( 'NONE',  ( -32.74775157610409337, 27.21557300919391054, -19.50000000000000355 ) ) ;
#3974 = CARTESIAN_POINT ( 'NONE',  ( 27.38650679510956820, -30.38832073129480094, 30.00757695512932344 ) ) ;
#3975 = CARTESIAN_POINT ( 'NONE',  ( -6.102995743689038299, 19.04655207687856944, 5.652912763329821288 ) ) ;
#3976 = VERTEX_POINT ( 'NONE', #4945 ) ;
#3977 = DIRECTION ( 'NONE',  ( 0.000000000000000000, -0.000000000000000000, -1.000000000000000000 ) ) ;
#3978 = ORIENTED_EDGE ( 'NONE', *, *, #412, .F. ) ;
#3979 = CARTESIAN_POINT ( 'NONE',  ( 2.687479362164894248, -44.39187623478217404, -19.50000000000000355 ) ) ;
#3980 = DIRECTION ( 'NONE',  ( 1.000000000000000000, 0.000000000000000000, 0.000000000000000000 ) ) ;
#3981 = ORIENTED_EDGE ( 'NONE', *, *, #21808, .F. ) ;
#3982 = DIRECTION ( 'NONE',  ( 1.000000000000000000, 0.000000000000000000, 0.000000000000000000 ) ) ;
#3983 = CARTESIAN_POINT ( 'NONE',  ( 0.000000000000000000, 0.000000000000000000, 1.500000000000000000 ) ) ;
#3984 = ORIENTED_EDGE ( 'NONE', *, *, #18723, .T. ) ;
#3985 = LINE ( 'NONE', #13508, #29816 ) ;
#3986 = TOROIDAL_SURFACE ( 'NONE', #25903, 17.00000000000000000, 3.000000000000000000 ) ;
#3987 = CYLINDRICAL_SURFACE ( 'NONE', #17331, 0.7500000000000006661 ) ;
#3988 = CARTESIAN_POINT ( 'NONE',  ( 0.4302108320067679070, -20.01327865860580602, 18.34838970509067479 ) ) ;
#3989 = VERTEX_POINT ( 'NONE', #19137 ) ;
#3990 = CARTESIAN_POINT ( 'NONE',  ( 11.69640250238807333, 12.44177653180062748, 19.02573955821369012 ) ) ;
#3991 = DIRECTION ( 'NONE',  ( 0.000000000000000000, 0.000000000000000000, 1.000000000000000000 ) ) ;
#3992 = CARTESIAN_POINT ( 'NONE',  ( 15.57266529552203416, -38.96488032230103471, 1.500000000000000000 ) ) ;
#3993 = CARTESIAN_POINT ( 'NONE',  ( -15.42380629414487991, -7.219239307198620281, 20.14907003336613300 ) ) ;
#3994 = DIRECTION ( 'NONE',  ( 1.000000000000000000, 0.000000000000000000, 0.000000000000000000 ) ) ;
#3995 = DIRECTION ( 'NONE',  ( 0.000000000000000000, 0.5000000000000006661, 0.8660254037844382635 ) ) ;
#3996 = FACE_OUTER_BOUND ( 'NONE', #27575, .T. ) ;
#3997 = CARTESIAN_POINT ( 'NONE',  ( 19.74251403343738076, 3.198927889078825970, 5.652196082369965069 ) ) ;
#3998 = CARTESIAN_POINT ( 'NONE',  ( -9.372686588590493528, -14.20906563288477997, 19.08155846658118548 ) ) ;
#3999 = ORIENTED_EDGE ( 'NONE', *, *, #30693, .F. ) ;
#4000 = ORIENTED_EDGE ( 'NONE', *, *, #24041, .F. ) ;
#4001 = FACE_BOUND ( 'NONE', #25427, .T. ) ;
#4002 = CARTESIAN_POINT ( 'NONE',  ( -40.05520443301966083, -7.028746486913004077, -16.50000000000000000 ) ) ;
#4003 = CARTESIAN_POINT ( 'NONE',  ( 28.34828976096172681, 29.18752572968383419, -1.500000000000000000 ) ) ;
#4004 = ORIENTED_EDGE ( 'NONE', *, *, #2534, .F. ) ;
#4005 =( LENGTH_UNIT ( ) NAMED_UNIT ( * ) SI_UNIT ( .MILLI., .METRE. ) );
#4006 = DIRECTION ( 'NONE',  ( 0.000000000000000000, 0.000000000000000000, -1.000000000000000000 ) ) ;
#4007 = AXIS2_PLACEMENT_3D ( 'NONE', #504, #24192, #9867 ) ;
#4008 = CARTESIAN_POINT ( 'NONE',  ( 9.051788058555931826, -14.41610800088323252, 19.66962785902261857 ) ) ;
#4009 = ORIENTED_EDGE ( 'NONE', *, *, #18946, .T. ) ;
#4010 = ORIENTED_EDGE ( 'NONE', *, *, #6742, .T. ) ;
#4011 = CARTESIAN_POINT ( 'NONE',  ( -10.62409560796092833, -16.94539057243558489, 18.34726407865098707 ) ) ;
#4012 = CARTESIAN_POINT ( 'NONE',  ( -30.03792366816883330, -15.52577997660842435, 36.94438844912276920 ) ) ;
#4013 = DIRECTION ( 'NONE',  ( -0.000000000000000000, -0.000000000000000000, 1.000000000000000000 ) ) ;
#4014 = CARTESIAN_POINT ( 'NONE',  ( -3.917446247819842409, 37.31292274963767142, 37.50000000001976019 ) ) ;
#4015 = ORIENTED_EDGE ( 'NONE', *, *, #23131, .F. ) ;
#4016 = APPLICATION_CONTEXT ( 'automotive_design' ) ;
#4017 = DIRECTION ( 'NONE',  ( 0.000000000000000000, 1.000000000000000000, 0.000000000000000000 ) ) ;
#4018 = ORIENTED_EDGE ( 'NONE', *, *, #15307, .F. ) ;
#4019 = EDGE_CURVE ( 'NONE', #6841, #26671, #13287, .T. ) ;
#4020 = FACE_OUTER_BOUND ( 'NONE', #26751, .T. ) ;
#4021 = AXIS2_PLACEMENT_3D ( 'NONE', #17121, #3236, #12612 ) ;
#4022 = LINE ( 'NONE', #13844, #14811 ) ;
#4023 = VERTEX_POINT ( 'NONE', #7595 ) ;
#4024 = CARTESIAN_POINT ( 'NONE',  ( 0.000000000000000000, 0.000000000000000000, 1.500000000000001332 ) ) ;
#4025 = CARTESIAN_POINT ( 'NONE',  ( 25.47847050916410439, -26.57182937991349903, 26.54355021145563143 ) ) ;
#4026 = EDGE_CURVE ( 'NONE', #24952, #26662, #8650, .T. ) ;
#4027 = CYLINDRICAL_SURFACE ( 'NONE', #17745, 0.7500000000000006661 ) ;
#4028 = EDGE_CURVE ( 'NONE', #13391, #8694, #14252, .T. ) ;
#4029 = FACE_OUTER_BOUND ( 'NONE', #6532, .T. ) ;
#4030 = CARTESIAN_POINT ( 'NONE',  ( -8.546423435383420752, -14.74799740001550141, 5.652196082368483587 ) ) ;
#4031 = FACE_OUTER_BOUND ( 'NONE', #21646, .T. ) ;
#4032 = CARTESIAN_POINT ( 'NONE',  ( 11.18191171624325797, -16.60365183919260090, 18.34838970509067479 ) ) ;
#4033 = CARTESIAN_POINT ( 'NONE',  ( 34.83396020575241891, 10.30249279383515848, 34.80090346875810070 ) ) ;
#4034 = ORIENTED_EDGE ( 'NONE', *, *, #21197, .F. ) ;
#4035 = ORIENTED_EDGE ( 'NONE', *, *, #10269, .T. ) ;
#4036 = DIRECTION ( 'NONE',  ( 1.000000000000000000, 0.000000000000000000, 0.000000000000000000 ) ) ;
#4037 = VECTOR ( 'NONE', #9389, 1000.000000000000000 ) ;
#4038 = DIRECTION ( 'NONE',  ( -0.000000000000000000, -0.000000000000000000, -1.000000000000000000 ) ) ;
#4039 = ORIENTED_EDGE ( 'NONE', *, *, #16675, .F. ) ;
#4040 = DIRECTION ( 'NONE',  ( -1.000000000000000000, 0.000000000000000000, 0.000000000000000000 ) ) ;
#4041 = CIRCLE ( 'NONE', #10515, 9.084132297865673777 ) ;
#4042 = DIRECTION ( 'NONE',  ( -0.000000000000000000, -0.000000000000000000, -1.000000000000000000 ) ) ;
#4043 = ADVANCED_FACE ( 'NONE', ( #5561 ), #20515, .F. ) ;
#4044 = FACE_OUTER_BOUND ( 'NONE', #30217, .T. ) ;
#4045 = VERTEX_POINT ( 'NONE', #29895 ) ;
#4046 = EDGE_CURVE ( 'NONE', #19640, #26022, #793, .T. ) ;
#4047 = DIRECTION ( 'NONE',  ( 0.000000000000000000, 0.000000000000000000, -1.000000000000000000 ) ) ;
#4048 = EDGE_CURVE ( 'NONE', #27691, #1845, #12903, .T. ) ;
#4049 = CARTESIAN_POINT ( 'NONE',  ( -32.68377466358848693, -8.668986135640256663, 41.18623755341147330 ) ) ;
#4050 = ORIENTED_EDGE ( 'NONE', *, *, #21197, .T. ) ;
#4051 = CARTESIAN_POINT ( 'NONE',  ( 8.413215745754998309, -3.196529495465417980, 21.50000000000000000 ) ) ;
#4052 = ORIENTED_EDGE ( 'NONE', *, *, #22560, .T. ) ;
#4053 = CARTESIAN_POINT ( 'NONE',  ( -6.974883619896829146, -5.687793815610328707, 1.500000000000001332 ) ) ;
#4054 = EDGE_CURVE ( 'NONE', #24825, #21731, #9306, .T. ) ;
#4055 = ORIENTED_EDGE ( 'NONE', *, *, #21799, .T. ) ;
#4056 = ORIENTED_EDGE ( 'NONE', *, *, #35, .F. ) ;
#4057 = EDGE_CURVE ( 'NONE', #26463, #11295, #7281, .T. ) ;
#4058 = EDGE_CURVE ( 'NONE', #6837, #752, #27084, .T. ) ;
#4059 = LINE ( 'NONE', #20579, #17067 ) ;
#4060 = CARTESIAN_POINT ( 'NONE',  ( -0.4564504349075055867, 9.471281197126600659, 21.50000000000000000 ) ) ;
#4061 = ORIENTED_EDGE ( 'NONE', *, *, #17013, .T. ) ;
#4062 = VECTOR ( 'NONE', #15681, 1000.000000000000000 ) ;
#4063 = CARTESIAN_POINT ( 'NONE',  ( -34.83396020575242602, 10.30249279383516381, 27.50000000000001066 ) ) ;
#4064 = FACE_OUTER_BOUND ( 'NONE', #9660, .T. ) ;
#4065 = CARTESIAN_POINT ( 'NONE',  ( 31.29501345866090389, 26.27841684422296353, -6.500000000000000888 ) ) ;
#4066 = VERTEX_POINT ( 'NONE', #15678 ) ;
#4067 = CARTESIAN_POINT ( 'NONE',  ( -16.90489691178405707, 2.092419235659072729, 20.25336174263950184 ) ) ;
#4068 = DIRECTION ( 'NONE',  ( -0.000000000000000000, -1.000000000000000000, -0.000000000000000000 ) ) ;
#4069 = CARTESIAN_POINT ( 'NONE',  ( -15.57270467870638342, 12.57827228024023825, 5.704143890883081269 ) ) ;
#4070 = CARTESIAN_POINT ( 'NONE',  ( 3.623302445573593378, 16.66947753447049152, 20.25542030744407640 ) ) ;
#4071 = VERTEX_POINT ( 'NONE', #24730 ) ;
#4072 = FACE_OUTER_BOUND ( 'NONE', #29918, .T. ) ;
#4073 = FACE_OUTER_BOUND ( 'NONE', #22551, .T. ) ;
#4074 = EDGE_CURVE ( 'NONE', #19699, #4573, #15229, .T. ) ;
#4075 = VECTOR ( 'NONE', #16182, 1000.000000000000000 ) ;
#4076 = CARTESIAN_POINT ( 'NONE',  ( -4.626122995383912695, 16.38173570853529881, 19.00652017443069752 ) ) ;
#4077 = PRESENTATION_STYLE_ASSIGNMENT (( #15939 ) ) ;
#4078 = DIRECTION ( 'NONE',  ( -1.000000000000000000, 0.000000000000000000, 0.000000000000000000 ) ) ;
#4079 = LINE ( 'NONE', #13609, #19373 ) ;
#4080 = ITEM_DEFINED_TRANSFORMATION ( 'NONE', 'NONE', #2925,  #7396 ) ;
#4081 = EDGE_CURVE ( 'NONE', #1314, #25466, #15529, .T. ) ;
#4082 = FACE_OUTER_BOUND ( 'NONE', #16701, .T. ) ;
#4083 = ORIENTED_EDGE ( 'NONE', *, *, #3661, .T. ) ;
#4084 = EDGE_CURVE ( 'NONE', #15207, #7019, #19784, .T. ) ;
#4085 = VECTOR ( 'NONE', #30821, 1000.000000000000000 ) ;
#4086 = CARTESIAN_POINT ( 'NONE',  ( 1.239979252855709868, -19.96159058730291136, 6.149077423860696001 ) ) ;
#4087 = DIRECTION ( 'NONE',  ( -0.000000000000000000, -0.000000000000000000, 1.000000000000000000 ) ) ;
#4088 = DIRECTION ( 'NONE',  ( -0.000000000000000000, -1.000000000000000000, -0.000000000000000000 ) ) ;
#4089 = ORIENTED_EDGE ( 'NONE', *, *, #130, .F. ) ;
#4090 = DIRECTION ( 'NONE',  ( 1.000000000000000000, 0.000000000000000000, 0.000000000000000000 ) ) ;
#4091 = EDGE_LOOP ( 'NONE', ( #13530, #26791, #12899, #4967 ) ) ;
#4092 = CARTESIAN_POINT ( 'NONE',  ( 2.094186647214743235, -9.248129367672072831, 13.00000000000000178 ) ) ;
#4093 = CARTESIAN_POINT ( 'NONE',  ( -19.94291556179616265, 1.510882595598286970, 19.08830981656264214 ) ) ;
#4094 = ORIENTED_EDGE ( 'NONE', *, *, #2774, .F. ) ;
#4095 = DIRECTION ( 'NONE',  ( 1.000000000000000000, 0.000000000000000000, 0.000000000000000000 ) ) ;
#4096 = FACE_OUTER_BOUND ( 'NONE', #11719, .T. ) ;
#4097 = DIRECTION ( 'NONE',  ( -1.000000000000000000, 0.000000000000000000, -0.000000000000000000 ) ) ;
#4098 = CARTESIAN_POINT ( 'NONE',  ( 28.37932450449293853, 10.51822134874671022, 1.500000000000000000 ) ) ;
#4099 = DIRECTION ( 'NONE',  ( -0.000000000000000000, 1.000000000000000000, -0.000000000000000000 ) ) ;
#4100 = CARTESIAN_POINT ( 'NONE',  ( 33.01877980957530667, -12.12572312222180670, 39.84356070656651383 ) ) ;
#4101 = DIRECTION ( 'NONE',  ( -0.000000000000000000, 0.000000000000000000, 1.000000000000000000 ) ) ;
#4102 = CARTESIAN_POINT ( 'NONE',  ( -16.84890868873869607, 2.447051129653413870, 6.031926333436659071 ) ) ;
#4103 = VERTEX_POINT ( 'NONE', #29726 ) ;
#4104 = VECTOR ( 'NONE', #6592, 1000.000000000000114 ) ;
#4105 = CARTESIAN_POINT ( 'NONE',  ( 8.752572334588123226, -2.431858781452763463, 21.50000000000000000 ) ) ;
#4106 = CARTESIAN_POINT ( 'NONE',  ( 37.16608720827707657, -51.86186943028246787, 57.49999999999999289 ) ) ;
#4107 = VERTEX_POINT ( 'NONE', #8063 ) ;
#4108 = DIRECTION ( 'NONE',  ( -1.000000000000000000, -0.000000000000000000, -0.000000000000000000 ) ) ;
#4109 = CARTESIAN_POINT ( 'NONE',  ( -17.86170306354901527, -9.037578821739913337, 18.44527579819791185 ) ) ;
#4110 = EDGE_CURVE ( 'NONE', #19511, #20108, #9346, .T. ) ;
#4111 = CARTESIAN_POINT ( 'NONE',  ( -12.56641067637617759, -40.32935944494947478, -1.500000000000000000 ) ) ;
#4112 = EDGE_CURVE ( 'NONE', #14448, #4543, #20664, .T. ) ;
#4113 = CARTESIAN_POINT ( 'NONE',  ( -23.17581250239728519, 34.50630206824672541, 1.499999999999999778 ) ) ;
#4114 = ORIENTED_EDGE ( 'NONE', *, *, #249, .F. ) ;
#4115 = CARTESIAN_POINT ( 'NONE',  ( -0.4522595252855764469, -19.99510590919687303, 18.72886616302735519 ) ) ;
#4116 = AXIS2_PLACEMENT_3D ( 'NONE', #10753, #20264, #29789 ) ;
#4117 = CARTESIAN_POINT ( 'NONE',  ( -37.99999999999999289, 209.2686044187655909, -22.50000000000001421 ) ) ;
#4118 = CARTESIAN_POINT ( 'NONE',  ( 36.29469092165690114, -9.775717669454033754, 37.49999999999255351 ) ) ;
#4120 = AXIS2_PLACEMENT_3D ( 'NONE', #13060, #10867, #22550 ) ;
#4119 = CARTESIAN_POINT ( 'NONE',  ( -2.555255504830902691, 9.131494062835640690, 13.00000000000000178 ) ) ;
#4121 = VERTEX_POINT ( 'NONE', #13518 ) ;
#4122 = CARTESIAN_POINT ( 'NONE',  ( 12.33859880789485253, 8.132258305203430737, -16.50000000000000000 ) ) ;
#4123 = ORIENTED_EDGE ( 'NONE', *, *, #2310, .T. ) ;
#4124 = CARTESIAN_POINT ( 'NONE',  ( -20.65888525914099105, 38.75220717792564784, -19.50000000000000355 ) ) ;
#4125 = DIRECTION ( 'NONE',  ( 0.000000000000000000, -0.000000000000000000, -1.000000000000000000 ) ) ;
#4126 = VERTEX_POINT ( 'NONE', #25360 ) ;
#4127 = CARTESIAN_POINT ( 'NONE',  ( -15.78417422266179315, -38.97739145708682429, 29.15446067280243270 ) ) ;
#4128 = ORIENTED_EDGE ( 'NONE', *, *, #4081, .T. ) ;
#4129 = CARTESIAN_POINT ( 'NONE',  ( -25.41654339919794836, -6.509636863629521208, 44.52079389600195469 ) ) ;
#4130 = FACE_OUTER_BOUND ( 'NONE', #14028, .T. ) ;
#4131 = CARTESIAN_POINT ( 'NONE',  ( 0.5064538767941890729, -20.01148730445866164, 18.35718225375110180 ) ) ;
#4132 = ORIENTED_EDGE ( 'NONE', *, *, #21013, .T. ) ;
#4133 = CARTESIAN_POINT ( 'NONE',  ( 11.65964093050817674, 12.47882650181266051, 19.28454053338348828 ) ) ;
#4134 = AXIS2_PLACEMENT_3D ( 'NONE', #29072, #5984, #5366 ) ;
#4135 = PLANE ( 'NONE',  #1422 ) ;
#4136 = DIRECTION ( 'NONE',  ( 0.000000000000000000, 0.000000000000000000, 1.000000000000000000 ) ) ;
#4137 = AXIS2_PLACEMENT_3D ( 'NONE', #973, #12834, #20459 ) ;
#4138 = DIRECTION ( 'NONE',  ( -1.000000000000000000, 0.000000000000000000, 0.000000000000000000 ) ) ;
#4139 = CARTESIAN_POINT ( 'NONE',  ( -15.52715705409945457, -6.980092275558532400, 18.83976166372255179 ) ) ;
#4140 = CARTESIAN_POINT ( 'NONE',  ( -47.00000000000000000, 87.00000000000001421, 52.49999999999999289 ) ) ;
#4141 = CARTESIAN_POINT ( 'NONE',  ( -3.515970705488605130, -17.06554576617236307, 1.500000000000000000 ) ) ;
#4142 = DIRECTION ( 'NONE',  ( 0.000000000000000000, 0.000000000000000000, 1.000000000000000000 ) ) ;
#4143 = CARTESIAN_POINT ( 'NONE',  ( -18.04156136322730219, -8.631457789788591128, 18.34798005863226678 ) ) ;
#4144 = CARTESIAN_POINT ( 'NONE',  ( 0.8476314135585345522, 42.50000000000000711, 28.83974596215562869 ) ) ;
#4145 = LINE ( 'NONE', #27557, #6094 ) ;
#4146 = EDGE_LOOP ( 'NONE', ( #11075, #24133, #28915, #1546 ) ) ;
#4147 = ORIENTED_EDGE ( 'NONE', *, *, #4054, .F. ) ;
#4148 = DIRECTION ( 'NONE',  ( 1.000000000000000000, 0.000000000000000000, 0.000000000000000000 ) ) ;
#4149 = DIRECTION ( 'NONE',  ( 0.000000000000000000, 0.000000000000000000, 1.000000000000000000 ) ) ;
#4150 = CARTESIAN_POINT ( 'NONE',  ( -19.64177907938615064, -36.71644397333972876, 24.50000000000000000 ) ) ;
#4151 = VERTEX_POINT ( 'NONE', #6485 ) ;
#4152 = DIRECTION ( 'NONE',  ( 0.000000000000000000, 0.000000000000000000, 1.000000000000000000 ) ) ;
#4153 = CIRCLE ( 'NONE', #18608, 6.000000000000005329 ) ;
#4154 = CARTESIAN_POINT ( 'NONE',  ( 6.974883619896790954, 5.687793815610376669, 21.50000000000000000 ) ) ;
#4155 = DIRECTION ( 'NONE',  ( 0.000000000000000000, -1.132880637372608986E-16, 1.000000000000000000 ) ) ;
#4156 = CIRCLE ( 'NONE', #21578, 20.00000000000000355 ) ;
#4157 = VERTEX_POINT ( 'NONE', #23315 ) ;
#4158 = CIRCLE ( 'NONE', #13143, 23.20393738267338790 ) ;
#4159 = CARTESIAN_POINT ( 'NONE',  ( 26.80246859415415273, -7.028748154183637631, -6.500000000000000888 ) ) ;
#4160 = DIRECTION ( 'NONE',  ( 0.000000000000000000, 0.000000000000000000, 1.000000000000000000 ) ) ;
#4161 = CARTESIAN_POINT ( 'NONE',  ( 12.72536390617885438, -2.839914339433650348, 1.500000000000001332 ) ) ;
#4162 = VERTEX_POINT ( 'NONE', #18799 ) ;
#4163 = DIRECTION ( 'NONE',  ( 0.000000000000000000, 0.000000000000000000, -1.000000000000000000 ) ) ;
#4164 = VERTEX_POINT ( 'NONE', #1802 ) ;
#4165 = DIRECTION ( 'NONE',  ( -0.9329908884337522190, -0.3598999890241700306, 0.000000000000000000 ) ) ;
#4166 = CARTESIAN_POINT ( 'NONE',  ( -14.93932203929706759, 13.29757777824904075, 7.454139397117721444 ) ) ;
#4167 = ORIENTED_EDGE ( 'NONE', *, *, #29989, .T. ) ;
#4168 = CYLINDRICAL_SURFACE ( 'NONE', #19812, 0.7500000000000006661 ) ;
#4169 = CARTESIAN_POINT ( 'NONE',  ( 8.828055718019477638, -43.02192272134110596, -16.50000000000000000 ) ) ;
#4170 = CARTESIAN_POINT ( 'NONE',  ( 19.73705937795079279, 3.341332093703274442, 7.643931100913408550 ) ) ;
#4171 = CIRCLE ( 'NONE', #11154, 23.20393738267338790 ) ;
#4172 = LINE ( 'NONE', #29112, #30193 ) ;
#4173 = CARTESIAN_POINT ( 'NONE',  ( -16.99844672493304998, 1.385815296451945899, 18.34938820207544907 ) ) ;
#4174 = TOROIDAL_SURFACE ( 'NONE', #27614, 17.00000000000000000, 3.000000000000000000 ) ;
#4175 = CARTESIAN_POINT ( 'NONE',  ( -9.395142731145654125, -14.19351217900082496, 6.519181285484530797 ) ) ;
#4176 = CARTESIAN_POINT ( 'NONE',  ( 2.431858781452735041, 8.752572334588126779, 21.50000000000000000 ) ) ;
#4177 = ORIENTED_EDGE ( 'NONE', *, *, #7257, .F. ) ;
#4178 = CIRCLE ( 'NONE', #7096, 7.500000000000013323 ) ;
#4179 = CARTESIAN_POINT ( 'NONE',  ( -4.776122516674677878E-15, -42.50000000000000000, 28.83974596215560737 ) ) ;
#4180 = CARTESIAN_POINT ( 'NONE',  ( 4.677126025380961671, -39.24912351428227453, 27.50000000000000355 ) ) ;
#4181 = VERTEX_POINT ( 'NONE', #28319 ) ;
#4182 = VERTEX_POINT ( 'NONE', #4453 ) ;
#4183 = EDGE_CURVE ( 'NONE', #5874, #10035, #5818, .T. ) ;
#4184 = LINE ( 'NONE', #8426, #26587 ) ;
#4185 = EDGE_CURVE ( 'NONE', #15872, #6674, #25382, .T. ) ;
#4186 = CARTESIAN_POINT ( 'NONE',  ( -9.056472324687611319, -0.7083562926194842957, 21.50000000000000000 ) ) ;
#4187 = ORIENTED_EDGE ( 'NONE', *, *, #24263, .F. ) ;
#4188 = CARTESIAN_POINT ( 'NONE',  ( -12.73056545647080640, 11.29944703098672854, 6.385774490351133537 ) ) ;
#4189 = DIRECTION ( 'NONE',  ( 1.000000000000000000, 0.000000000000000000, 0.000000000000000000 ) ) ;
#4190 = ORIENTED_EDGE ( 'NONE', *, *, #25406, .F. ) ;
#4191 = CARTESIAN_POINT ( 'NONE',  ( -6.482337650448453559, -6.364020599487773211, 13.22130136205108819 ) ) ;
#4192 = CARTESIAN_POINT ( 'NONE',  ( -18.04156136322730219, -8.631457789788591128, 18.34798005863226678 ) ) ;
#4193 = ORIENTED_EDGE ( 'NONE', *, *, #28094, .F. ) ;
#4194 = ADVANCED_FACE ( 'NONE', ( #6944 ), #8983, .F. ) ;
#4195 = CARTESIAN_POINT ( 'NONE',  ( 5.687793815610356241, -6.974883619896809606, 21.50000000000000000 ) ) ;
#4196 = AXIS2_PLACEMENT_3D ( 'NONE', #2618, #274, #28200 ) ;
#4197 = EDGE_LOOP ( 'NONE', ( #27838, #16737, #25976, #14993 ) ) ;
#4198 = FACE_OUTER_BOUND ( 'NONE', #20942, .T. ) ;
#4199 = EDGE_LOOP ( 'NONE', ( #517, #16025, #16239, #292, #1167, #17865, #20571, #17192, #27539, #4262, #21843, #21431, #5471, #14410, #5926, #20078, #24138, #24209, #12133, #7149, #26635, #2017, #7569, #20691, #3431, #9511 ) ) ;
#4200 = EDGE_LOOP ( 'NONE', ( #22486, #236, #24354, #13821 ) ) ;
#4201 = CARTESIAN_POINT ( 'NONE',  ( 39.99999999999998579, 0.000000000000000000, 62.49999999999999289 ) ) ;
#4202 = DIRECTION ( 'NONE',  ( 1.000000000000000000, 0.000000000000000000, 0.000000000000000000 ) ) ;
#4203 = EDGE_CURVE ( 'NONE', #7918, #25828, #27233, .T. ) ;
#4204 = CARTESIAN_POINT ( 'NONE',  ( -31.18890335284659443, -19.89223002944918051, 34.80090346875804386 ) ) ;
#4205 = DIRECTION ( 'NONE',  ( 0.000000000000000000, 1.000000000000000000, 6.938893903907227392E-16 ) ) ;
#4206 = CARTESIAN_POINT ( 'NONE',  ( 16.80963242778062749, 2.754998275627143389, 20.25336174263950184 ) ) ;
#4207 = EDGE_CURVE ( 'NONE', #12790, #24988, #12731, .T. ) ;
#4208 = ORIENTED_EDGE ( 'NONE', *, *, #6336, .T. ) ;
#4209 = EDGE_CURVE ( 'NONE', #25701, #23663, #9125, .T. ) ;
#4210 = CARTESIAN_POINT ( 'NONE',  ( -16.88948989945504309, 2.193765388987376497, 20.19668224736330941 ) ) ;
#4211 = CARTESIAN_POINT ( 'NONE',  ( 18.09058649146511044, -8.570415951004783039, 5.862424720655265098 ) ) ;
#4212 = CARTESIAN_POINT ( 'NONE',  ( -15.90168156411149170, 12.15925017959999188, 6.131018562779544823 ) ) ;
#4213 = CARTESIAN_POINT ( 'NONE',  ( 3.200917658998823967, 16.77053181957577621, 18.82680253904184298 ) ) ;
#4214 = VERTEX_POINT ( 'NONE', #6779 ) ;
#4215 = ORIENTED_EDGE ( 'NONE', *, *, #28347, .T. ) ;
#4216 = VECTOR ( 'NONE', #30204, 1000.000000000000000 ) ;
#4217 = PLANE ( 'NONE',  #27251 ) ;
#4218 = EDGE_CURVE ( 'NONE', #14001, #13970, #18775, .T. ) ;
#4219 = CARTESIAN_POINT ( 'NONE',  ( 12.13957942244085331, -40.43335259791965086, 21.42951026665136993 ) ) ;
#4220 = CARTESIAN_POINT ( 'NONE',  ( -5.222323004038176286, 16.21609733491350980, 20.29090034784956131 ) ) ;
#4221 = CARTESIAN_POINT ( 'NONE',  ( 11.68275852896170619, 12.45554129447766378, 6.392658652357122939 ) ) ;
#4222 = CARTESIAN_POINT ( 'NONE',  ( -27.99175947355483274, 24.84200504376626029, 27.50000000000000355 ) ) ;
#4223 = CARTESIAN_POINT ( 'NONE',  ( 9.216505592218814158, -7.781333699927420966, 1.500000000000000000 ) ) ;
#4224 = EDGE_CURVE ( 'NONE', #27607, #29319, #11944, .T. ) ;
#4225 = ORIENTED_EDGE ( 'NONE', *, *, #9051, .T. ) ;
#4226 = CARTESIAN_POINT ( 'NONE',  ( -17.06612199394663421, 0.6423840055640266389, 6.782048567692550378 ) ) ;
#4227 = EDGE_CURVE ( 'NONE', #18904, #8467, #5218, .T. ) ;
#4228 = DIRECTION ( 'NONE',  ( -1.000000000000000000, 0.000000000000000000, 0.000000000000000000 ) ) ;
#4229 = LINE ( 'NONE', #23548, #16439 ) ;
#4230 = ORIENTED_EDGE ( 'NONE', *, *, #2891, .T. ) ;
#4231 = EDGE_CURVE ( 'NONE', #30675, #20736, #20734, .T. ) ;
#4232 = FACE_OUTER_BOUND ( 'NONE', #30300, .T. ) ;
#4233 = ORIENTED_EDGE ( 'NONE', *, *, #16442, .T. ) ;
#4234 = CARTESIAN_POINT ( 'NONE',  ( 18.38343463818524626, -7.922482876633606175, 5.652605728828373977 ) ) ;
#4235 = CARTESIAN_POINT ( 'NONE',  ( -20.94685371601454094, 37.75489722317177410, -16.49999999999998934 ) ) ;
#4236 = ORIENTED_EDGE ( 'NONE', *, *, #14115, .T. ) ;
#4237 = DIRECTION ( 'NONE',  ( -0.000000000000000000, -0.000000000000000000, 1.000000000000000000 ) ) ;
#4238 = CIRCLE ( 'NONE', #1267, 1.447898107987198646 ) ;
#4239 = CARTESIAN_POINT ( 'NONE',  ( 5.317332916452814473, 49.71854057255719539, -40.96554122676177201 ) ) ;
#4240 = CARTESIAN_POINT ( 'NONE',  ( -4.163336342344337027E-14, 1.387778780781445676E-14, 1.500000000000000000 ) ) ;
#4241 = LINE ( 'NONE', #6445, #26813 ) ;
#4242 = DIRECTION ( 'NONE',  ( -0.000000000000000000, -0.000000000000000000, -1.000000000000000000 ) ) ;
#4243 = LINE ( 'NONE', #5017, #7840 ) ;
#4244 = CARTESIAN_POINT ( 'NONE',  ( -3.515970705488605130, -17.06554576617236307, 1.500000000000000000 ) ) ;
#4245 = EDGE_CURVE ( 'NONE', #24485, #20446, #30795, .T. ) ;
#4246 = EDGE_LOOP ( 'NONE', ( #3474, #28596, #25128, #21949, #3916, #27127 ) ) ;
#4247 = ADVANCED_FACE ( 'NONE', ( #528 ), #12297, .T. ) ;
#4248 = DIRECTION ( 'NONE',  ( -0.000000000000000000, 1.132880637372608986E-16, -1.000000000000000000 ) ) ;
#4249 = FACE_OUTER_BOUND ( 'NONE', #6363, .T. ) ;
#4250 = ORIENTED_EDGE ( 'NONE', *, *, #17204, .F. ) ;
#4251 = CYLINDRICAL_SURFACE ( 'NONE', #22007, 9.482273699623480212 ) ;
#4252 = CARTESIAN_POINT ( 'NONE',  ( -17.81743587613174284, -9.123988531026231641, 18.50655187082627862 ) ) ;
#4253 = EDGE_CURVE ( 'NONE', #16582, #17083, #21587, .T. ) ;
#4254 = CARTESIAN_POINT ( 'NONE',  ( -2.552544031601109875, 42.50000000001772094, -1.500000000000000000 ) ) ;
#4255 = CARTESIAN_POINT ( 'NONE',  ( -33.52485258639264032, 10.76172163581451890, 35.54788606881927393 ) ) ;
#4256 = VERTEX_POINT ( 'NONE', #2878 ) ;
#4257 = CARTESIAN_POINT ( 'NONE',  ( -0.2646837113541511410, -19.99846847964001384, 18.54479204710283469 ) ) ;
#4258 = CARTESIAN_POINT ( 'NONE',  ( 49.99999999999998579, 50.00000000000000000, 12.49999999999999112 ) ) ;
#4259 = CARTESIAN_POINT ( 'NONE',  ( 14.08068486978915601, -39.64040334357339646, 29.09405787692634249 ) ) ;
#4260 = EDGE_CURVE ( 'NONE', #4652, #6382, #12402, .T. ) ;
#4261 = CYLINDRICAL_SURFACE ( 'NONE', #27545, 0.7500000000000006661 ) ;
#4262 = ORIENTED_EDGE ( 'NONE', *, *, #9922, .T. ) ;
#4263 = CARTESIAN_POINT ( 'NONE',  ( -7.341751895053199028, 5.349779314757666882, 13.22130136205108819 ) ) ;
#4264 = VERTEX_POINT ( 'NONE', #29080 ) ;
#4265 = FACE_OUTER_BOUND ( 'NONE', #16896, .T. ) ;
#4266 = LINE ( 'NONE', #1640, #23887 ) ;
#4267 = ORIENTED_EDGE ( 'NONE', *, *, #23852, .F. ) ;
#4268 = FACE_OUTER_BOUND ( 'NONE', #21376, .T. ) ;
#4269 = ORIENTED_EDGE ( 'NONE', *, *, #6714, .T. ) ;
#4270 = CARTESIAN_POINT ( 'NONE',  ( -24.86084284002701850, -6.930828199065642181, 44.94877300773892159 ) ) ;
#4271 = ADVANCED_FACE ( 'NONE', ( #220 ), #25079, .T. ) ;
#4272 = CARTESIAN_POINT ( 'NONE',  ( -10.05618025891931389, -17.30842068227156361, 5.810767894563978686 ) ) ;
#4273 = ADVANCED_FACE ( 'NONE', ( #29691 ), #5523, .F. ) ;
#4274 = DIRECTION ( 'NONE',  ( 1.000000000000000000, 0.000000000000000000, 0.000000000000000000 ) ) ;
#4275 = DIRECTION ( 'NONE',  ( 0.8932538319083086487, -0.4495526574063634095, 0.000000000000000000 ) ) ;
#4276 = VERTEX_POINT ( 'NONE', #10200 ) ;
#4277 = CARTESIAN_POINT ( 'NONE',  ( 23.13152334643393715, 11.98019263786950184, 44.70772167928459595 ) ) ;
#4278 = AXIS2_PLACEMENT_3D ( 'NONE', #19953, #15105, #29472 ) ;
#4279 = CARTESIAN_POINT ( 'NONE',  ( -20.71335220384823117, 27.86167394782616213, -16.50000000000000000 ) ) ;
#4280 = DIRECTION ( 'NONE',  ( 0.000000000000000000, 0.000000000000000000, 1.000000000000000000 ) ) ;
#4281 = DIRECTION ( 'NONE',  ( 0.000000000000000000, 0.000000000000000000, -1.000000000000000000 ) ) ;
#4282 = CARTESIAN_POINT ( 'NONE',  ( -41.18576677649696904, 67.96526564190969566, 12.55147014419179641 ) ) ;
#4283 = CIRCLE ( 'NONE', #19218, 9.084132297865673777 ) ;
#4284 = CARTESIAN_POINT ( 'NONE',  ( -15.56680656381426786, -6.886169722883741962, 19.08155846658118904 ) ) ;
#4285 = FACE_OUTER_BOUND ( 'NONE', #13846, .T. ) ;
#4286 = DIRECTION ( 'NONE',  ( -0.000000000000000000, -0.000000000000000000, 1.000000000000000000 ) ) ;
#4287 = CARTESIAN_POINT ( 'NONE',  ( 3.794966104483022296, 16.62713903700563378, 20.34789198813115263 ) ) ;
#4288 = DIRECTION ( 'NONE',  ( 1.000000000000000000, 4.440892098500625373E-15, 0.000000000000000000 ) ) ;
#4289 = FACE_OUTER_BOUND ( 'NONE', #22147, .T. ) ;
#4290 = CARTESIAN_POINT ( 'NONE',  ( 49.99999999999998579, 90.00000000000001421, 62.49999999999999289 ) ) ;
#4291 = CIRCLE ( 'NONE', #20236, 32.50000000000000000 ) ;
#4292 = ORIENTED_EDGE ( 'NONE', *, *, #17776, .T. ) ;
#4293 = ORIENTED_EDGE ( 'NONE', *, *, #15692, .F. ) ;
#4294 = CARTESIAN_POINT ( 'NONE',  ( -28.79137815760242702, -9.331429872129930914, -1.500000000000000000 ) ) ;
#4295 = AXIS2_PLACEMENT_3D ( 'NONE', #7686, #7532, #7376 ) ;
#4296 = CARTESIAN_POINT ( 'NONE',  ( -2.687479363073305372, 44.39187623477332068, -19.50000000000000355 ) ) ;
#4297 = DIRECTION ( 'NONE',  ( 1.000000000000000000, 0.000000000000000000, 0.000000000000000000 ) ) ;
#4298 = ORIENTED_EDGE ( 'NONE', *, *, #24131, .F. ) ;
#4299 = CARTESIAN_POINT ( 'NONE',  ( 18.35115206909799923, -7.996681782469499566, 20.34789198813115263 ) ) ;
#4300 = CARTESIAN_POINT ( 'NONE',  ( 5.372849316406058229, 19.28330981562107027, 5.653912893140659257 ) ) ;
#4301 = AXIS2_PLACEMENT_3D ( 'NONE', #1613, #27653, #25148 ) ;
#4302 = ORIENTED_EDGE ( 'NONE', *, *, #18529, .T. ) ;
#4303 = CARTESIAN_POINT ( 'NONE',  ( -19.84673203616234716, 2.611426761413839781, 5.657991946698900598 ) ) ;
#4304 = AXIS2_PLACEMENT_3D ( 'NONE', #19915, #17711, #10858 ) ;
#4305 = DIRECTION ( 'NONE',  ( 1.000000000000000000, 0.000000000000000000, -0.000000000000000000 ) ) ;
#4306 = VECTOR ( 'NONE', #20470, 1000.000000000000000 ) ;
#4307 = CARTESIAN_POINT ( 'NONE',  ( -18.92920200386403451, -38.99007567941009711, -16.50000000000000000 ) ) ;
#4308 = CARTESIAN_POINT ( 'NONE',  ( -10.19388640336980068, 41.04980642620002840, 28.96642789899617298 ) ) ;
#4309 = ORIENTED_EDGE ( 'NONE', *, *, #23142, .F. ) ;
#4310 = DIRECTION ( 'NONE',  ( -0.000000000000000000, -0.000000000000000000, 1.000000000000000000 ) ) ;
#4311 = B_SPLINE_CURVE_WITH_KNOTS ( 'NONE', 3,
 ( #10305, #19822, #5118, #26332, #28979, #5270, #2305 ),
 .UNSPECIFIED., .F., .F.,
 ( 4, 3, 4 ),
 ( 0.000000000000000000, 0.005028111721475434122, 0.01005622344647096392 ),
 .UNSPECIFIED. ) ;
#4312 = CARTESIAN_POINT ( 'NONE',  ( -8.072557715923444732, 14.41080185948837311, -0.6213203435596476032 ) ) ;
#4313 = DIRECTION ( 'NONE',  ( 1.000000000000000000, 0.000000000000000000, 0.000000000000000000 ) ) ;
#4314 = EDGE_CURVE ( 'NONE', #30397, #21299, #27759, .T. ) ;
#4315 = AXIS2_PLACEMENT_3D ( 'NONE', #6599, #16415, #25927 ) ;
#4316 = ORIENTED_EDGE ( 'NONE', *, *, #24326, .F. ) ;
#4317 = EDGE_CURVE ( 'NONE', #16098, #16473, #6136, .T. ) ;
#4318 = VECTOR ( 'NONE', #22725, 1000.000000000000000 ) ;
#4319 = CARTESIAN_POINT ( 'NONE',  ( 4.049916833591939103, 16.55712665779026693, 20.34789198813115263 ) ) ;
#4320 = DIRECTION ( 'NONE',  ( -0.4154150130018864351, 0.9096319953545184411, 0.000000000000000000 ) ) ;
#4321 = FACE_OUTER_BOUND ( 'NONE', #25208, .T. ) ;
#4322 = CARTESIAN_POINT ( 'NONE',  ( -0.6368756358441494125, -20.00777098345651339, 6.864725433338323413 ) ) ;
#4323 = AXIS2_PLACEMENT_3D ( 'NONE', #5483, #3143, #8135 ) ;
#4324 = CARTESIAN_POINT ( 'NONE',  ( -35.37867965644041135, 9.545149127882528772E-15, 35.37867965644034740 ) ) ;
#4325 = VECTOR ( 'NONE', #2242, 1000.000000000000000 ) ;
#4326 = DIRECTION ( 'NONE',  ( -1.000000000000000000, 0.000000000000000000, 0.000000000000000000 ) ) ;
#4327 = CARTESIAN_POINT ( 'NONE',  ( -17.05413688332568256, 0.7966627085705066946, 19.89182036555910571 ) ) ;
#4328 = CARTESIAN_POINT ( 'NONE',  ( -4.163336342344337027E-14, 1.387778780781445676E-14, 24.50000000000000000 ) ) ;
#4329 = ORIENTED_EDGE ( 'NONE', *, *, #30067, .F. ) ;
#4330 = CIRCLE ( 'NONE', #21760, 6.000000000000005329 ) ;
#4331 = CARTESIAN_POINT ( 'NONE',  ( 10.69412491129097553, -13.31565357151864859, 19.25672174529527325 ) ) ;
#4332 = CIRCLE ( 'NONE', #24257, 1.447898107987198646 ) ;
#4333 = CARTESIAN_POINT ( 'NONE',  ( 2.338573377552013888, -39.50000000000001421, 34.80090346875810070 ) ) ;
#4334 = EDGE_LOOP ( 'NONE', ( #11368, #25411, #409, #25739 ) ) ;
#4335 = ORIENTED_EDGE ( 'NONE', *, *, #28125, .F. ) ;
#4336 = CARTESIAN_POINT ( 'NONE',  ( -49.37764993206276642, 69.99068904741281472, 55.98768320531517872 ) ) ;
#4337 =( NAMED_UNIT ( * ) SI_UNIT ( $, .STERADIAN. ) SOLID_ANGLE_UNIT ( ) );
#4338 = ORIENTED_EDGE ( 'NONE', *, *, #17404, .F. ) ;
#4339 = AXIS2_PLACEMENT_3D ( 'NONE', #16684, #26506, #21185 ) ;
#4340 = CYLINDRICAL_SURFACE ( 'NONE', #24606, 2.000000000000001776 ) ;
#4341 = CARTESIAN_POINT ( 'NONE',  ( 23.15418787629628739, 10.94208358504856804, 49.39104550112972447 ) ) ;
#4342 = ORIENTED_EDGE ( 'NONE', *, *, #28074, .F. ) ;
#4343 = CARTESIAN_POINT ( 'NONE',  ( 37.99999999999999289, 80.00000000000000000, 0.000000000000000000 ) ) ;
#4344 = AXIS2_PLACEMENT_3D ( 'NONE', #4051, #13872, #23374 ) ;
#4345 = LINE ( 'NONE', #11535, #19465 ) ;
#4346 = EDGE_LOOP ( 'NONE', ( #5689, #11400, #10833, #14682 ) ) ;
#4347 = AXIS2_PLACEMENT_3D ( 'NONE', #15874, #16484, #30657 ) ;
#4348 = EDGE_LOOP ( 'NONE', ( #8219, #11418, #25052, #23025 ) ) ;
#4349 = DIRECTION ( 'NONE',  ( -0.000000000000000000, -0.000000000000000000, 1.000000000000000000 ) ) ;
#4350 = AXIS2_PLACEMENT_3D ( 'NONE', #13291, #27633, #18117 ) ;
#4351 = ORIENTED_EDGE ( 'NONE', *, *, #10466, .T. ) ;
#4352 = ORIENTED_EDGE ( 'NONE', *, *, #27680, .T. ) ;
#4353 = VECTOR ( 'NONE', #18024, 1000.000000000000000 ) ;
#4354 = CARTESIAN_POINT ( 'NONE',  ( 22.58267429318970443, -26.57182937991349903, 24.50000000000000000 ) ) ;
#4355 = CARTESIAN_POINT ( 'NONE',  ( 0.5197766397930339011, -17.03069205084988269, 18.37259980046033903 ) ) ;
#4356 = AXIS2_PLACEMENT_3D ( 'NONE', #16520, #23385, #2322 ) ;
#4357 = VECTOR ( 'NONE', #15370, 1000.000000000000000 ) ;
#4358 = CARTESIAN_POINT ( 'NONE',  ( -34.13832859401785669, -12.80067323710187921, 27.49999999999998934 ) ) ;
#4359 = CARTESIAN_POINT ( 'NONE',  ( 20.71335220384823117, -27.86167394782616213, -16.50000600000000262 ) ) ;
#4360 = CARTESIAN_POINT ( 'NONE',  ( -28.34828976096172681, -29.18752572968383419, 1.500000000000000000 ) ) ;
#4361 = VERTEX_POINT ( 'NONE', #29864 ) ;
#4362 = B_SPLINE_CURVE_WITH_KNOTS ( 'NONE', 3,
 ( #22847, #15985, #6164, #8667, #25805, #11308, #13947, #1497, #20945, #15827, #4437, #2082, #6475, #8809, #23141, #30027 ),
 .UNSPECIFIED., .F., .F.,
 ( 4, 2, 2, 2, 2, 2, 2, 4 ),
 ( 2.980374332640320740E-07, 0.0009280375596593464730, 0.001391907320772394928, 0.001855777081885443165, 0.002319646842998491186, 0.002783516604111547447, 0.003247386365224603274, 0.003711256126337659968 ),
 .UNSPECIFIED. ) ;
#4364 = B_SPLINE_CURVE_WITH_KNOTS ( 'NONE', 3,
 ( #18354, #10705, #13675, #18194, #30349, #17895 ),
 .UNSPECIFIED., .F., .F.,
 ( 4, 2, 4 ),
 ( 2.380730968221991799E-07, 0.002629065763328360898, 0.005257893453559900170 ),
 .UNSPECIFIED. ) ;
#4363 = DIRECTION ( 'NONE',  ( 0.3598999890241668664, -0.9329908884337534403, 0.000000000000000000 ) ) ;
#4365 = CARTESIAN_POINT ( 'NONE',  ( -4.375757216953428294E-15, -39.50000000000000000, 34.49999999999999289 ) ) ;
#4366 = VECTOR ( 'NONE', #11189, 1000.000000000000114 ) ;
#4367 = FACE_OUTER_BOUND ( 'NONE', #20653, .T. ) ;
#4368 = CARTESIAN_POINT ( 'NONE',  ( 3.826954525806321339, 16.61697297626111336, 18.37415474056476938 ) ) ;
#4369 = EDGE_LOOP ( 'NONE', ( #25058, #111, #24453, #3394 ) ) ;
#4370 = ORIENTED_EDGE ( 'NONE', *, *, #15083, .F. ) ;
#4371 = AXIS2_PLACEMENT_3D ( 'NONE', #25035, #12733, #24892 ) ;
#4372 = FACE_OUTER_BOUND ( 'NONE', #27020, .T. ) ;
#4373 = CARTESIAN_POINT ( 'NONE',  ( 10.52757208841436309, -13.43854510675287983, 6.037360021877314686 ) ) ;
#4374 = DIRECTION ( 'NONE',  ( 0.000000000000000000, 0.000000000000000000, -1.000000000000000000 ) ) ;
#4375 = DIRECTION ( 'NONE',  ( 0.000000000000000000, 0.000000000000000000, 1.000000000000000000 ) ) ;
#4376 = DIRECTION ( 'NONE',  ( -1.000000000000000000, 0.000000000000000000, -0.000000000000000000 ) ) ;
#4377 = B_SPLINE_CURVE_WITH_KNOTS ( 'NONE', 3,
 ( #23766, #14427, #24231, #7097, #24080, #17221, #2730, #28930, #11771, #16919, #2419, #379, #28619, #9592, #14248, #19103, #530, #12091 ),
 .UNSPECIFIED., .F., .F.,
 ( 4, 2, 2, 2, 2, 2, 2, 2, 4 ),
 ( 0.000000000000000000, 0.0003967869494442860957, 0.0007935738988885721913, 0.001190360848332858287, 0.001587147797777144383, 0.001983934747221430261, 0.002380721696665716574, 0.002777508646110002886, 0.003174295595554288765 ),
 .UNSPECIFIED. ) ;
#4378 = LINE ( 'NONE', #20906, #7453 ) ;
#4379 = AXIS2_PLACEMENT_3D ( 'NONE', #26165, #16192, #11528 ) ;
#4380 = ORIENTED_EDGE ( 'NONE', *, *, #24844, .T. ) ;
#4381 = AXIS2_PLACEMENT_3D ( 'NONE', #25852, #16026, #23346 ) ;
#4382 = CARTESIAN_POINT ( 'NONE',  ( -19.91121867491064279, 2.064381093144387780, 7.559636331181775581 ) ) ;
#4383 = CIRCLE ( 'NONE', #21814, 7.500000000000000000 ) ;
#4384 = CARTESIAN_POINT ( 'NONE',  ( 14.27661992934219626, 14.00645734016342736, 19.85730954408916915 ) ) ;
#4385 = CARTESIAN_POINT ( 'NONE',  ( 39.52380524533145945, -7.028748154382047808, -6.500000000000000888 ) ) ;
#4386 = ORIENTED_EDGE ( 'NONE', *, *, #11639, .F. ) ;
#4387 = EDGE_CURVE ( 'NONE', #7648, #29438, #22657, .T. ) ;
#4388 = VERTEX_POINT ( 'NONE', #5836 ) ;
#4389 = EDGE_CURVE ( 'NONE', #28571, #3416, #5320, .T. ) ;
#4390 = DIRECTION ( 'NONE',  ( -0.000000000000000000, 0.000000000000000000, -1.000000000000000000 ) ) ;
#4391 = VECTOR ( 'NONE', #7705, 1000.000000000000227 ) ;
#4392 = CARTESIAN_POINT ( 'NONE',  ( 0.000000000000000000, 0.000000000000000000, 1.500000000000001332 ) ) ;
#4393 = ORIENTED_EDGE ( 'NONE', *, *, #7277, .T. ) ;
#4394 = CARTESIAN_POINT ( 'NONE',  ( 31.61035137122363636, -19.06714716585487679, 27.50000000000000355 ) ) ;
#4395 = ADVANCED_FACE ( 'NONE', ( #25157 ), #17381, .F. ) ;
#4396 = CARTESIAN_POINT ( 'NONE',  ( -19.62935297797563905, -3.832558109936532009, 24.50000000000000000 ) ) ;
#4397 = ADVANCED_FACE ( 'NONE', ( #24540 ), #3188, .F. ) ;
#4398 = DIRECTION ( 'NONE',  ( -1.000000000000000000, 0.000000000000000000, 0.000000000000000000 ) ) ;
#4399 = CYLINDRICAL_SURFACE ( 'NONE', #20325, 2.061368542273053883 ) ;
#4400 = CARTESIAN_POINT ( 'NONE',  ( -6.294089901980526314, 15.86740633010675161, 19.97651184436794125 ) ) ;
#4401 = CARTESIAN_POINT ( 'NONE',  ( -32.19782014694307293, 14.25394737442115733, -16.55003854064094426 ) ) ;
#4402 = CARTESIAN_POINT ( 'NONE',  ( 33.56327786402394509, -10.57885966092500674, 39.80973752444699443 ) ) ;
#4403 = ORIENTED_EDGE ( 'NONE', *, *, #7857, .F. ) ;
#4404 = EDGE_CURVE ( 'NONE', #12912, #19716, #19764, .T. ) ;
#4405 = ORIENTED_EDGE ( 'NONE', *, *, #28416, .T. ) ;
#4406 = ADVANCED_FACE ( 'NONE', ( #15174 ), #8178, .T. ) ;
#4407 = AXIS2_PLACEMENT_3D ( 'NONE', #11659, #4639, #25700 ) ;
#4408 = CARTESIAN_POINT ( 'NONE',  ( 13.22505861668094340, 42.10773672057246841, -19.50000000000000355 ) ) ;
#4409 = CARTESIAN_POINT ( 'NONE',  ( 0.000000000000000000, 13.00000000000001421, 24.50000000000000000 ) ) ;
#4410 = ORIENTED_EDGE ( 'NONE', *, *, #12035, .F. ) ;
#4411 = DIRECTION ( 'NONE',  ( -0.000000000000000000, 0.000000000000000000, 1.000000000000000000 ) ) ;
#4412 = EDGE_CURVE ( 'NONE', #10675, #30448, #6746, .T. ) ;
#4413 = CARTESIAN_POINT ( 'NONE',  ( -14.72704883620385630, -8.644027383692558075, 19.03762469184452755 ) ) ;
#4414 = CARTESIAN_POINT ( 'NONE',  ( -10.11202017158235833, -41.14070756921188377, -1.500000000000000000 ) ) ;
#4415 = FACE_OUTER_BOUND ( 'NONE', #28711, .T. ) ;
#4416 = AXIS2_PLACEMENT_3D ( 'NONE', #20527, #10562, #1358 ) ;
#4417 = VERTEX_POINT ( 'NONE', #18758 ) ;
#4418 = DIRECTION ( 'NONE',  ( -1.000000000000000000, 0.000000000000000000, 0.000000000000000000 ) ) ;
#4419 = DIRECTION ( 'NONE',  ( -1.000000000000000000, 0.000000000000000000, 1.369518533665900065E-16 ) ) ;
#4420 = CARTESIAN_POINT ( 'NONE',  ( 14.71494672776318957, -39.36570965915668552, 29.11934627781901952 ) ) ;
#4421 = CARTESIAN_POINT ( 'NONE',  ( -6.737892368765494133, 18.83108299337147784, 7.272192800924337952 ) ) ;
#4422 = ORIENTED_EDGE ( 'NONE', *, *, #1182, .F. ) ;
#4423 = PLANE ( 'NONE',  #21066 ) ;
#4424 = VERTEX_POINT ( 'NONE', #6456 ) ;
#4425 = CARTESIAN_POINT ( 'NONE',  ( 24.35970437652574105, 13.37404834226503958, -16.55003854064094426 ) ) ;
#4426 = CARTESIAN_POINT ( 'NONE',  ( 127.5000000000000000, 0.000000000000000000, 0.000000000000000000 ) ) ;
#4427 = ADVANCED_FACE ( 'NONE', ( #4249 ), #6903, .F. ) ;
#4428 = ORIENTED_EDGE ( 'NONE', *, *, #11577, .F. ) ;
#4429 = ADVANCED_FACE ( 'NONE', ( #18306 ), #16112, .F. ) ;
#4430 = PRODUCT ( 'Slotted Rotor Drive Shaft', 'Slotted Rotor Drive Shaft', '', ( #9606 ) ) ;
#4431 = ADVANCED_FACE ( 'NONE', ( #1915 ), #9240, .T. ) ;
#4432 = VECTOR ( 'NONE', #465, 1000.000000000000000 ) ;
#4433 = VECTOR ( 'NONE', #9673, 1000.000000000000000 ) ;
#4434 = EDGE_CURVE ( 'NONE', #9450, #2272, #25252, .T. ) ;
#4435 = CARTESIAN_POINT ( 'NONE',  ( 16.55527708515955609, 4.194179076328807376, 19.28454053338348473 ) ) ;
#4436 = VERTEX_POINT ( 'NONE', #11440 ) ;
#4437 = CARTESIAN_POINT ( 'NONE',  ( -31.57476163834523675, -15.10795358447669301, 39.99718304312881401 ) ) ;
#4438 = EDGE_CURVE ( 'NONE', #6357, #10933, #11798, .T. ) ;
#4439 = CARTESIAN_POINT ( 'NONE',  ( -8.361245565923718814, -14.86101098545373489, 7.627891251804737927 ) ) ;
#4440 = FACE_OUTER_BOUND ( 'NONE', #27615, .T. ) ;
#4441 = AXIS2_PLACEMENT_3D ( 'NONE', #15620, #20461, #29981 ) ;
#4442 = CARTESIAN_POINT ( 'NONE',  ( 0.8870900849372836960, -19.99803318816115549, 20.19593175699879595 ) ) ;
#4443 = ORIENTED_EDGE ( 'NONE', *, *, #19075, .F. ) ;
#4444 = ADVANCED_FACE ( 'NONE', ( #21076 ), #28121, .F. ) ;
#4445 = DIRECTION ( 'NONE',  ( 0.000000000000000000, 0.000000000000000000, 1.000000000000000000 ) ) ;
#4446 = CARTESIAN_POINT ( 'NONE',  ( 12.53055695656588497, 11.54555247029844800, 18.37259980046034613 ) ) ;
#4447 = CARTESIAN_POINT ( 'NONE',  ( 39.99999999999998579, 87.00000000000001421, 52.49999999999999289 ) ) ;
#4448 = CARTESIAN_POINT ( 'NONE',  ( -9.216505592218814158, -7.781333699927420966, 1.500000000000000000 ) ) ;
#4449 = EDGE_CURVE ( 'NONE', #21250, #27848, #15964, .T. ) ;
#4450 = EDGE_LOOP ( 'NONE', ( #12033, #25018, #12184, #29434 ) ) ;
#4451 = LINE ( 'NONE', #16300, #1331 ) ;
#4452 = AXIS2_PLACEMENT_3D ( 'NONE', #20719, #27769, #15916 ) ;
#4453 = CARTESIAN_POINT ( 'NONE',  ( 25.47847050916411504, 26.57182937991349903, -1.500000000000001332 ) ) ;
#4454 = CARTESIAN_POINT ( 'NONE',  ( -12.73345385815705555, 11.29622791819166494, 19.60617949693493500 ) ) ;
#4455 = DIRECTION ( 'NONE',  ( 0.000000000000000000, 0.000000000000000000, 1.000000000000000000 ) ) ;
#4456 = CARTESIAN_POINT ( 'NONE',  ( 3.062271323958273950, 16.80150817659525231, 19.47952243369111258 ) ) ;
#4457 = CARTESIAN_POINT ( 'NONE',  ( -18.04365185506137337, -8.627086862512673093, 7.652108011868850035 ) ) ;
#4458 = CARTESIAN_POINT ( 'NONE',  ( -18.47553274370957155, -7.705290464775618631, 19.33715507985239412 ) ) ;
#4459 = PLANE ( 'NONE',  #20543 ) ;
#4460 = CIRCLE ( 'NONE', #29856, 9.084132297865673777 ) ;
#4461 = ORIENTED_EDGE ( 'NONE', *, *, #16791, .T. ) ;
#4462 = DIRECTION ( 'NONE',  ( -0.000000000000000000, -0.000000000000000000, 1.000000000000000000 ) ) ;
#4463 = CARTESIAN_POINT ( 'NONE',  ( 39.00000000000000000, -5.563236990218592304, -1.500000000000000000 ) ) ;
#4464 = EDGE_CURVE ( 'NONE', #20151, #29358, #14278, .T. ) ;
#4465 = CARTESIAN_POINT ( 'NONE',  ( 14.89473990422475680, -17.79239818699420539, 1.500000000000000000 ) ) ;
#4466 = VERTEX_POINT ( 'NONE', #25634 ) ;
#4467 = DIRECTION ( 'NONE',  ( 0.000000000000000000, 0.000000000000000000, -1.000000000000000000 ) ) ;
#4468 = EDGE_CURVE ( 'NONE', #12485, #24910, #2328, .T. ) ;
#4469 = B_SPLINE_CURVE_WITH_KNOTS ( 'NONE', 1,
 ( #9085, #28113 ),
 .UNSPECIFIED., .F., .F.,
 ( 2, 2 ),
 ( 0.1666666666666667962, 1.000000000000000000 ),
 .UNSPECIFIED. ) ;
#4470 = AXIS2_PLACEMENT_3D ( 'NONE', #28446, #18328, #30465 ) ;
#4471 = CARTESIAN_POINT ( 'NONE',  ( 15.38564065975359796, -7.280544306537534816, 19.45164628100866722 ) ) ;
#4472 = CARTESIAN_POINT ( 'NONE',  ( 5.997818345539172924, 19.09841206584651729, 7.359006845440219102 ) ) ;
#4473 = EDGE_CURVE ( 'NONE', #24171, #17300, #24729, .T. ) ;
#4474 = ORIENTED_EDGE ( 'NONE', *, *, #12980, .F. ) ;
#4475 = CARTESIAN_POINT ( 'NONE',  ( -16.81263688882342322, 2.656251026639211421, 6.641371103590088865 ) ) ;
#4476 = CARTESIAN_POINT ( 'NONE',  ( 24.03057240117690441, -26.57182937991349903, -6.499999999999999112 ) ) ;
#4477 = CARTESIAN_POINT ( 'NONE',  ( -16.16747268278624716, -40.42849113817944584, -16.49999999999999645 ) ) ;
#4478 = CARTESIAN_POINT ( 'NONE',  ( -37.02637947441376554, 5.976920169802977689, 37.50000000003053913 ) ) ;
#4479 = ORIENTED_EDGE ( 'NONE', *, *, #6561, .T. ) ;
#4480 = DIRECTION ( 'NONE',  ( -0.000000000000000000, -0.000000000000000000, -1.000000000000000000 ) ) ;
#4481 = CARTESIAN_POINT ( 'NONE',  ( -14.70303524442681997, -8.688445896238663479, 6.588756557121050683 ) ) ;
#4482 = CYLINDRICAL_SURFACE ( 'NONE', #18810, 0.7500000000000006661 ) ;
#4483 = ORIENTED_EDGE ( 'NONE', *, *, #3470, .F. ) ;
#4484 = CARTESIAN_POINT ( 'NONE',  ( 16.86471733739940859, 2.322843836249472105, 18.83976166372255179 ) ) ;
#4485 = CARTESIAN_POINT ( 'NONE',  ( 24.85846090629200589, -6.933313039714902537, 44.95040115368828992 ) ) ;
#4486 = CARTESIAN_POINT ( 'NONE',  ( 21.14511335159655658, -37.62126931545598296, -16.50000000000000000 ) ) ;
#4487 = CARTESIAN_POINT ( 'NONE',  ( 0.1433833641520070590, -17.02852539342428884, 7.429667576816606278 ) ) ;
#4488 = VECTOR ( 'NONE', #29638, 1000.000000000000000 ) ;
#4489 = DIRECTION ( 'NONE',  ( 1.000000000000000000, 0.000000000000000000, 0.000000000000000000 ) ) ;
#4490 = DIRECTION ( 'NONE',  ( 0.000000000000000000, 0.000000000000000000, -1.000000000000000000 ) ) ;
#4491 = CARTESIAN_POINT ( 'NONE',  ( -19.87893182697125027, 2.354587536660440072, 20.33971507717571114 ) ) ;
#4492 = CARTESIAN_POINT ( 'NONE',  ( -10.47960520055065636, -7.757439966934454034, 24.50000000000000000 ) ) ;
#4493 = ORIENTED_EDGE ( 'NONE', *, *, #2912, .T. ) ;
#4494 = CIRCLE ( 'NONE', #7982, 0.7500000000000011102 ) ;
#4495 = CARTESIAN_POINT ( 'NONE',  ( 11.94600218753717868, -16.06231219995582293, 19.36813350477385143 ) ) ;
#4496 = CARTESIAN_POINT ( 'NONE',  ( -5.881244434206279514, -6.812559277181949646, -3.621320343559650379 ) ) ;
#4497 = VERTEX_POINT ( 'NONE', #22823 ) ;
#4498 = ORIENTED_EDGE ( 'NONE', *, *, #20279, .T. ) ;
#4499 = CARTESIAN_POINT ( 'NONE',  ( -15.34307810681595718, 12.82926163924266483, 7.652108011868850035 ) ) ;
#4500 = ADVANCED_FACE ( 'NONE', ( #13487 ), #1474, .F. ) ;
#4501 = CARTESIAN_POINT ( 'NONE',  ( 8.099999999999999645, 0.000000000000000000, 0.000000000000000000 ) ) ;
#4502 = VERTEX_POINT ( 'NONE', #27662 ) ;
#4503 = DIRECTION ( 'NONE',  ( 1.156482317317871725E-15, 1.000000000000000000, 0.000000000000000000 ) ) ;
#4504 = PLANE ( 'NONE',  #22888 ) ;
#4505 = VERTEX_POINT ( 'NONE', #11134 ) ;
#4506 = CIRCLE ( 'NONE', #25445, 7.500000000000000000 ) ;
#4507 = CARTESIAN_POINT ( 'NONE',  ( -24.85846090629201299, 6.933313039714896320, 49.19304184080765907 ) ) ;
#4508 = ORIENTED_EDGE ( 'NONE', *, *, #27657, .T. ) ;
#4509 = LINE ( 'NONE', #23664, #3372 ) ;
#4510 = EDGE_LOOP ( 'NONE', ( #26970, #16542, #29849, #25228 ) ) ;
#4511 = DIRECTION ( 'NONE',  ( 1.000000000000000000, 0.000000000000000000, 0.000000000000000000 ) ) ;
#4512 = VERTEX_POINT ( 'NONE', #25323 ) ;
#4513 = VERTEX_POINT ( 'NONE', #4106 ) ;
#4514 = DIRECTION ( 'NONE',  ( -0.000000000000000000, -0.000000000000000000, -1.000000000000000000 ) ) ;
#4515 = CARTESIAN_POINT ( 'NONE',  ( -17.68050765791475243, -9.349252870402523286, 7.272192800924347722 ) ) ;
#4516 = CARTESIAN_POINT ( 'NONE',  ( 19.72232476070952956, 3.323723214581396412, 7.652108011868850923 ) ) ;
#4517 = FACE_BOUND ( 'NONE', #19816, .T. ) ;
#4518 = VERTEX_POINT ( 'NONE', #18610 ) ;
#4519 = CARTESIAN_POINT ( 'NONE',  ( -16.96555893295483841, 1.647560171216679192, 18.34798005862930381 ) ) ;
#4520 = CARTESIAN_POINT ( 'NONE',  ( 32.98805937973592961, -22.67054169308934064, 18.00000000000000000 ) ) ;
#4521 = AXIS2_PLACEMENT_3D ( 'NONE', #14643, #12939, #2794 ) ;
#4522 = CARTESIAN_POINT ( 'NONE',  ( -13.77701868333376645, 10.07013474916661266, 7.441806358946449151 ) ) ;
#4523 = CARTESIAN_POINT ( 'NONE',  ( 10.50506478158603407, 13.32952022457704544, 1.500000000000000000 ) ) ;
#4524 = ORIENTED_EDGE ( 'NONE', *, *, #5364, .T. ) ;
#4525 = ORIENTED_EDGE ( 'NONE', *, *, #21854, .F. ) ;
#4526 = CARTESIAN_POINT ( 'NONE',  ( -8.840471615930058036, 1.687027447297517080, 21.50000000000000000 ) ) ;
#4527 = PLANE ( 'NONE',  #12134 ) ;
#4528 = FACE_OUTER_BOUND ( 'NONE', #20639, .T. ) ;
#4529 = CARTESIAN_POINT ( 'NONE',  ( -23.08950671686661948, 11.27322061222802851, 45.06306679229680157 ) ) ;
#4530 = ADVANCED_FACE ( 'NONE', ( #13638 ), #23118, .F. ) ;
#4531 = CARTESIAN_POINT ( 'NONE',  ( -26.45199234830066004, 26.79642899342907825, 27.50000000000000355 ) ) ;
#4532 = CARTESIAN_POINT ( 'NONE',  ( 0.000000000000000000, 65.00000000000000000, 50.49999999999998579 ) ) ;
#4533 = ORIENTED_EDGE ( 'NONE', *, *, #15839, .T. ) ;
#4534 = CARTESIAN_POINT ( 'NONE',  ( -19.93913687200723572, 1.772791844786496762, 5.951255046771932733 ) ) ;
#4535 = CARTESIAN_POINT ( 'NONE',  ( -5.687793815610304726, 6.974883619896852238, -1.500000000000000888 ) ) ;
#4536 = CARTESIAN_POINT ( 'NONE',  ( 19.78337026033622337, 2.938244205458798941, 18.37250658438899009 ) ) ;
#4537 = ORIENTED_EDGE ( 'NONE', *, *, #21177, .F. ) ;
#4538 = LINE ( 'NONE', #5308, #1858 ) ;
#4539 = VERTEX_POINT ( 'NONE', #30151 ) ;
#4540 = CARTESIAN_POINT ( 'NONE',  ( 15.87456320658224485, -6.220724357885995204, 5.661398277488801867 ) ) ;
#4541 = AXIS2_PLACEMENT_3D ( 'NONE', #7484, #27125, #5131 ) ;
#4542 = CARTESIAN_POINT ( 'NONE',  ( -11.30959556923743392, 42.34504995199416300, -16.50000000000000000 ) ) ;
#4543 = VERTEX_POINT ( 'NONE', #20776 ) ;
#4544 = CARTESIAN_POINT ( 'NONE',  ( 25.24607261983683060, -28.18396486040856530, 27.50000000000000355 ) ) ;
#4545 = CARTESIAN_POINT ( 'NONE',  ( -4.776122516674677878E-15, -42.50000000000000000, 24.50000000000000000 ) ) ;
#4546 = DIRECTION ( 'NONE',  ( 1.000000000000000000, 0.000000000000000000, -0.000000000000000000 ) ) ;
#4547 = AXIS2_PLACEMENT_3D ( 'NONE', #10799, #3945, #8482 ) ;
#4548 = CARTESIAN_POINT ( 'NONE',  ( -18.04365185506137337, -8.627086862512673093, 7.652108011868850035 ) ) ;
#4549 = CARTESIAN_POINT ( 'NONE',  ( -6.374050743166105981, 15.83881588044503808, 18.82680253904184298 ) ) ;
#4550 = LINE ( 'NONE', #23563, #29260 ) ;
#4551 = CARTESIAN_POINT ( 'NONE',  ( -10.00000000000004263, 1.387778780781445676E-14, -1.500000000000000000 ) ) ;
#4552 = CARTESIAN_POINT ( 'NONE',  ( 14.44122519041005859, -13.83658248990206729, 24.50000000000000000 ) ) ;
#4553 = ORIENTED_EDGE ( 'NONE', *, *, #9784, .T. ) ;
#4554 = CIRCLE ( 'NONE', #28965, 11.46182693247435935 ) ;
#4555 = CARTESIAN_POINT ( 'NONE',  ( 42.49999999999998579, 50.00000000000000000, 12.49999999999999112 ) ) ;
#4556 = CARTESIAN_POINT ( 'NONE',  ( 20.65888525914559892, 38.75220717792412728, -19.50000000000000355 ) ) ;
#4557 = DIRECTION ( 'NONE',  ( -1.000000000000000000, 0.000000000000000000, 0.000000000000000000 ) ) ;
#4558 = EDGE_CURVE ( 'NONE', #18898, #2369, #8951, .T. ) ;
#4559 = ORIENTED_EDGE ( 'NONE', *, *, #5602, .T. ) ;
#4560 = CARTESIAN_POINT ( 'NONE',  ( 0.000000000000000000, 0.000000000000000000, 1.500000000000001332 ) ) ;
#4561 = CARTESIAN_POINT ( 'NONE',  ( -14.71441417907128013, -8.667509008793198078, 19.58863275299554019 ) ) ;
#4562 = CARTESIAN_POINT ( 'NONE',  ( -25.07950435457407323, 11.50806656539752737, -16.55003854064094426 ) ) ;
#4563 = PRODUCT_RELATED_PRODUCT_CATEGORY ( 'part', '', ( #23856 ) ) ;
#4564 =( NAMED_UNIT ( * ) SI_UNIT ( $, .STERADIAN. ) SOLID_ANGLE_UNIT ( ) );
#4565 = AXIS2_PLACEMENT_3D ( 'NONE', #1195, #10700, #8213 ) ;
#4566 = FACE_OUTER_BOUND ( 'NONE', #26121, .T. ) ;
#4567 = ORIENTED_EDGE ( 'NONE', *, *, #25632, .F. ) ;
#4568 = CARTESIAN_POINT ( 'NONE',  ( 12.72536390617885438, -2.839914339433650348, 1.500000000000001332 ) ) ;
#4569 = DIRECTION ( 'NONE',  ( -1.000000000000000000, 0.000000000000000000, 0.000000000000000000 ) ) ;
#4570 = CARTESIAN_POINT ( 'NONE',  ( 13.83399314246956813, -39.74420824290464793, 34.55195916885559626 ) ) ;
#4571 = EDGE_CURVE ( 'NONE', #19951, #10643, #12792, .T. ) ;
#4572 = CARTESIAN_POINT ( 'NONE',  ( 42.49999999999998579, -50.00000000000000000, 62.49999999999999289 ) ) ;
#4573 = VERTEX_POINT ( 'NONE', #16718 ) ;
#4574 = FACE_OUTER_BOUND ( 'NONE', #5111, .T. ) ;
#4575 = CARTESIAN_POINT ( 'NONE',  ( -19.64114023396299302, -37.13592150529018454, -1.500000000000000000 ) ) ;
#4576 = DIRECTION ( 'NONE',  ( 1.000000000000000000, 0.000000000000000000, 0.000000000000000000 ) ) ;
#4577 = VERTEX_POINT ( 'NONE', #21863 ) ;
#4578 = EDGE_LOOP ( 'NONE', ( #24122, #21961 ) ) ;
#4579 = DIRECTION ( 'NONE',  ( 0.000000000000000000, 0.000000000000000000, 1.000000000000000000 ) ) ;
#4580 = VECTOR ( 'NONE', #22281, 1000.000000000000000 ) ;
#4581 = VERTEX_POINT ( 'NONE', #17025 ) ;
#4582 = CARTESIAN_POINT ( 'NONE',  ( -0.6660349346848405405, -20.00682905350634400, 19.33715507985239412 ) ) ;
#4583 = ADVANCED_FACE ( 'NONE', ( #2215 ), #26228, .T. ) ;
#4584 = CARTESIAN_POINT ( 'NONE',  ( -10.52692686119061172, -17.02631563033162365, 7.652108011868850035 ) ) ;
#4585 = CIRCLE ( 'NONE', #19020, 12.50000000000000000 ) ;
#4586 = DIRECTION ( 'NONE',  ( 0.5503133621338236470, 0.8349582046168341209, 0.000000000000000000 ) ) ;
#4587 = CARTESIAN_POINT ( 'NONE',  ( 0.4984457374290387488, -20.01168570850558481, 20.33971507717571114 ) ) ;
#4588 = EDGE_LOOP ( 'NONE', ( #467, #6769, #28243, #8881 ) ) ;
#4589 = DIRECTION ( 'NONE',  ( -0.06975647374412530244, 0.000000000000000000, -0.9975640502598241977 ) ) ;
#4590 = FACE_OUTER_BOUND ( 'NONE', #28756, .T. ) ;
#4591 = CARTESIAN_POINT ( 'NONE',  ( 14.21537200517654398, 14.09360477215026108, 19.58863275299554019 ) ) ;
#4592 = CARTESIAN_POINT ( 'NONE',  ( 26.36764545593177544, -31.31467416275353344, 1.500000000000000000 ) ) ;
#4593 = EDGE_LOOP ( 'NONE', ( #24402, #19731, #27523, #18874 ) ) ;
#4594 = CARTESIAN_POINT ( 'NONE',  ( -15.22163550582783031, -7.663797071066537292, 20.34789198813115974 ) ) ;
#4595 = DIRECTION ( 'NONE',  ( 1.000000000000000000, 0.000000000000000000, 0.000000000000000000 ) ) ;
#4596 = CARTESIAN_POINT ( 'NONE',  ( 0.000000000000000000, -2.322405306613848348E-14, 117.5000000000000000 ) ) ;
#4597 = DIRECTION ( 'NONE',  ( -1.000000000000000000, 0.000000000000000000, 0.000000000000000000 ) ) ;
#4598 = DIRECTION ( 'NONE',  ( 1.000000000000000000, 0.000000000000000000, 0.000000000000000000 ) ) ;
#4599 = EDGE_CURVE ( 'NONE', #14232, #5487, #9545, .T. ) ;
#4600 = ADVANCED_FACE ( 'NONE', ( #24185 ), #23889, .F. ) ;
#4601 = AXIS2_PLACEMENT_3D ( 'NONE', #26016, #2612, #9323 ) ;
#4602 = DIRECTION ( 'NONE',  ( 1.000000000000000000, 0.000000000000000000, 0.000000000000000000 ) ) ;
#4603 = DIRECTION ( 'NONE',  ( 0.000000000000000000, 1.000000000000000000, 0.000000000000000000 ) ) ;
#4604 = ORIENTED_EDGE ( 'NONE', *, *, #4988, .F. ) ;
#4605 = ORIENTED_EDGE ( 'NONE', *, *, #27863, .F. ) ;
#4606 = FACE_OUTER_BOUND ( 'NONE', #1726, .T. ) ;
#4607 = EDGE_CURVE ( 'NONE', #549, #30256, #7842, .T. ) ;
#4608 = CARTESIAN_POINT ( 'NONE',  ( -5.374868878254082105, 44.10336124695542992, -19.50000000000000355 ) ) ;
#4609 = CARTESIAN_POINT ( 'NONE',  ( -37.99999999999999289, 209.2686044187655909, -81.50000000000000000 ) ) ;
#4610 = EDGE_CURVE ( 'NONE', #18893, #6285, #25275, .T. ) ;
#4611 = CARTESIAN_POINT ( 'NONE',  ( -14.36006998371493637, -17.26937953831884442, 1.500000000000000000 ) ) ;
#4612 = ORIENTED_EDGE ( 'NONE', *, *, #27152, .T. ) ;
#4613 = CARTESIAN_POINT ( 'NONE',  ( 0.000000000000000000, 0.000000000000000000, 0.000000000000000000 ) ) ;
#4614 = CARTESIAN_POINT ( 'NONE',  ( 18.21411928606760711, -8.304179478877907528, 20.29090034784956131 ) ) ;
#4615 = CARTESIAN_POINT ( 'NONE',  ( 6.270562923531074695, 19.01045013183040311, 6.755862304746362845 ) ) ;
#4616 = EDGE_CURVE ( 'NONE', #11338, #6047, #11733, .T. ) ;
#4617 = ADVANCED_FACE ( 'NONE', ( #7527 ), #19374, .T. ) ;
#4618 = ORIENTED_EDGE ( 'NONE', *, *, #6709, .F. ) ;
#4619 = CARTESIAN_POINT ( 'NONE',  ( 6.171684994647416822, 19.04275422834224329, 18.90679857307105749 ) ) ;
#4620 = CYLINDRICAL_SURFACE ( 'NONE', #10747, 0.7499999999999997780 ) ;
#4621 = CARTESIAN_POINT ( 'NONE',  ( -0.9307681286967910417, 9.436481611552762772, 1.500000000000001332 ) ) ;
#4622 = CARTESIAN_POINT ( 'NONE',  ( -36.61847497238780846, 14.68214248103183905, 31.56314805174072191 ) ) ;
#4623 = ORIENTED_EDGE ( 'NONE', *, *, #6175, .F. ) ;
#4624 = LINE ( 'NONE', #2911, #18830 ) ;
#4625 = EDGE_CURVE ( 'NONE', #21504, #5226, #7678, .T. ) ;
#4626 = CIRCLE ( 'NONE', #11618, 9.482273699623480212 ) ;
#4627 = CARTESIAN_POINT ( 'NONE',  ( 32.44940373544195467, 8.539989232413363496, 37.20300302271262183 ) ) ;
#4628 = DIRECTION ( 'NONE',  ( 1.000000000000000000, 0.000000000000000000, 0.000000000000000000 ) ) ;
#4629 = B_SPLINE_CURVE_WITH_KNOTS ( 'NONE', 3,
 ( #7522, #10012, #641, #10470, #24180, #10310 ),
 .UNSPECIFIED., .F., .F.,
 ( 4, 2, 4 ),
 ( 2.111164903090458206E-07, 0.0003706953849294946247, 0.0007411796533686801358 ),
 .UNSPECIFIED. ) ;
#4630 = ORIENTED_EDGE ( 'NONE', *, *, #21768, .F. ) ;
#4631 = CARTESIAN_POINT ( 'NONE',  ( -18.46427634282258268, -7.732205987805706116, 6.864725433338323413 ) ) ;
#4632 = CYLINDRICAL_SURFACE ( 'NONE', #23788, 0.7500000000000007772 ) ;
#4633 = CARTESIAN_POINT ( 'NONE',  ( 25.88604317058895532, -6.345278376181632041, 44.10533075955772375 ) ) ;
#4634 = CARTESIAN_POINT ( 'NONE',  ( 18.92760511682993751, -39.00287852246747633, -16.50000000000000711 ) ) ;
#4635 = FACE_BOUND ( 'NONE', #30165, .T. ) ;
#4636 = CARTESIAN_POINT ( 'NONE',  ( 27.03074382657074537, -6.449748410230991880, 47.21042702067962438 ) ) ;
#4637 = CARTESIAN_POINT ( 'NONE',  ( -32.28307784207223108, -8.475829241206275455, -16.55003854064094426 ) ) ;
#4638 = DIRECTION ( 'NONE',  ( 0.000000000000000000, 0.000000000000000000, 1.000000000000000000 ) ) ;
#4639 = DIRECTION ( 'NONE',  ( 0.000000000000000000, 0.000000000000000000, 1.000000000000000000 ) ) ;
#4640 = ORIENTED_EDGE ( 'NONE', *, *, #7718, .T. ) ;
#4641 = EDGE_CURVE ( 'NONE', #4182, #14649, #15809, .T. ) ;
#4642 = EDGE_CURVE ( 'NONE', #4182, #15053, #16558, .T. ) ;
#4643 = CARTESIAN_POINT ( 'NONE',  ( 11.86528446860017105, -16.12209958341615135, 19.79423548914561692 ) ) ;
#4644 = DIRECTION ( 'NONE',  ( -1.000000000000000000, -0.000000000000000000, -0.000000000000000000 ) ) ;
#4645 = VERTEX_POINT ( 'NONE', #2533 ) ;
#4646 = EDGE_CURVE ( 'NONE', #2167, #12762, #23762, .T. ) ;
#4647 = ORIENTED_EDGE ( 'NONE', *, *, #26147, .T. ) ;
#4648 = DIRECTION ( 'NONE',  ( -0.000000000000000000, -0.000000000000000000, 1.000000000000000000 ) ) ;
#4649 = VERTEX_POINT ( 'NONE', #26397 ) ;
#4650 = DIRECTION ( 'NONE',  ( 0.000000000000000000, 0.000000000000000000, 1.000000000000000000 ) ) ;
#4651 = ADVANCED_FACE ( 'NONE', ( #2372 ), #26076, .T. ) ;
#4652 = VERTEX_POINT ( 'NONE', #14061 ) ;
#4653 = CARTESIAN_POINT ( 'NONE',  ( 18.35307771382469255, -7.992233955150557456, 18.34798005862662507 ) ) ;
#4654 = CARTESIAN_POINT ( 'NONE',  ( 19.57285800138751952, 4.196195780087080607, 19.25672174529527325 ) ) ;
#4655 = DIRECTION ( 'NONE',  ( 1.000000000000000000, 0.000000000000000000, 0.000000000000000000 ) ) ;
#4656 = ORIENTED_EDGE ( 'NONE', *, *, #27078, .F. ) ;
#4657 = LINE ( 'NONE', #18417, #16309 ) ;
#4658 = ORIENTED_EDGE ( 'NONE', *, *, #21962, .F. ) ;
#4659 = VECTOR ( 'NONE', #5520, 1000.000000000000000 ) ;
#4660 = ORIENTED_EDGE ( 'NONE', *, *, #27298, .T. ) ;
#4661 = AXIS2_PLACEMENT_3D ( 'NONE', #2184, #28861, #23999 ) ;
#4662 = EDGE_CURVE ( 'NONE', #15798, #20585, #18798, .T. ) ;
#4663 = AXIS2_PLACEMENT_3D ( 'NONE', #29324, #7966, #26993 ) ;
#4664 = LINE ( 'NONE', #3243, #11611 ) ;
#4665 = DIRECTION ( 'NONE',  ( 0.000000000000000000, 0.000000000000000000, 1.000000000000000000 ) ) ;
#4666 = EDGE_CURVE ( 'NONE', #19456, #8889, #26030, .T. ) ;
#4667 = CARTESIAN_POINT ( 'NONE',  ( 0.8531715179115259007, -17.02613171184588126, 7.652108011868850035 ) ) ;
#4668 = CARTESIAN_POINT ( 'NONE',  ( -14.76455652123169138, -8.574248774011078211, 18.84329447212443753 ) ) ;
#4669 = CARTESIAN_POINT ( 'NONE',  ( -0.7220001660363114526, -9.454746441592957851, 21.50000000000000000 ) ) ;
#4670 = CARTESIAN_POINT ( 'NONE',  ( -43.34097750826428097, -11.89502811014148342, 1.500000000000000444 ) ) ;
#4671 = ORIENTED_EDGE ( 'NONE', *, *, #26545, .F. ) ;
#4672 = CARTESIAN_POINT ( 'NONE',  ( 9.860909911264739591, -13.90333503211347654, 7.652108011868850035 ) ) ;
#4673 = FACE_OUTER_BOUND ( 'NONE', #9260, .T. ) ;
#4674 = CARTESIAN_POINT ( 'NONE',  ( -13.87349289520722806, 9.945669722324359086, 7.280727868105637768 ) ) ;
#4675 = DIRECTION ( 'NONE',  ( 1.000000000000000000, 0.000000000000000000, 0.000000000000000000 ) ) ;
#4676 = VERTEX_POINT ( 'NONE', #33 ) ;
#4677 = VERTEX_POINT ( 'NONE', #2680 ) ;
#4678 = CARTESIAN_POINT ( 'NONE',  ( 40.05104235265675783, 2.353288714459732311, -11.49999999999999645 ) ) ;
#4679 = LINE ( 'NONE', #9514, #27590 ) ;
#4680 = DIRECTION ( 'NONE',  ( 0.8412535328311810945, 0.5406408174555976665, 0.000000000000000000 ) ) ;
#4681 = PRODUCT ( 'Double-Lip Hydraulic Vanes', 'Double-Lip Hydraulic Vanes', '', ( #28633 ) ) ;
#4682 = DIRECTION ( 'NONE',  ( 0.9594929736144951482, -0.2817325568414371095, 0.000000000000000000 ) ) ;
#4683 = CARTESIAN_POINT ( 'NONE',  ( -23.07950435457394889, 11.39182330144667432, 45.01971494674684493 ) ) ;
#4684 = DIRECTION ( 'NONE',  ( 0.000000000000000000, 0.000000000000000000, -1.000000000000000000 ) ) ;
#4685 = AXIS2_PLACEMENT_3D ( 'NONE', #850, #28781, #24399 ) ;
#4686 = CARTESIAN_POINT ( 'NONE',  ( -7.856594496258223259, -4.390207617113929039, 21.50000000000000000 ) ) ;
#4687 = ORIENTED_EDGE ( 'NONE', *, *, #4074, .F. ) ;
#4688 = CARTESIAN_POINT ( 'NONE',  ( -19.88720069594608475, 2.282442057551330450, 7.627891251804737927 ) ) ;
#4689 = DIRECTION ( 'NONE',  ( 0.000000000000000000, 0.000000000000000000, -1.000000000000000000 ) ) ;
#4690 = DIRECTION ( 'NONE',  ( 0.000000000000000000, 0.000000000000000000, -1.000000000000000000 ) ) ;
#4691 = VERTEX_POINT ( 'NONE', #27326 ) ;
#4692 = DIRECTION ( 'NONE',  ( 0.000000000000000000, 0.000000000000000000, 1.000000000000000000 ) ) ;
#4693 = VERTEX_POINT ( 'NONE', #20140 ) ;
#4694 = CARTESIAN_POINT ( 'NONE',  ( -25.64627119138473788, 23.40052582045089480, -6.500000000000000888 ) ) ;
#4695 = CARTESIAN_POINT ( 'NONE',  ( -0.5234333628969437546, 44.07381280400610279, -16.50000000000000711 ) ) ;
#4696 = ORIENTED_EDGE ( 'NONE', *, *, #17013, .F. ) ;
#4697 = CARTESIAN_POINT ( 'NONE',  ( 25.62842000332392800, 27.74319361490436009, 27.50000000000001421 ) ) ;
#4698 = CARTESIAN_POINT ( 'NONE',  ( 1.868132521858655084E-15, 50.00000000000000000, -40.00000000000000711 ) ) ;
#4699 = CARTESIAN_POINT ( 'NONE',  ( -17.79239818699324616, -14.89473990422481187, 1.500000000000000000 ) ) ;
#4700 = CARTESIAN_POINT ( 'NONE',  ( -18.30120037456298832, -8.066899270990512960, 5.849008070840539197 ) ) ;
#4701 = EDGE_CURVE ( 'NONE', #2298, #17387, #7332, .T. ) ;
#4702 = B_SPLINE_CURVE_WITH_KNOTS ( 'NONE', 3,
 ( #6446, #16107, #3960, #6594 ),
 .UNSPECIFIED., .F., .F.,
 ( 4, 4 ),
 ( 2.143643656964903641E-07, 0.003421830178490235450 ),
 .UNSPECIFIED. ) ;
#4703 = EDGE_CURVE ( 'NONE', #17954, #21094, #3610, .T. ) ;
#4704 = VECTOR ( 'NONE', #23050, 1000.000000000000000 ) ;
#4705 = CARTESIAN_POINT ( 'NONE',  ( 26.80246859415415273, 7.028748154183637631, -1.499999999999999556 ) ) ;
#4706 = DIRECTION ( 'NONE',  ( 0.000000000000000000, 0.000000000000000000, -1.000000000000000000 ) ) ;
#4707 = ORIENTED_EDGE ( 'NONE', *, *, #7500, .F. ) ;
#4708 = CARTESIAN_POINT ( 'NONE',  ( 15.44332723074500180, -7.163653983975262207, 6.143977687428009204 ) ) ;
#4709 = CARTESIAN_POINT ( 'NONE',  ( 39.83602371822922095, -11.57901747687539640, -19.50000000000000355 ) ) ;
#4710 = CARTESIAN_POINT ( 'NONE',  ( -2.081668171172168513E-14, 80.00000000000000000, 37.49999999999999289 ) ) ;
#4711 = VERTEX_POINT ( 'NONE', #14839 ) ;
#4712 = CARTESIAN_POINT ( 'NONE',  ( -23.62400240902268322, -9.724154461249517212, 49.47829057475703252 ) ) ;
#4713 = CARTESIAN_POINT ( 'NONE',  ( -15.10044507415838488, -7.916284227987608446, 20.33971507717571114 ) ) ;
#4714 = CARTESIAN_POINT ( 'NONE',  ( 6.631244434206235105, 6.812559277181991391, 1.500000000000001332 ) ) ;
#4715 = CARTESIAN_POINT ( 'NONE',  ( 4.892923698309762592, 16.30563068515024838, 6.143977687428008316 ) ) ;
#4716 = CARTESIAN_POINT ( 'NONE',  ( -15.10419704716067102, -17.26937953831884442, -1.500000000000000000 ) ) ;
#4717 = ORIENTED_EDGE ( 'NONE', *, *, #21348, .F. ) ;
#4718 = DIRECTION ( 'NONE',  ( -1.000000000000000000, 0.000000000000000000, 0.000000000000000000 ) ) ;
#4719 = CARTESIAN_POINT ( 'NONE',  ( 37.16608720827707657, -65.00000000000000000, 97.07879600563551037 ) ) ;
#4720 = CARTESIAN_POINT ( 'NONE',  ( 24.51012911669599958, 28.40691445806841386, 37.50000000005638157 ) ) ;
#4721 = CARTESIAN_POINT ( 'NONE',  ( -4.163336342344337027E-14, 1.387778780781445676E-14, 62.49999999999999289 ) ) ;
#4722 = ORIENTED_EDGE ( 'NONE', *, *, #21635, .T. ) ;
#4723 = ORIENTED_EDGE ( 'NONE', *, *, #2706, .F. ) ;
#4724 = PLANE ( 'NONE',  #22159 ) ;
#4725 = CARTESIAN_POINT ( 'NONE',  ( 0.000000000000000000, 0.000000000000000000, 1.500000000000001332 ) ) ;
#4726 = ORIENTED_EDGE ( 'NONE', *, *, #20656, .T. ) ;
#4727 = CIRCLE ( 'NONE', #23636, 32.50000000000000000 ) ;
#4728 = ORIENTED_EDGE ( 'NONE', *, *, #9371, .F. ) ;
#4729 = CARTESIAN_POINT ( 'NONE',  ( 7.730328572437743517, -4.608906612435629491, 1.500000000000001332 ) ) ;
#4730 = ORIENTED_EDGE ( 'NONE', *, *, #1597, .T. ) ;
#4731 = ORIENTED_EDGE ( 'NONE', *, *, #8208, .F. ) ;
#4732 = CARTESIAN_POINT ( 'NONE',  ( 0.5496282100021194772, -17.03044801512709938, 20.32842677360128292 ) ) ;
#4733 = CARTESIAN_POINT ( 'NONE',  ( -7.919226493207299100, -15.11997014267743822, 5.951255046771932733 ) ) ;
#4734 = CARTESIAN_POINT ( 'NONE',  ( 4.892923698324559645, 16.30563068514543446, 18.83976166372255534 ) ) ;
#4735 = CARTESIAN_POINT ( 'NONE',  ( 1.303806812501130619, -19.97511938206333681, 19.69140814234746273 ) ) ;
#4736 = ORIENTED_EDGE ( 'NONE', *, *, #8425, .F. ) ;
#4737 = CARTESIAN_POINT ( 'NONE',  ( 18.70859934877966424, -7.070433808158458788, 6.919864475265772086 ) ) ;
#4738 = DIRECTION ( 'NONE',  ( -0.000000000000000000, -0.000000000000000000, 1.000000000000000000 ) ) ;
#4739 = CARTESIAN_POINT ( 'NONE',  ( 11.98626544954000117, 12.14249340222027129, 18.50655187082627862 ) ) ;
#4740 = DIRECTION ( 'NONE',  ( 0.000000000000000000, -0.8660254037844383745, 0.5000000000000006661 ) ) ;
#4741 = ORIENTED_EDGE ( 'NONE', *, *, #25781, .T. ) ;
#4742 = CARTESIAN_POINT ( 'NONE',  ( 69.99999999999998579, 70.00000000000000000, -92.50000000000000000 ) ) ;
#4743 = CARTESIAN_POINT ( 'NONE',  ( -17.66624025659152863, -9.413543259203214220, 6.131018562779544823 ) ) ;
#4744 = CARTESIAN_POINT ( 'NONE',  ( 9.349584168494304848, 12.69858007495367680, 1.500000000000001332 ) ) ;
#4745 = AXIS2_PLACEMENT_3D ( 'NONE', #14191, #2345, #10 ) ;
#4746 = FACE_OUTER_BOUND ( 'NONE', #22612, .T. ) ;
#4747 = DIRECTION ( 'NONE',  ( 1.000000000000000000, 0.000000000000000000, 0.000000000000000000 ) ) ;
#4748 = EDGE_CURVE ( 'NONE', #19059, #20079, #13400, .T. ) ;
#4749 = CARTESIAN_POINT ( 'NONE',  ( 2.538591345309722414, 42.43983719188426562, 28.84490890740515567 ) ) ;
#4750 = CARTESIAN_POINT ( 'NONE',  ( 1.073881485057758711, -0.9711784013061475207, -1.500000000000000000 ) ) ;
#4751 = ORIENTED_EDGE ( 'NONE', *, *, #24059, .T. ) ;
#4752 = ORIENTED_EDGE ( 'NONE', *, *, #5216, .F. ) ;
#4753 = CARTESIAN_POINT ( 'NONE',  ( 2.810445847081857629, 9.056208293496320394, 1.500000000000001332 ) ) ;
#4754 = CARTESIAN_POINT ( 'NONE',  ( -12.56641067637617759, -40.32935944494947478, -1.500000000000000000 ) ) ;
#4755 = CARTESIAN_POINT ( 'NONE',  ( -12.74366836927934976, 11.28516576207253053, 6.974106381145714018 ) ) ;
#4756 = LINE ( 'NONE', #2586, #16068 ) ;
#4757 = ORIENTED_EDGE ( 'NONE', *, *, #14546, .T. ) ;
#4758 = CARTESIAN_POINT ( 'NONE',  ( 17.97060409579513163, -8.818932628521073624, 18.90679857307105749 ) ) ;
#4759 = CARTESIAN_POINT ( 'NONE',  ( 6.275630943545792206, 19.00876817605120195, 6.641371103590088865 ) ) ;
#4760 = ORIENTED_EDGE ( 'NONE', *, *, #8795, .T. ) ;
#4761 = CARTESIAN_POINT ( 'NONE',  ( 4.575061044035268587, 16.40537387836874927, 20.19668224736330941 ) ) ;
#4762 = CARTESIAN_POINT ( 'NONE',  ( -32.93066663369632607, -23.11087908566834770, -3.166603007242238643 ) ) ;
#4763 = DIRECTION ( 'NONE',  ( 0.000000000000000000, 0.000000000000000000, -1.000000000000000000 ) ) ;
#4764 = CARTESIAN_POINT ( 'NONE',  ( -27.01611617209707816, 30.66277435038324128, 34.52684288084092401 ) ) ;
#4765 = ORIENTED_EDGE ( 'NONE', *, *, #23833, .T. ) ;
#4766 = DIRECTION ( 'NONE',  ( -0.000000000000000000, -0.000000000000000000, 1.000000000000000000 ) ) ;
#4767 = AXIS2_PLACEMENT_3D ( 'NONE', #22328, #15298, #3464 ) ;
#4768 = EDGE_CURVE ( 'NONE', #4932, #21725, #29265, .T. ) ;
#4769 = DIRECTION ( 'NONE',  ( -0.000000000000000000, 1.132880637372608986E-16, -1.000000000000000000 ) ) ;
#4770 = AXIS2_PLACEMENT_3D ( 'NONE', #11070, #11217, #25258 ) ;
#4771 = DIRECTION ( 'NONE',  ( 0.000000000000000000, 0.000000000000000000, 1.000000000000000000 ) ) ;
#4772 = VERTEX_POINT ( 'NONE', #22468 ) ;
#4773 = CARTESIAN_POINT ( 'NONE',  ( -18.11003155545034460, -8.529482236167142517, 7.652108011868850035 ) ) ;
#4774 = EDGE_CURVE ( 'NONE', #26376, #14162, #5344, .T. ) ;
#4775 = CARTESIAN_POINT ( 'NONE',  ( -3.196529495465446402, -8.413215745754985875, 1.500000000000001332 ) ) ;
#4776 = CARTESIAN_POINT ( 'NONE',  ( -64.99999999999998579, 36.86186943028246787, 12.49999999999999112 ) ) ;
#4777 = ADVANCED_FACE ( 'NONE', ( #1116 ), #10784, .F. ) ;
#4778 = LINE ( 'NONE', #259, #26740 ) ;
#4779 = LINE ( 'NONE', #3067, #23204 ) ;
#4780 = CYLINDRICAL_SURFACE ( 'NONE', #7047, 3.000000000000002665 ) ;
#4781 = CARTESIAN_POINT ( 'NONE',  ( 34.23529990058388250, -20.39752770391714876, 17.87601422035457333 ) ) ;
#4782 = LINE ( 'NONE', #6525, #15356 ) ;
#4783 = ORIENTED_EDGE ( 'NONE', *, *, #20862, .T. ) ;
#4784 = ADVANCED_FACE ( 'NONE', ( #24353 ), #3000, .F. ) ;
#4785 = CARTESIAN_POINT ( 'NONE',  ( 11.17648341053133976, -16.60731568869665153, 20.34789198813115263 ) ) ;
#4786 = DIRECTION ( 'NONE',  ( 0.000000000000000000, -1.132880637372608986E-16, 1.000000000000000000 ) ) ;
#4787 = EDGE_CURVE ( 'NONE', #1099, #23147, #22773, .T. ) ;
#4788 = ORIENTED_EDGE ( 'NONE', *, *, #6550, .T. ) ;
#4789 = ORIENTED_EDGE ( 'NONE', *, *, #24819, .F. ) ;
#4791 = EDGE_CURVE ( 'NONE', #7470, #18940, #19832, .T. ) ;
#4790 = CIRCLE ( 'NONE', #8782, 9.482273699623480212 ) ;
#4792 = CARTESIAN_POINT ( 'NONE',  ( 5.291489565152559749, 19.28730510418394672, 18.34798005863226678 ) ) ;
#4793 = DIRECTION ( 'NONE',  ( 0.000000000000000000, -1.132880637372608986E-16, 1.000000000000000000 ) ) ;
#4794 = ORIENTED_EDGE ( 'NONE', *, *, #11872, .T. ) ;
#4795 = CIRCLE ( 'NONE', #17249, 2.061368542273053883 ) ;
#4796 = CARTESIAN_POINT ( 'NONE',  ( 12.51082390549570889, 11.56795297236522480, 20.32842677360128292 ) ) ;
#4797 = CARTESIAN_POINT ( 'NONE',  ( 15.90320373664000009, -6.152843468454362252, 18.37415474056476938 ) ) ;
#4798 = CARTESIAN_POINT ( 'NONE',  ( 19.60578376704636838, 4.040313317649107283, 19.89182036555910571 ) ) ;
#4799 = AXIS2_PLACEMENT_3D ( 'NONE', #12088, #24391, #14879 ) ;
#4800 = CARTESIAN_POINT ( 'NONE',  ( -25.18466322232232457, 6.657711795334223304, 48.95036236631857207 ) ) ;
#4801 = ORIENTED_EDGE ( 'NONE', *, *, #17400, .T. ) ;
#4802 = CARTESIAN_POINT ( 'NONE',  ( 14.44122519041005859, -13.83658248990206729, 1.500000000000001332 ) ) ;
#4803 = AXIS2_PLACEMENT_3D ( 'NONE', #7056, #16564, #19063 ) ;
#4804 = EDGE_CURVE ( 'NONE', #20273, #16284, #11321, .T. ) ;
#4805 = ORIENTED_EDGE ( 'NONE', *, *, #3767, .F. ) ;
#4806 = EDGE_CURVE ( 'NONE', #17339, #20389, #18315, .T. ) ;
#4807 = CIRCLE ( 'NONE', #6391, 9.084132297865673777 ) ;
#4808 = EDGE_CURVE ( 'NONE', #14021, #12560, #15981, .T. ) ;
#4809 = EDGE_LOOP ( 'NONE', ( #19388, #2819, #16274, #20379 ) ) ;
#4810 = AXIS2_PLACEMENT_3D ( 'NONE', #5511, #20009, #3023 ) ;
#4811 = VECTOR ( 'NONE', #14610, 1000.000000000000000 ) ;
#4812 = EDGE_CURVE ( 'NONE', #19313, #19602, #3323, .T. ) ;
#4813 = FACE_OUTER_BOUND ( 'NONE', #2331, .T. ) ;
#4814 = CARTESIAN_POINT ( 'NONE',  ( 0.1624814967139596167, -17.02900520012434882, 18.54473042795395443 ) ) ;
#4815 = AXIS2_PLACEMENT_3D ( 'NONE', #4869, #14385, #23892 ) ;
#4816 = CARTESIAN_POINT ( 'NONE',  ( 0.7902931953360854411, -20.00234323981187856, 7.559636331181775581 ) ) ;
#4817 = CARTESIAN_POINT ( 'NONE',  ( -40.00000000000002842, 80.00000000000001421, 27.49999999999983658 ) ) ;
#4818 = DIRECTION ( 'NONE',  ( -0.000000000000000000, 0.000000000000000000, 1.000000000000000000 ) ) ;
#4819 = VERTEX_POINT ( 'NONE', #23227 ) ;
#4820 = ADVANCED_FACE ( 'NONE', ( #6098 ), #20354, .T. ) ;
#4821 = CARTESIAN_POINT ( 'NONE',  ( -19.85654738780300832, 2.535877853918452995, 18.34777357837152323 ) ) ;
#4822 = DIRECTION ( 'NONE',  ( -0.000000000000000000, -0.000000000000000000, 1.000000000000000000 ) ) ;
#4823 = VECTOR ( 'NONE', #18717, 1000.000000000000000 ) ;
#4824 = DIRECTION ( 'NONE',  ( -0.000000000000000000, -0.000000000000000000, 1.000000000000000000 ) ) ;
#4825 = ORIENTED_EDGE ( 'NONE', *, *, #7691, .T. ) ;
#4826 = ORIENTED_EDGE ( 'NONE', *, *, #5765, .F. ) ;
#4827 = CARTESIAN_POINT ( 'NONE',  ( 39.52380524535330153, 7.028748154198969367, -11.49999999999999645 ) ) ;
#4828 = CARTESIAN_POINT ( 'NONE',  ( 23.28555253867649810, -23.03920922976760721, -16.50001200000000168 ) ) ;
#4829 = DIRECTION ( 'NONE',  ( 0.000000000000000000, 0.000000000000000000, 1.000000000000000000 ) ) ;
#4830 = CARTESIAN_POINT ( 'NONE',  ( -15.16517293421789070, -7.781889191988407894, 7.652108011868850923 ) ) ;
#4831 = FACE_OUTER_BOUND ( 'NONE', #2557, .T. ) ;
#4832 = VECTOR ( 'NONE', #17699, 1000.000000000000000 ) ;
#4833 = CARTESIAN_POINT ( 'NONE',  ( -16.56775953753748354, -35.09133156286775090, 27.50000000000001066 ) ) ;
#4834 = DIRECTION ( 'NONE',  ( 1.000000000000000000, 0.000000000000000000, 0.000000000000000000 ) ) ;
#4835 = EDGE_CURVE ( 'NONE', #27607, #115, #14177, .T. ) ;
#4836 = ORIENTED_EDGE ( 'NONE', *, *, #12611, .T. ) ;
#4837 = EDGE_CURVE ( 'NONE', #9540, #115, #19279, .T. ) ;
#4838 = ADVANCED_FACE ( 'NONE', ( #23683 ), #6859, .F. ) ;
#4839 = AXIS2_PLACEMENT_3D ( 'NONE', #17881, #17705, #8057 ) ;
#4840 = CARTESIAN_POINT ( 'NONE',  ( -28.12430571491142572, -24.65851106883863508, 34.49999999999999289 ) ) ;
#4841 = CARTESIAN_POINT ( 'NONE',  ( -17.59500444164589794, -9.508866521682287853, 19.61564845152807735 ) ) ;
#4842 = CARTESIAN_POINT ( 'NONE',  ( -50.00000000000000000, -50.00000000000000000, -87.50000000000000000 ) ) ;
#4843 = VERTEX_POINT ( 'NONE', #11855 ) ;
#4844 = CARTESIAN_POINT ( 'NONE',  ( 15.48724201788533428, 12.68311944884417919, 6.211014596808754007 ) ) ;
#4845 = ORIENTED_EDGE ( 'NONE', *, *, #25979, .F. ) ;
#4846 = VECTOR ( 'NONE', #4013, 1000.000000000000000 ) ;
#4847 = DIRECTION ( 'NONE',  ( -1.000000000000000000, 0.000000000000000000, 0.000000000000000000 ) ) ;
#4848 = UNCERTAINTY_MEASURE_WITH_UNIT (LENGTH_MEASURE( 1.000000000000000082E-05 ), #21403, 'distance_accuracy_value', 'NONE');
#4849 = CIRCLE ( 'NONE', #26266, 5.000000000000004441 ) ;
#4850 = CARTESIAN_POINT ( 'NONE',  ( -10.31606103249976059, 42.64332891061493314, -16.49999999999999645 ) ) ;
#4851 = VECTOR ( 'NONE', #26357, 1000.000000000000227 ) ;
#4852 = ORIENTED_EDGE ( 'NONE', *, *, #6683, .F. ) ;
#4853 = CARTESIAN_POINT ( 'NONE',  ( 34.25977182215996919, -12.14538519402363903, 27.50000000000000000 ) ) ;
#4854 = AXIS2_PLACEMENT_3D ( 'NONE', #29179, #19979, #7517 ) ;
#4855 = CARTESIAN_POINT ( 'NONE',  ( 0.000000000000000000, 42.50000000000000000, 24.50000000000000000 ) ) ;
#4856 = DIRECTION ( 'NONE',  ( -0.000000000000000000, -0.000000000000000000, 1.000000000000000000 ) ) ;
#4857 = CARTESIAN_POINT ( 'NONE',  ( 0.8038475772931101826, -5.196152422707025487, -9.000000000000000000 ) ) ;
#4858 = CIRCLE ( 'NONE', #19287, 0.7499999999999997780 ) ;
#4859 = VECTOR ( 'NONE', #2278, 1000.000000000000000 ) ;
#4860 = CARTESIAN_POINT ( 'NONE',  ( -30.26724724044810699, -27.72993536917633151, -6.500000000000001776 ) ) ;
#4861 = CARTESIAN_POINT ( 'NONE',  ( -29.61203839202723032, 15.40012917324033204, 41.62281023987520001 ) ) ;
#4862 = VERTEX_POINT ( 'NONE', #21824 ) ;
#4863 = CARTESIAN_POINT ( 'NONE',  ( -8.549050687778191104, -4.102102735472431760, 1.500000000000001332 ) ) ;
#4864 = VECTOR ( 'NONE', #24722, 1000.000000000000000 ) ;
#4865 = CARTESIAN_POINT ( 'NONE',  ( 4.336808689942017736E-16, 42.50000000000000000, -1.500000000000000000 ) ) ;
#4866 = DIRECTION ( 'NONE',  ( -0.000000000000000000, -0.000000000000000000, 1.000000000000000000 ) ) ;
#4867 = EDGE_LOOP ( 'NONE', ( #30617, #2776, #28876, #19505 ) ) ;
#4868 = LINE ( 'NONE', #10593, #25520 ) ;
#4869 = CARTESIAN_POINT ( 'NONE',  ( 0.1262659238204208167, 8.999114229549594057, -1.500000000000000888 ) ) ;
#4870 = VECTOR ( 'NONE', #29883, 1000.000000000000000 ) ;
#4871 = CARTESIAN_POINT ( 'NONE',  ( -22.58267429318970443, -26.57182937991348481, 24.50000000000000000 ) ) ;
#4872 = CARTESIAN_POINT ( 'NONE',  ( 4.644508076310276401, 16.38413139300089227, 7.453286057244488561 ) ) ;
#4873 = AXIS2_PLACEMENT_3D ( 'NONE', #30449, #16414, #28120 ) ;
#4874 = CARTESIAN_POINT ( 'NONE',  ( 39.83602371822922095, -11.57901747687539640, -19.50000000000000355 ) ) ;
#4875 = AXIS2_PLACEMENT_3D ( 'NONE', #10231, #7915, #18189 ) ;
#4876 = EDGE_LOOP ( 'NONE', ( #30060, #10543, #29266, #29368 ) ) ;
#4877 = DIRECTION ( 'NONE',  ( -1.000000000000000000, 0.000000000000000000, 0.000000000000000000 ) ) ;
#4878 = CARTESIAN_POINT ( 'NONE',  ( 30.58308285076613586, 26.38567509859110061, 34.58766046687880902 ) ) ;
#4879 = CARTESIAN_POINT ( 'NONE',  ( -6.933969404122152902, 18.75953273845654579, 6.788986777570698905 ) ) ;
#4880 = ORIENTED_EDGE ( 'NONE', *, *, #19250, .F. ) ;
#4881 = DIRECTION ( 'NONE',  ( -0.000000000000000000, -0.000000000000000000, 1.000000000000000000 ) ) ;
#4883 = VERTEX_POINT ( 'NONE', #4523 ) ;
#4882 = VECTOR ( 'NONE', #29455, 1000.000000000000000 ) ;
#4884 = CARTESIAN_POINT ( 'NONE',  ( -37.98493438988128901, 11.12428508575241004, -1.500000000000000000 ) ) ;
#4885 = DIRECTION ( 'NONE',  ( -1.000000000000000000, 0.000000000000000000, 0.000000000000000000 ) ) ;
#4886 = AXIS2_PLACEMENT_3D ( 'NONE', #26893, #8326, #17842 ) ;
#4887 = VERTEX_POINT ( 'NONE', #23995 ) ;
#4888 = VERTEX_POINT ( 'NONE', #12012 ) ;
#4889 = FACE_OUTER_BOUND ( 'NONE', #13109, .T. ) ;
#4890 = ORIENTED_EDGE ( 'NONE', *, *, #3454, .T. ) ;
#4891 = ORIENTED_EDGE ( 'NONE', *, *, #21373, .F. ) ;
#4892 = ORIENTED_EDGE ( 'NONE', *, *, #14529, .F. ) ;
#4893 = CARTESIAN_POINT ( 'NONE',  ( -0.1864951924744789880, -20.01724188655222747, 18.49267272388512140 ) ) ;
#4894 = CARTESIAN_POINT ( 'NONE',  ( -9.972083266784114386, -17.35726207598482063, 5.872146474157316831 ) ) ;
#4895 = AXIS2_PLACEMENT_3D ( 'NONE', #25187, #15525, #27081 ) ;
#4896 = CARTESIAN_POINT ( 'NONE',  ( -34.50378612593421224, 19.82132163181573148, 17.77334831411353733 ) ) ;
#4897 = CARTESIAN_POINT ( 'NONE',  ( 1.568770080425526237, -16.99791492429841711, 19.97651184436794125 ) ) ;
#4898 = CIRCLE ( 'NONE', #9376, 20.00000000000000000 ) ;
#4899 = ORIENTED_EDGE ( 'NONE', *, *, #24785, .F. ) ;
#4900 = CARTESIAN_POINT ( 'NONE',  ( 11.11118388262826251, -16.62953976291647962, 5.652196082369964181 ) ) ;
#4901 = DIRECTION ( 'NONE',  ( 0.000000000000000000, -0.000000000000000000, -1.000000000000000000 ) ) ;
#4902 = CARTESIAN_POINT ( 'NONE',  ( 11.81884104268966773, 12.31686436340674184, 19.97651184436794125 ) ) ;
#4903 = CARTESIAN_POINT ( 'NONE',  ( 32.28307784207223108, 8.475829241206289666, 37.38016955275583086 ) ) ;
#4904 = ORIENTED_EDGE ( 'NONE', *, *, #8427, .F. ) ;
#4905 = AXIS2_PLACEMENT_3D ( 'NONE', #19903, #1181, #29259 ) ;
#4906 = CARTESIAN_POINT ( 'NONE',  ( 26.80246859415415273, 7.028748154183637631, -1.499999999999999556 ) ) ;
#4907 = CARTESIAN_POINT ( 'NONE',  ( -17.69908921317806261, -9.351398086983019553, 6.041646659195333058 ) ) ;
#4908 = DIRECTION ( 'NONE',  ( -0.000000000000000000, -0.000000000000000000, -1.000000000000000000 ) ) ;
#4909 = DIRECTION ( 'NONE',  ( 0.8932538319083086487, 0.4495526574063634095, -0.000000000000000000 ) ) ;
#4910 = CARTESIAN_POINT ( 'NONE',  ( -23.59263552078001425, 12.85968412197262545, 43.88772444904758885 ) ) ;
#4911 = CARTESIAN_POINT ( 'NONE',  ( -4.163336342344337027E-14, 1.387778780781445676E-14, 37.50000000000000000 ) ) ;
#4912 = CARTESIAN_POINT ( 'NONE',  ( 5.105024945673418912, -42.22604126506271882, -1.500000000000000000 ) ) ;
#4913 = ORIENTED_EDGE ( 'NONE', *, *, #16059, .F. ) ;
#4914 = VERTEX_POINT ( 'NONE', #2329 ) ;
#4915 = CARTESIAN_POINT ( 'NONE',  ( -3.469446951953614189E-15, -30.50000000000000711, 24.50000000000000000 ) ) ;
#4916 = CARTESIAN_POINT ( 'NONE',  ( -23.96732207939035675, 33.98584080153585774, -1.500000000000000000 ) ) ;
#4917 = CARTESIAN_POINT ( 'NONE',  ( -14.70379955820389561, 13.58362208154139772, 6.864725433338323413 ) ) ;
#4918 = CARTESIAN_POINT ( 'NONE',  ( 7.500000000000000000, 8.082668874372532992E-16, 6.600000000000001421 ) ) ;
#4919 = ORIENTED_EDGE ( 'NONE', *, *, #332, .F. ) ;
#4920 = CONTEXT_DEPENDENT_SHAPE_REPRESENTATION ( #815, #7178 ) ;
#4921 = VECTOR ( 'NONE', #29031, 1000.000000000000000 ) ;
#4922 = DIRECTION ( 'NONE',  ( 0.000000000000000000, 0.000000000000000000, 1.000000000000000000 ) ) ;
#4923 = CIRCLE ( 'NONE', #9886, 50.00000000000000000 ) ;
#4924 = CARTESIAN_POINT ( 'NONE',  ( 6.060672894209297112, 19.07852886212369725, 6.018569869498933578 ) ) ;
#4925 = EDGE_LOOP ( 'NONE', ( #28982, #987, #26981, #872 ) ) ;
#4926 = CARTESIAN_POINT ( 'NONE',  ( 4.971436688744666377, 16.28007576866361816, 19.66989035740801839 ) ) ;
#4927 = FACE_OUTER_BOUND ( 'NONE', #18242, .T. ) ;
#4928 = EDGE_CURVE ( 'NONE', #25203, #10854, #5137, .T. ) ;
#4929 = AXIS2_PLACEMENT_3D ( 'NONE', #6643, #16160, #4297 ) ;
#4930 = DIRECTION ( 'NONE',  ( 1.000000000000000000, 0.000000000000000000, 0.000000000000000000 ) ) ;
#4931 = CARTESIAN_POINT ( 'NONE',  ( -32.22095362587521095, 24.09752088550972005, 30.66525214441444902 ) ) ;
#4932 = VERTEX_POINT ( 'NONE', #26043 ) ;
#4933 = DIRECTION ( 'NONE',  ( -0.000000000000000000, -0.000000000000000000, 1.000000000000000000 ) ) ;
#4934 = B_SPLINE_CURVE_WITH_KNOTS ( 'NONE', 3,
 ( #23015, #20387, #1363, #6037, #10878, #1820, #3855, #4008, #20678, #15546, #13533, #20222, #1213, #11343, #1520, #25531, #8844, #29911, #20532, #25061 ),
 .UNSPECIFIED., .F., .F.,
 ( 4, 2, 2, 2, 2, 2, 2, 2, 2, 4 ),
 ( 0.000000000000000000, 0.06250000000000006939, 0.1250000000000001388, 0.1875000000000002220, 0.2187499999999995282, 0.2499999999999988065, 0.3124999999999990563, 0.3749999999999992784, 0.4374999999999995559, 0.4999999999999997224 ),
 .UNSPECIFIED. ) ;
#4935 = CARTESIAN_POINT ( 'NONE',  ( 33.51212652704789008, 9.877957833750135919, 35.81989857765422869 ) ) ;
#4936 = EDGE_CURVE ( 'NONE', #27180, #9077, #13812, .T. ) ;
#4937 = DIRECTION ( 'NONE',  ( 1.000000000000000000, 0.000000000000000000, 0.000000000000000000 ) ) ;
#4938 = ORIENTED_EDGE ( 'NONE', *, *, #29023, .F. ) ;
#4939 =( BOUNDED_CURVE ( )  B_SPLINE_CURVE ( 3, ( #26353, #26038, #4670, #4360 ),
 .UNSPECIFIED., .F., .T. ) 
 B_SPLINE_CURVE_WITH_KNOTS ( ( 4, 4 ),
 ( 0.8137667884748612801, 2.327825865114931947 ),
 .UNSPECIFIED. ) 
 CURVE ( )  GEOMETRIC_REPRESENTATION_ITEM ( )  RATIONAL_B_SPLINE_CURVE ( ( 1.000000000000000000, 0.8179194830933627092, 0.8179194830933627092, 1.000000000000000000 ) ) 
 REPRESENTATION_ITEM ( '' )  );
#4940 = CARTESIAN_POINT ( 'NONE',  ( -18.28579658156514043, -8.145820804509362745, 5.796888747622817029 ) ) ;
#4941 = DIRECTION ( 'NONE',  ( -0.000000000000000000, 0.000000000000000000, 1.000000000000000000 ) ) ;
#4942 = DIRECTION ( 'NONE',  ( -0.000000000000000000, -0.000000000000000000, -1.000000000000000000 ) ) ;
#4943 = PRODUCT ( 'Housing End Cover Cap', 'Housing End Cover Cap', '', ( #393 ) ) ;
#4944 = DIRECTION ( 'NONE',  ( 0.000000000000000000, 0.000000000000000000, 1.000000000000000000 ) ) ;
#4945 = CARTESIAN_POINT ( 'NONE',  ( 50.00000000000000000, 6.123233995736766085E-15, 12.49999999999998401 ) ) ;
#4946 = DIRECTION ( 'NONE',  ( -0.9547931052914335748, 0.2972711322815276835, 0.000000000000000000 ) ) ;
#4947 = CARTESIAN_POINT ( 'NONE',  ( 37.94146307560947662, -9.835134691610786462, 13.69354701980937961 ) ) ;
#4948 = CARTESIAN_POINT ( 'NONE',  ( 24.35970437652574105, 13.37404834226503958, 47.21042702067963859 ) ) ;
#4949 = VERTEX_POINT ( 'NONE', #14648 ) ;
#4950 = CARTESIAN_POINT ( 'NONE',  ( -7.667077102831937552, 13.77986170986486592, 1.500000000000001332 ) ) ;
#4951 = VECTOR ( 'NONE', #10605, 1000.000000000000000 ) ;
#4952 = CARTESIAN_POINT ( 'NONE',  ( 4.677126025380971441, 39.24912351428226742, 34.80090346875809360 ) ) ;
#4953 = ORIENTED_EDGE ( 'NONE', *, *, #21611, .T. ) ;
#4954 = VERTEX_POINT ( 'NONE', #21355 ) ;
#4955 = EDGE_CURVE ( 'NONE', #4819, #2473, #21661, .T. ) ;
#4956 = CARTESIAN_POINT ( 'NONE',  ( 6.543385983536345485, 6.301234758012618009, 13.22130136205108819 ) ) ;
#4957 = CARTESIAN_POINT ( 'NONE',  ( -14.99954637771879540, 47.69710272843848742, -54.00831070145920165 ) ) ;
#4958 = EDGE_LOOP ( 'NONE', ( #3675, #4537, #8204, #25298 ) ) ;
#4959 = EDGE_CURVE ( 'NONE', #7694, #20319, #145, .T. ) ;
#4960 = DIRECTION ( 'NONE',  ( -0.000000000000000000, -0.000000000000000000, -1.000000000000000000 ) ) ;
#4961 = FACE_BOUND ( 'NONE', #30357, .T. ) ;
#4962 = ORIENTED_EDGE ( 'NONE', *, *, #30551, .F. ) ;
#4963 = EDGE_CURVE ( 'NONE', #21613, #27751, #9203, .T. ) ;
#4964 = CARTESIAN_POINT ( 'NONE',  ( 16.17271416092066261, -5.480318835022395696, 19.69140814234746273 ) ) ;
#4965 = CARTESIAN_POINT ( 'NONE',  ( 16.74250592927944936, 3.198927888044590162, 18.34798005862662507 ) ) ;
#4966 = CARTESIAN_POINT ( 'NONE',  ( -3.683253992019773992, 8.303920738747248009, 13.22130136205108997 ) ) ;
#4967 = ORIENTED_EDGE ( 'NONE', *, *, #18387, .F. ) ;
#4968 = LINE ( 'NONE', #2478, #10342 ) ;
#4969 = ORIENTED_EDGE ( 'NONE', *, *, #8636, .F. ) ;
#4970 = AXIS2_PLACEMENT_3D ( 'NONE', #6761, #9422, #25648 ) ;
#4971 = ADVANCED_FACE ( 'NONE', ( #19334 ), #24151, .F. ) ;
#4972 = VERTEX_POINT ( 'NONE', #28541 ) ;
#4973 = EDGE_CURVE ( 'NONE', #30466, #23022, #14032, .T. ) ;
#4974 = LINE ( 'NONE', #19320, #10114 ) ;
#4975 = CARTESIAN_POINT ( 'NONE',  ( -12.74837729798237440, 11.28012212083751642, 19.00652017443069752 ) ) ;
#4976 = CARTESIAN_POINT ( 'NONE',  ( -15.57266529552203416, 38.96488032230103471, 1.500000000000000000 ) ) ;
#4977 = CARTESIAN_POINT ( 'NONE',  ( 16.52525247487311333, -14.36006998371588317, -1.500000000000000000 ) ) ;
#4978 = CARTESIAN_POINT ( 'NONE',  ( 1.047421501641249364, -17.02264912680065478, 18.34938820207545263 ) ) ;
#4979 = CARTESIAN_POINT ( 'NONE',  ( 16.85411910731514240, 2.412525337365567513, 18.71435384576123440 ) ) ;
#4980 = VERTEX_POINT ( 'NONE', #28856 ) ;
#4981 = CARTESIAN_POINT ( 'NONE',  ( 6.900000000000000355, -7.794228634059942706, 4.500000000000005329 ) ) ;
#4982 = CARTESIAN_POINT ( 'NONE',  ( 15.78348099220817957, -6.430800111306883338, 5.653912893140659257 ) ) ;
#4983 = CARTESIAN_POINT ( 'NONE',  ( -15.35487439336962012, 12.84287527963942921, 7.652108011868850035 ) ) ;
#4984 = CARTESIAN_POINT ( 'NONE',  ( 1.000000000000008438, 15.73749217771910125, -0.6213203435596476032 ) ) ;
#4985 = ORIENTED_EDGE ( 'NONE', *, *, #15762, .T. ) ;
#4986 = ORIENTED_EDGE ( 'NONE', *, *, #13221, .F. ) ;
#4987 = CARTESIAN_POINT ( 'NONE',  ( -4.100931858250860707, -19.90478481566557534, -1.500000000000000000 ) ) ;
#4988 = EDGE_CURVE ( 'NONE', #21772, #15921, #19174, .T. ) ;
#4989 = PLANE ( 'NONE',  #9636 ) ;
#4990 = ADVANCED_FACE ( 'NONE', ( #7333 ), #298, .F. ) ;
#4991 = CARTESIAN_POINT ( 'NONE',  ( -39.87350638640939593, 4.706224724266459880, -11.49999999999999645 ) ) ;
#4992 = CARTESIAN_POINT ( 'NONE',  ( -5.128149923613388950, 16.24357618101654666, 18.44501272782439827 ) ) ;
#4993 = CARTESIAN_POINT ( 'NONE',  ( -15.22000698767478788, -7.667275872209097898, 5.651492010659115550 ) ) ;
#4994 = AXIS2_PLACEMENT_3D ( 'NONE', #5814, #27033, #22484 ) ;
#4995 = CARTESIAN_POINT ( 'NONE',  ( -9.834155381565185650, -38.09377060189168418, 27.50000000000000355 ) ) ;
#4996 = LINE ( 'NONE', #14656, #29364 ) ;
#4997 = ADVANCED_FACE ( 'NONE', ( #7172 ), #14339, .F. ) ;
#4998 = CARTESIAN_POINT ( 'NONE',  ( -10.05674029770914579, -37.94258163987278465, 34.49999999999998579 ) ) ;
#4999 = DIRECTION ( 'NONE',  ( -1.000000000000000000, 0.000000000000000000, 0.000000000000000000 ) ) ;
#5000 = DIRECTION ( 'NONE',  ( 1.000000000000000000, 0.000000000000000000, 0.000000000000000000 ) ) ;
#5001 = ADVANCED_FACE ( 'NONE', ( #28696 ), #30709, .F. ) ;
#5002 = VERTEX_POINT ( 'NONE', #2764 ) ;
#5003 = CARTESIAN_POINT ( 'NONE',  ( 12.65169814564037054, 11.40562544919841415, 7.557577766377196582 ) ) ;
#5004 = ORIENTED_EDGE ( 'NONE', *, *, #3097, .T. ) ;
#5005 = ADVANCED_FACE ( 'NONE', ( #5101 ), #28810, .T. ) ;
#5006 = DIRECTION ( 'NONE',  ( -1.000000000000000000, 0.000000000000000000, 0.000000000000000000 ) ) ;
#5007 = CARTESIAN_POINT ( 'NONE',  ( 16.56110944985486455, 4.167213836826286766, 19.61324152429826739 ) ) ;
#5008 = CYLINDRICAL_SURFACE ( 'NONE', #12575, 2.898871837527151829 ) ;
#5009 = VERTEX_POINT ( 'NONE', #27085 ) ;
#5010 = APPLICATION_CONTEXT ( 'automotive_design' ) ;
#5011 = EDGE_CURVE ( 'NONE', #7329, #6434, #27259, .T. ) ;
#5012 = CARTESIAN_POINT ( 'NONE',  ( 5.151948548241254144, 19.34356600583523544, 5.661398277488802755 ) ) ;
#5013 = DIRECTION ( 'NONE',  ( 0.000000000000000000, 0.000000000000000000, -1.000000000000000000 ) ) ;
#5014 = DIRECTION ( 'NONE',  ( 0.000000000000000000, 0.000000000000000000, 1.000000000000000000 ) ) ;
#5015 = DIRECTION ( 'NONE',  ( 0.000000000000000000, 0.000000000000000000, 1.000000000000000000 ) ) ;
#5016 = CIRCLE ( 'NONE', #9011, 9.482273699623480212 ) ;
#5017 = CARTESIAN_POINT ( 'NONE',  ( 1.112485354161228759E-15, -9.084132297865680883, 65.52304386563415051 ) ) ;
#5018 = LINE ( 'NONE', #14375, #17850 ) ;
#5019 = VERTEX_POINT ( 'NONE', #26627 ) ;
#5020 = CYLINDRICAL_SURFACE ( 'NONE', #1359, 1.447898107987198646 ) ;
#5021 = CARTESIAN_POINT ( 'NONE',  ( -23.96732207938974213, -33.98584080153308662, -1.500000000000000000 ) ) ;
#5022 = DIRECTION ( 'NONE',  ( 0.000000000000000000, 0.000000000000000000, 1.000000000000000000 ) ) ;
#5023 = ORIENTED_EDGE ( 'NONE', *, *, #28486, .F. ) ;
#5024 = CARTESIAN_POINT ( 'NONE',  ( -8.752572334588105463, 2.431858781452820306, -1.500000000000001554 ) ) ;
#5025 = CARTESIAN_POINT ( 'NONE',  ( -17.70591931088123516, -9.338465149306660606, 19.97651184436794125 ) ) ;
#5026 = ADVANCED_FACE ( 'NONE', ( #15061 ), #16950, .F. ) ;
#5027 = CARTESIAN_POINT ( 'NONE',  ( -5.349779314757643789, -7.341751895053219457, 13.22130136205108819 ) ) ;
#5028 = ADVANCED_FACE ( 'NONE', ( #24731 ), #7753, .F. ) ;
#5029 = DIRECTION ( 'NONE',  ( -0.000000000000000000, 1.000000000000000000, -0.000000000000000000 ) ) ;
#5030 = CARTESIAN_POINT ( 'NONE',  ( -12.56641067637752229, 40.32935944495016400, -1.500000000000000000 ) ) ;
#5031 = EDGE_LOOP ( 'NONE', ( #26106, #4757, #2029, #7902 ) ) ;
#5032 = ADVANCED_FACE ( 'NONE', ( #8064 ), #3068, .F. ) ;
#5033 = CARTESIAN_POINT ( 'NONE',  ( 0.000000000000000000, 0.000000000000000000, 1.500000000000001332 ) ) ;
#5034 = EDGE_CURVE ( 'NONE', #3349, #22024, #10832, .T. ) ;
#5035 = CARTESIAN_POINT ( 'NONE',  ( 22.67433715982020459, 34.69950560126978445, 29.56729215824071488 ) ) ;
#5036 = CARTESIAN_POINT ( 'NONE',  ( 19.58271949849003590, 4.064458250759529712, 7.161525567826888761 ) ) ;
#5037 = ORIENTED_EDGE ( 'NONE', *, *, #20349, .F. ) ;
#5038 = CIRCLE ( 'NONE', #21514, 1.447898107987198646 ) ;
#5039 = B_SPLINE_CURVE_WITH_KNOTS ( 'NONE', 3,
 ( #18982, #7588, #2445, #17089 ),
 .UNSPECIFIED., .F., .F.,
 ( 4, 4 ),
 ( 2.143643656977390230E-07, 0.003421830178490239353 ),
 .UNSPECIFIED. ) ;
#5040 = AXIS2_PLACEMENT_3D ( 'NONE', #16169, #25068, #25684 ) ;
#5041 = CARTESIAN_POINT ( 'NONE',  ( 7.500000000000000000, 5.196152422706634688, -9.000000000000001776 ) ) ;
#5042 = ORIENTED_EDGE ( 'NONE', *, *, #2561, .T. ) ;
#5043 = DIRECTION ( 'NONE',  ( -0.000000000000000000, -0.000000000000000000, 1.000000000000000000 ) ) ;
#5044 = DIRECTION ( 'NONE',  ( 0.000000000000000000, 0.000000000000000000, 1.000000000000000000 ) ) ;
#5045 = ORIENTED_EDGE ( 'NONE', *, *, #29382, .T. ) ;
#5046 = EDGE_LOOP ( 'NONE', ( #12211, #4039 ) ) ;
#5047 = DIRECTION ( 'NONE',  ( 0.6548607339452783282, -0.7557495743542641531, 0.000000000000000000 ) ) ;
#5048 = EDGE_LOOP ( 'NONE', ( #9836, #284, #24707, #405, #25214 ) ) ;
#5049 = ORIENTED_EDGE ( 'NONE', *, *, #26547, .T. ) ;
#5050 = ORIENTED_EDGE ( 'NONE', *, *, #25458, .T. ) ;
#5051 = LINE ( 'NONE', #26101, #2914 ) ;
#5052 = CARTESIAN_POINT ( 'NONE',  ( -7.870033247355589623, -15.14769711951103304, 7.280727868105637768 ) ) ;
#5053 = CARTESIAN_POINT ( 'NONE',  ( 0.000000000000000000, 0.000000000000000000, 92.49999999999998579 ) ) ;
#5054 = CARTESIAN_POINT ( 'NONE',  ( 1.342146863054723971, -19.97260970722470219, 19.58863275299554019 ) ) ;
#5055 = ORIENTED_EDGE ( 'NONE', *, *, #28673, .F. ) ;
#5056 = CARTESIAN_POINT ( 'NONE',  ( 4.045242219987652987, 16.55840560649981441, 5.652196082368482699 ) ) ;
#5057 = CARTESIAN_POINT ( 'NONE',  ( 23.22298177387596141, 35.92225147269209629, -14.83329744754546375 ) ) ;
#5058 = CARTESIAN_POINT ( 'NONE',  ( 11.72050123711541225, 12.41739018441317199, 18.92976555901915603 ) ) ;
#5059 = CARTESIAN_POINT ( 'NONE',  ( 8.260402557893151254, 8.184276679720483116, -1.500000000000000000 ) ) ;
#5060 = ORIENTED_EDGE ( 'NONE', *, *, #4812, .F. ) ;
#5061 = ADVANCED_FACE ( 'NONE', ( #9936 ), #879, .F. ) ;
#5062 = EDGE_CURVE ( 'NONE', #11207, #18139, #5863, .T. ) ;
#5063 = ADVANCED_BREP_SHAPE_REPRESENTATION ( '', ( #2811, #7396 ), #11893 ) ;
#5064 = VECTOR ( 'NONE', #23251, 1000.000000000000000 ) ;
#5065 = CARTESIAN_POINT ( 'NONE',  ( 11.80555446153501897, -11.55276080277260320, 24.50000000000000000 ) ) ;
#5066 = CARTESIAN_POINT ( 'NONE',  ( -15.06439250341027858, -7.989583865232171789, 5.678370764302467677 ) ) ;
#5067 = CARTESIAN_POINT ( 'NONE',  ( -6.789382699754177963, 18.83122862112907114, 7.196036389296800451 ) ) ;
#5068 = CARTESIAN_POINT ( 'NONE',  ( -23.16720440049831709, -10.90834004837188154, 49.39346268393973816 ) ) ;
#5069 = DIRECTION ( 'NONE',  ( -0.000000000000000000, 1.000000000000000000, -0.000000000000000000 ) ) ;
#5070 = CARTESIAN_POINT ( 'NONE',  ( 37.16608720827707657, 51.86186943028246787, 97.07879600563551037 ) ) ;
#5071 = ORIENTED_EDGE ( 'NONE', *, *, #5596, .T. ) ;
#5072 = EDGE_LOOP ( 'NONE', ( #23650, #17074, #10196, #11676 ) ) ;
#5073 = CARTESIAN_POINT ( 'NONE',  ( -40.00000000000000000, 90.00000000000001421, 59.49999999999999289 ) ) ;
#5074 = CARTESIAN_POINT ( 'NONE',  ( 35.76344986163714168, -22.29344514668044752, -19.50000000000000355 ) ) ;
#5075 = CARTESIAN_POINT ( 'NONE',  ( 1.195154792889394635, 9.406652940105990623, 13.00000000000000178 ) ) ;
#5077 = CYLINDRICAL_SURFACE ( 'NONE', #10597, 1.447898107987198646 ) ;
#5076 = VECTOR ( 'NONE', #21496, 1000.000000000000000 ) ;
#5078 = VERTEX_POINT ( 'NONE', #17102 ) ;
#5079 = PRODUCT_CONTEXT ( 'NONE', #7195, 'mechanical' ) ;
#5080 = CARTESIAN_POINT ( 'NONE',  ( 16.12090643793933964, -5.615848544254287589, 19.96568007040468373 ) ) ;
#5081 = DIRECTION ( 'NONE',  ( 1.000000000000000000, -0.000000000000000000, 0.000000000000000000 ) ) ;
#5082 = VERTEX_POINT ( 'NONE', #7596 ) ;
#5083 = CARTESIAN_POINT ( 'NONE',  ( 4.159666964149443480, 16.52698801271857221, 20.34789198813115263 ) ) ;
#5084 = CARTESIAN_POINT ( 'NONE',  ( 14.26939381558975484, 14.03892697587676786, 7.098451512883313441 ) ) ;
#5085 = CIRCLE ( 'NONE', #10565, 9.084132297865673777 ) ;
#5086 = CARTESIAN_POINT ( 'NONE',  ( -8.321991900554296606, -14.88664253293455353, 18.34938820207545263 ) ) ;
#5087 = CARTESIAN_POINT ( 'NONE',  ( -22.90437772071893363, 29.69852781866232760, 37.50000000002601297 ) ) ;
#5088 = EDGE_LOOP ( 'NONE', ( #29820, #29190, #17479, #29943 ) ) ;
#5089 = CARTESIAN_POINT ( 'NONE',  ( -24.35970437652574105, -13.37404834226503070, 47.21042702067970254 ) ) ;
#5090 = B_SPLINE_CURVE_WITH_KNOTS ( 'NONE', 3,
 ( #2770, #5570, #15066, #5260, #24581, #3224, #29437, #17108, #1047, #20065, #29585, #7601, #8217, #14761, #21787, #425, #9943, #720 ),
 .UNSPECIFIED., .F., .F.,
 ( 4, 2, 2, 2, 2, 2, 2, 2, 4 ),
 ( 0.000000000000000000, 0.0003967869494442915167, 0.0007935738988885830333, 0.001190360848332874550, 0.001587147797777166067, 0.001983934747221457583, 0.002380721696665749100, 0.002777508646110040617, 0.003174295595554332133 ),
 .UNSPECIFIED. ) ;
#5091 = CARTESIAN_POINT ( 'NONE',  ( 8.413215745754998309, -3.196529495465417980, 1.500000000000001332 ) ) ;
#5092 = CARTESIAN_POINT ( 'NONE',  ( 21.14235806497239167, 37.62311247503154021, -16.49999999999999645 ) ) ;
#5093 = ORIENTED_EDGE ( 'NONE', *, *, #10026, .F. ) ;
#5094 = LINE ( 'NONE', #26142, #337 ) ;
#5095 = DIRECTION ( 'NONE',  ( -1.000000000000000000, 0.000000000000000000, -0.000000000000000000 ) ) ;
#5096 = CARTESIAN_POINT ( 'NONE',  ( 14.53924466656744663, 13.73408656550489759, 7.528076282304593470 ) ) ;
#5097 = CIRCLE ( 'NONE', #1113, 21.71568325578193637 ) ;
#5098 = CARTESIAN_POINT ( 'NONE',  ( 0.6691466709101926424, -17.02906906675068299, 5.657991946698900598 ) ) ;
#5099 = EDGE_CURVE ( 'NONE', #10066, #1290, #24575, .T. ) ;
#5100 = FACE_OUTER_BOUND ( 'NONE', #23941, .T. ) ;
#5101 = FACE_OUTER_BOUND ( 'NONE', #8027, .T. ) ;
#5102 = LINE ( 'NONE', #14613, #3038 ) ;
#5103 = CARTESIAN_POINT ( 'NONE',  ( -77.99999999999998579, -42.49999999999998579, 32.33822642395377045 ) ) ;
#5104 = ORIENTED_EDGE ( 'NONE', *, *, #17397, .F. ) ;
#5105 = FACE_OUTER_BOUND ( 'NONE', #4450, .T. ) ;
#5106 = DIRECTION ( 'NONE',  ( 1.000000000000000000, 0.000000000000000000, 0.000000000000000000 ) ) ;
#5107 = VERTEX_POINT ( 'NONE', #2920 ) ;
#5108 = ORIENTED_EDGE ( 'NONE', *, *, #10925, .F. ) ;
#5109 = DIRECTION ( 'NONE',  ( 0.000000000000000000, 0.000000000000000000, 1.000000000000000000 ) ) ;
#5110 = DIRECTION ( 'NONE',  ( 1.000000000000000000, 0.000000000000000000, 0.000000000000000000 ) ) ;
#5111 = EDGE_LOOP ( 'NONE', ( #12334, #25103 ) ) ;
#5112 = CARTESIAN_POINT ( 'NONE',  ( 14.97341519046260316, 13.28616376876794725, 20.34789198813115263 ) ) ;
#5113 = AXIS2_PLACEMENT_3D ( 'NONE', #24196, #5189, #8006 ) ;
#5114 = VECTOR ( 'NONE', #18706, 1000.000000000000000 ) ;
#5115 = FILL_AREA_STYLE_COLOUR ( '', #13923 ) ;
#5116 = EDGE_LOOP ( 'NONE', ( #21681, #28520, #6220, #13437 ) ) ;
#5117 = AXIS2_PLACEMENT_3D ( 'NONE', #12449, #17429, #885 ) ;
#5118 = CARTESIAN_POINT ( 'NONE',  ( 31.61046531696969808, 26.43913157123721192, -9.833326301035395289 ) ) ;
#5119 = CARTESIAN_POINT ( 'NONE',  ( 19.63091490780798765, 3.916522693408248657, 18.64703902303423178 ) ) ;
#5120 = CARTESIAN_POINT ( 'NONE',  ( -15.71962203721309592, -1.249857212218242752, 24.50000000000000000 ) ) ;
#5121 =( BOUNDED_SURFACE ( )  B_SPLINE_SURFACE ( 3, 1, ( 
 ( #19077, #19390 ),
 ( #28595, #12534 ),
 ( #14228, #663 ),
 ( #12065, #26094 ) ),
 .UNSPECIFIED., .F., .F., .F. ) 
 B_SPLINE_SURFACE_WITH_KNOTS ( ( 4, 4 ),
 ( 2, 2 ),
 ( 0.000000000000000000, 1.000000000000000000 ),
 ( 0.000000000000000000, 1.000000000000000000 ),
 .UNSPECIFIED. ) 
 GEOMETRIC_REPRESENTATION_ITEM ( )  RATIONAL_B_SPLINE_SURFACE ( (
 ( 1.000000000000000000, 1.000000000000000000),
 ( 0.8179194830933627092, 0.8179194830933627092),
 ( 0.8179194830933627092, 0.8179194830933627092),
 ( 1.000000000000000000, 1.000000000000000000) ) ) 
 REPRESENTATION_ITEM ( '' )  SURFACE ( )  );
#5122 = ORIENTED_EDGE ( 'NONE', *, *, #4218, .F. ) ;
#5123 = CARTESIAN_POINT ( 'NONE',  ( 23.07593096178833747, -11.40900259639455605, 45.01551998640317009 ) ) ;
#5124 = ORIENTED_EDGE ( 'NONE', *, *, #7088, .F. ) ;
#5125 = EDGE_LOOP ( 'NONE', ( #29214, #24225, #27771, #17870 ) ) ;
#5126 = CARTESIAN_POINT ( 'NONE',  ( 9.163215745754998309, -3.196529495465417980, 21.50000000000000000 ) ) ;
#5127 = CARTESIAN_POINT ( 'NONE',  ( -17.76782356872499591, -9.182228809334526787, 7.454606537396346155 ) ) ;
#5128 = LINE ( 'NONE', #12624, #8774 ) ;
#5129 = DIRECTION ( 'NONE',  ( -1.000000000000000000, 0.000000000000000000, 0.000000000000000000 ) ) ;
#5130 = CIRCLE ( 'NONE', #22562, 7.500000000000000000 ) ;
#5131 = DIRECTION ( 'NONE',  ( 1.000000000000000000, 0.000000000000000000, -0.000000000000000000 ) ) ;
#5132 = CARTESIAN_POINT ( 'NONE',  ( 8.637616862297843312, -3.912171961291978306, 1.500000000000001332 ) ) ;
#5133 = ORIENTED_EDGE ( 'NONE', *, *, #13621, .T. ) ;
#5134 = EDGE_CURVE ( 'NONE', #7128, #10711, #17828, .T. ) ;
#5135 = CARTESIAN_POINT ( 'NONE',  ( 10.33891776879019986, -17.14136798460503996, 7.080843742048788414 ) ) ;
#5136 = CARTESIAN_POINT ( 'NONE',  ( 34.17252016804844317, -12.46427775875993937, 34.49999999999999289 ) ) ;
#5137 = LINE ( 'NONE', #2493, #21771 ) ;
#5138 = EDGE_LOOP ( 'NONE', ( #18048, #9564, #12206, #9985 ) ) ;
#5139 = VERTEX_POINT ( 'NONE', #3376 ) ;
#5140 = DIRECTION ( 'NONE',  ( 0.4539545692076743522, 0.8910248307962438385, -0.000000000000000000 ) ) ;
#5141 = CARTESIAN_POINT ( 'NONE',  ( 10.68225562352957070, -16.90870462272443575, 7.526993102356321685 ) ) ;
#5142 = CARTESIAN_POINT ( 'NONE',  ( -5.548724899233040908, 19.23375410423647836, 7.557577766377196582 ) ) ;
#5143 = PLANE ( 'NONE',  #2665 ) ;
#5144 = CARTESIAN_POINT ( 'NONE',  ( 0.1482032042127267857, 2.204400401860220793, -9.000000000000001776 ) ) ;
#5145 = ORIENTED_EDGE ( 'NONE', *, *, #9638, .F. ) ;
#5146 = VERTEX_POINT ( 'NONE', #10400 ) ;
#5147 = VECTOR ( 'NONE', #26430, 1000.000000000000000 ) ;
#5148 = CARTESIAN_POINT ( 'NONE',  ( -29.56528975567554696, -22.55618809495488009, 34.49999999999999289 ) ) ;
#5149 = FACE_OUTER_BOUND ( 'NONE', #26061, .T. ) ;
#5150 = CARTESIAN_POINT ( 'NONE',  ( 24.03057240117690441, -26.57182937991349903, 24.50000000000000000 ) ) ;
#5151 = ORIENTED_EDGE ( 'NONE', *, *, #14931, .T. ) ;
#5152 = DIRECTION ( 'NONE',  ( 0.000000000000000000, 0.000000000000000000, 1.000000000000000000 ) ) ;
#5153 = CIRCLE ( 'NONE', #7146, 0.7441270634456903510 ) ;
#5154 = ORIENTED_EDGE ( 'NONE', *, *, #551, .F. ) ;
#5155 = CARTESIAN_POINT ( 'NONE',  ( 18.59495189863232412, -7.412450086248064451, 7.441806358946449151 ) ) ;
#5156 = CIRCLE ( 'NONE', #25089, 1.447898107987170890 ) ;
#5157 = UNCERTAINTY_MEASURE_WITH_UNIT (LENGTH_MEASURE( 1.000000000000000082E-05 ), #433, 'distance_accuracy_value', 'NONE');
#5158 = FACE_OUTER_BOUND ( 'NONE', #14662, .T. ) ;
#5159 = EDGE_CURVE ( 'NONE', #1292, #21299, #24291, .T. ) ;
#5160 = CARTESIAN_POINT ( 'NONE',  ( 3.118309183252346628, -17.14266753270391774, 1.500000000000000000 ) ) ;
#5161 = ORIENTED_EDGE ( 'NONE', *, *, #26331, .F. ) ;
#5162 = EDGE_CURVE ( 'NONE', #15220, #9060, #714, .T. ) ;
#5163 = CARTESIAN_POINT ( 'NONE',  ( 4.972463595808061854, 19.39063357279558275, 5.704143890883081269 ) ) ;
#5164 = EDGE_CURVE ( 'NONE', #624, #11023, #30257, .T. ) ;
#5165 = DIRECTION ( 'NONE',  ( 0.000000000000000000, -1.132880637372608986E-16, 1.000000000000000000 ) ) ;
#5166 = DIRECTION ( 'NONE',  ( 0.000000000000000000, -0.000000000000000000, -1.000000000000000000 ) ) ;
#5167 = CARTESIAN_POINT ( 'NONE',  ( 0.000000000000000000, 12.18947652193946851, 29.43090101791767665 ) ) ;
#5168 = CARTESIAN_POINT ( 'NONE',  ( -1.734723475976807094E-15, -44.07656352898514740, -6.500000000000000888 ) ) ;
#5169 = ADVANCED_FACE ( 'NONE', ( #22400 ), #19744, .F. ) ;
#5170 = CARTESIAN_POINT ( 'NONE',  ( 10.58932223943304685, -16.96688107778387078, 18.54479204710284179 ) ) ;
#5171 = EDGE_LOOP ( 'NONE', ( #3384, #908, #26832, #3749 ) ) ;
#5172 = EDGE_CURVE ( 'NONE', #2517, #27291, #16812, .T. ) ;
#5173 = DIRECTION ( 'NONE',  ( 0.000000000000000000, 0.000000000000000000, 1.000000000000000000 ) ) ;
#5174 = CARTESIAN_POINT ( 'NONE',  ( 34.99999999999933920, 4.286263797015655244E-15, 92.49999999999998579 ) ) ;
#5175 = CARTESIAN_POINT ( 'NONE',  ( 10.11202017158399968, 41.14070756921128691, -1.500000000000000000 ) ) ;
#5176 = DIRECTION ( 'NONE',  ( 1.000000000000000000, 0.000000000000000000, -0.000000000000000000 ) ) ;
#5177 = ORIENTED_EDGE ( 'NONE', *, *, #5968, .F. ) ;
#5178 = VECTOR ( 'NONE', #18475, 1000.000000000000000 ) ;
#5179 = CARTESIAN_POINT ( 'NONE',  ( -70.00000000000000000, -50.00000000000000000, -92.50000000000000000 ) ) ;
#5181 = ADVANCED_FACE ( 'NONE', ( #22691, #22856 ), #15842, .T. ) ;
#5180 = DIRECTION ( 'NONE',  ( -0.000000000000000000, -0.000000000000000000, 1.000000000000000000 ) ) ;
#5182 = AXIS2_PLACEMENT_3D ( 'NONE', #19514, #24649, #22310 ) ;
#5183 = DIRECTION ( 'NONE',  ( 1.000000000000000000, 0.000000000000000000, 0.000000000000000000 ) ) ;
#5184 = FACE_OUTER_BOUND ( 'NONE', #17156, .T. ) ;
#5185 = CARTESIAN_POINT ( 'NONE',  ( -10.11202017158235833, -41.14070756921188377, -1.500000000000000000 ) ) ;
#5186 = EDGE_CURVE ( 'NONE', #23254, #15912, #894, .T. ) ;
#5187 = ADVANCED_FACE ( 'NONE', ( #8374 ), #27235, .T. ) ;
#5188 = CARTESIAN_POINT ( 'NONE',  ( 38.93535427911099589, 2.534171857450247423, 35.07262524311201446 ) ) ;
#5189 = DIRECTION ( 'NONE',  ( -0.000000000000000000, 0.000000000000000000, 1.000000000000000000 ) ) ;
#5190 = ORIENTED_EDGE ( 'NONE', *, *, #4599, .F. ) ;
#5191 = CARTESIAN_POINT ( 'NONE',  ( 33.78553947564427773, -24.40792753551981775, -16.50000000000000000 ) ) ;
#5192 = EDGE_LOOP ( 'NONE', ( #14605, #10358 ) ) ;
#5193 = CARTESIAN_POINT ( 'NONE',  ( -14.41708049311053053, 17.22181377296911720, 1.500000000000000000 ) ) ;
#5194 = CARTESIAN_POINT ( 'NONE',  ( 38.00000000000000711, 209.2686044187655909, -87.50000000000000000 ) ) ;
#5195 = APPLICATION_CONTEXT ( 'automotive_design' ) ;
#5196 = VERTEX_POINT ( 'NONE', #29727 ) ;
#5197 = ORIENTED_EDGE ( 'NONE', *, *, #2117, .F. ) ;
#5198 = ORIENTED_EDGE ( 'NONE', *, *, #4973, .T. ) ;
#5199 = PRODUCT ( 'Cam Ring Elliptical Outer Ring', 'Cam Ring Elliptical Outer Ring', '', ( #24403 ) ) ;
#5200 = ORIENTED_EDGE ( 'NONE', *, *, #8775, .T. ) ;
#5201 = ORIENTED_EDGE ( 'NONE', *, *, #28277, .F. ) ;
#5202 = CARTESIAN_POINT ( 'NONE',  ( -0.2093543646724285723, -17.02041581256300873, 19.11611934778430921 ) ) ;
#5203 = AXIS2_PLACEMENT_3D ( 'NONE', #30843, #4650, #26327 ) ;
#5204 = ADVANCED_FACE ( 'NONE', ( #5871 ), #23001, .F. ) ;
#5205 = CARTESIAN_POINT ( 'NONE',  ( -25.47847050916411504, 26.57182937991348481, -6.499999999999999112 ) ) ;
#5206 = EDGE_CURVE ( 'NONE', #3904, #26649, #2876, .T. ) ;
#5207 = CARTESIAN_POINT ( 'NONE',  ( -3.469446951953614189E-15, -30.50000000000000711, 1.500000000000000000 ) ) ;
#5208 = CYLINDRICAL_SURFACE ( 'NONE', #28803, 0.7500000000000006661 ) ;
#5209 = CARTESIAN_POINT ( 'NONE',  ( -21.37787209074186734, 24.17206580633116175, -16.50001200000000168 ) ) ;
#5210 = ORIENTED_EDGE ( 'NONE', *, *, #14701, .F. ) ;
#5211 = CARTESIAN_POINT ( 'NONE',  ( 23.05654803991950175, 35.38768971483871439, -9.833278432202751773 ) ) ;
#5212 = DIRECTION ( 'NONE',  ( 0.000000000000000000, 0.000000000000000000, 1.000000000000000000 ) ) ;
#5213 = CARTESIAN_POINT ( 'NONE',  ( 14.29853178503252309, 14.00938365128603458, 18.82680253904184298 ) ) ;
#5214 = DIRECTION ( 'NONE',  ( 1.000000000000000000, 0.000000000000000000, 0.000000000000000000 ) ) ;
#5215 = ORIENTED_EDGE ( 'NONE', *, *, #21350, .F. ) ;
#5216 = EDGE_CURVE ( 'NONE', #20799, #22863, #20516, .T. ) ;
#5217 = CARTESIAN_POINT ( 'NONE',  ( -10.52692833102915770, -17.02631732661572883, 20.34789198813115263 ) ) ;
#5218 = LINE ( 'NONE', #2416, #23226 ) ;
#5219 = DIRECTION ( 'NONE',  ( -0.7557495743542579358, 0.6548607339452855447, 0.000000000000000000 ) ) ;
#5220 = DIRECTION ( 'NONE',  ( -0.000000000000000000, -0.000000000000000000, -1.000000000000000000 ) ) ;
#5221 = CARTESIAN_POINT ( 'NONE',  ( -17.75446986341067301, 9.207540381081360081, 1.500000000000001332 ) ) ;
#5222 = EDGE_CURVE ( 'NONE', #23472, #5078, #9844, .T. ) ;
#5223 = DIRECTION ( 'NONE',  ( 0.000000000000000000, 0.000000000000000000, 1.000000000000000000 ) ) ;
#5224 = DIRECTION ( 'NONE',  ( -1.000000000000000000, 0.000000000000000000, 0.000000000000000000 ) ) ;
#5225 = ORIENTED_EDGE ( 'NONE', *, *, #9404, .F. ) ;
#5226 = VERTEX_POINT ( 'NONE', #6326 ) ;
#5227 = LINE ( 'NONE', #14433, #24389 ) ;
#5228 = VECTOR ( 'NONE', #22063, 1000.000000000000000 ) ;
#5229 = CARTESIAN_POINT ( 'NONE',  ( -8.325649706230674241, -14.88445757356298493, 7.652108011868850035 ) ) ;
#5230 = CARTESIAN_POINT ( 'NONE',  ( -13.16038179581985723, 10.81844819380990330, 7.595116371587256054 ) ) ;
#5231 = DIRECTION ( 'NONE',  ( 0.000000000000000000, 1.000000000000000000, 0.000000000000000000 ) ) ;
#5232 = EDGE_LOOP ( 'NONE', ( #2676, #23041 ) ) ;
#5233 = SHAPE_DEFINITION_REPRESENTATION ( #23350, #10497 ) ;
#5234 = CARTESIAN_POINT ( 'NONE',  ( -3.993622308618941741, -8.159193615868385763, 13.22130136205108641 ) ) ;
#5235 = CARTESIAN_POINT ( 'NONE',  ( -22.58267429318970443, -26.57182937991348481, 1.500000000000001332 ) ) ;
#5236 = EDGE_CURVE ( 'NONE', #15112, #21717, #8365, .T. ) ;
#5237 = ORIENTED_EDGE ( 'NONE', *, *, #16413, .T. ) ;
#5238 = CARTESIAN_POINT ( 'NONE',  ( 6.249808329856146649, 19.01727106391103916, 19.11611934778430921 ) ) ;
#5239 = EDGE_CURVE ( 'NONE', #26950, #3989, #374, .T. ) ;
#5240 = DIRECTION ( 'NONE',  ( 0.000000000000000000, 0.000000000000000000, 1.000000000000000000 ) ) ;
#5241 = ADVANCED_FACE ( 'NONE', ( #25046 ), #6022, .F. ) ;
#5242 = FACE_OUTER_BOUND ( 'NONE', #28065, .T. ) ;
#5243 = CARTESIAN_POINT ( 'NONE',  ( -37.84083111920662645, -10.30891341277128248, 34.96466318893187264 ) ) ;
#5244 = ORIENTED_EDGE ( 'NONE', *, *, #19672, .F. ) ;
#5245 = CARTESIAN_POINT ( 'NONE',  ( -23.21352257770656990, 10.78826658734919519, 49.40206402021039622 ) ) ;
#5246 = CARTESIAN_POINT ( 'NONE',  ( 33.36692087966583387, 9.471517865689168758, 36.07226619909889820 ) ) ;
#5247 = CARTESIAN_POINT ( 'NONE',  ( 19.81910295759737295, 38.46425637429425848, -16.50000000000000711 ) ) ;
#5248 = ORIENTED_EDGE ( 'NONE', *, *, #18916, .F. ) ;
#5249 = CARTESIAN_POINT ( 'NONE',  ( -15.51812306427841293, -7.001296657735112561, 6.111214848085761986 ) ) ;
#5250 = CIRCLE ( 'NONE', #26664, 0.6002263538043648428 ) ;
#5251 = CARTESIAN_POINT ( 'NONE',  ( 0.000000000000000000, 0.000000000000000000, 1.500000000000000000 ) ) ;
#5252 = DIRECTION ( 'NONE',  ( 1.000000000000000000, 0.000000000000000000, 0.000000000000000000 ) ) ;
#5253 = CARTESIAN_POINT ( 'NONE',  ( 7.500000000000000000, -10.39230484541329247, 8.776157072412030708E-17 ) ) ;
#5254 = FACE_OUTER_BOUND ( 'NONE', #14795, .T. ) ;
#5255 = DIRECTION ( 'NONE',  ( 0.6548607339452890974, 0.7557495743542548272, 0.000000000000000000 ) ) ;
#5256 = CARTESIAN_POINT ( 'NONE',  ( 37.70070167288648122, -10.88189949536004342, 14.68280373647734116 ) ) ;
#5257 = CARTESIAN_POINT ( 'NONE',  ( -50.00000000000000000, -70.00000000000000000, 12.49999999999999112 ) ) ;
#5258 = ORIENTED_EDGE ( 'NONE', *, *, #21763, .T. ) ;
#5259 = CARTESIAN_POINT ( 'NONE',  ( 6.301234758012599357, -6.543385983536367689, 21.50000000000000000 ) ) ;
#5260 = CARTESIAN_POINT ( 'NONE',  ( 4.800123045415255696, 19.41580659536132103, 5.779535427900766464 ) ) ;
#5261 = ORIENTED_EDGE ( 'NONE', *, *, #25949, .T. ) ;
#5262 = VERTEX_POINT ( 'NONE', #20058 ) ;
#5263 = DIRECTION ( 'NONE',  ( -0.9096319953545183301, -0.4154150130018863796, -0.000000000000000000 ) ) ;
#5264 = FACE_OUTER_BOUND ( 'NONE', #12664, .T. ) ;
#5265 = ORIENTED_EDGE ( 'NONE', *, *, #18963, .T. ) ;
#5266 = CARTESIAN_POINT ( 'NONE',  ( 13.01404215953673571, 10.97082360537801193, 19.45164628100866722 ) ) ;
#5267 = VECTOR ( 'NONE', #14540, 1000.000000000000000 ) ;
#5268 = CARTESIAN_POINT ( 'NONE',  ( -11.06207408980607276, -16.68369011021418302, 7.429667576816606278 ) ) ;
#5269 = ORIENTED_EDGE ( 'NONE', *, *, #7968, .F. ) ;
#5270 = CARTESIAN_POINT ( 'NONE',  ( 32.08353429860093797, 26.68014822794475549, -14.83332872293874871 ) ) ;
#5271 = CARTESIAN_POINT ( 'NONE',  ( -15.73346977245379819, 12.34774510571039308, 20.15039051365863898 ) ) ;
#5272 = CIRCLE ( 'NONE', #16241, 6.000000000000001776 ) ;
#5273 = ADVANCED_FACE ( 'NONE', ( #29579 ), #11169, .F. ) ;
#5274 = DIRECTION ( 'NONE',  ( 0.000000000000000000, 0.000000000000000000, -1.000000000000000000 ) ) ;
#5275 = EDGE_LOOP ( 'NONE', ( #19433, #28369, #19966, #29124 ) ) ;
#5276 = EDGE_CURVE ( 'NONE', #20799, #23754, #17713, .T. ) ;
#5277 = CARTESIAN_POINT ( 'NONE',  ( 6.974883619896790954, 5.687793815610376669, 21.50000000000000000 ) ) ;
#5278 = ORIENTED_EDGE ( 'NONE', *, *, #25507, .F. ) ;
#5279 = VECTOR ( 'NONE', #8978, 1000.000000000000000 ) ;
#5280 = ORIENTED_EDGE ( 'NONE', *, *, #2149, .T. ) ;
#5281 = DIRECTION ( 'NONE',  ( -0.1430297813019457409, -0.9897183850271336070, 0.000000000000000000 ) ) ;
#5282 = CARTESIAN_POINT ( 'NONE',  ( -6.359874605901119082, 15.84393421166758742, 19.89182036555910571 ) ) ;
#5283 = CARTESIAN_POINT ( 'NONE',  ( -14.99868389510896982, 13.25752457422374597, 20.19668224736330941 ) ) ;
#5284 = FACE_OUTER_BOUND ( 'NONE', #385, .T. ) ;
#5285 = DIRECTION ( 'NONE',  ( 0.9329908884337542174, -0.3598999890241648125, 0.000000000000000000 ) ) ;
#5286 = CYLINDRICAL_SURFACE ( 'NONE', #4521, 45.00000000000000711 ) ;
#5287 = CARTESIAN_POINT ( 'NONE',  ( 69.99999999999998579, -50.00000000000000000, 59.49999999999999289 ) ) ;
#5288 = ORIENTED_EDGE ( 'NONE', *, *, #28220, .T. ) ;
#5289 = CARTESIAN_POINT ( 'NONE',  ( 9.331524088667746852, -14.24511854140750522, 5.862424720655265098 ) ) ;
#5290 = CARTESIAN_POINT ( 'NONE',  ( -28.00213357088913924, 29.58171923439856243, 13.43815007647722659 ) ) ;
#5291 = AXIS2_PLACEMENT_3D ( 'NONE', #23203, #1857, #18695 ) ;
#5292 = CARTESIAN_POINT ( 'NONE',  ( 19.85631519639702347, 2.394924755340403166, 7.267242832833948007 ) ) ;
#5293 = EDGE_LOOP ( 'NONE', ( #29784, #26572, #23619, #2932 ) ) ;
#5294 = ORIENTED_EDGE ( 'NONE', *, *, #10365, .F. ) ;
#5295 = CARTESIAN_POINT ( 'NONE',  ( -3.515970705488605130, -17.06554576617236307, 1.500000000000000000 ) ) ;
#5296 = CARTESIAN_POINT ( 'NONE',  ( 28.34828976096171971, 29.18752572968384129, -1.500000000000000000 ) ) ;
#5297 = CARTESIAN_POINT ( 'NONE',  ( 24.03057240117691862, 26.57182937991349903, -16.50000000000000000 ) ) ;
#5298 = FACE_OUTER_BOUND ( 'NONE', #20524, .T. ) ;
#5299 = DIRECTION ( 'NONE',  ( -0.000000000000000000, -0.000000000000000000, 1.000000000000000000 ) ) ;
#5300 = CIRCLE ( 'NONE', #23208, 0.7499999999999988898 ) ;
#5301 = CARTESIAN_POINT ( 'NONE',  ( 5.296161872597630271, 19.28602264385381204, 7.652108011868850035 ) ) ;
#5302 = ORIENTED_EDGE ( 'NONE', *, *, #22477, .F. ) ;
#5303 = DIRECTION ( 'NONE',  ( 0.000000000000000000, 0.000000000000000000, -1.000000000000000000 ) ) ;
#5304 = CARTESIAN_POINT ( 'NONE',  ( 8.860628911697515875, 8.184276679720483116, -1.500000000000000000 ) ) ;
#5305 = CARTESIAN_POINT ( 'NONE',  ( 18.33793066653144521, -7.982499537706466697, 5.652196082369965069 ) ) ;
#5306 = ORIENTED_EDGE ( 'NONE', *, *, #15767, .F. ) ;
#5307 = VECTOR ( 'NONE', #17672, 1000.000000000000000 ) ;
#5308 = CARTESIAN_POINT ( 'NONE',  ( -70.00000000000000000, 70.00000000000000000, -92.50000000000000000 ) ) ;
#5309 = ORIENTED_EDGE ( 'NONE', *, *, #8981, .F. ) ;
#5310 = CARTESIAN_POINT ( 'NONE',  ( 16.19464367748838640, -5.422319245274333177, 6.672349528511551497 ) ) ;
#5311 = CONICAL_SURFACE ( 'NONE', #30229, 35.37867965644036872, 0.7853981633974500554 ) ;
#5312 = CARTESIAN_POINT ( 'NONE',  ( -33.14492814497880602, 23.43596551657908122, -6.499906363187105462 ) ) ;
#5313 = VECTOR ( 'NONE', #19564, 1000.000000000000000 ) ;
#5314 = CARTESIAN_POINT ( 'NONE',  ( -12.86767874445213877, -1.850092897552710225, 24.50000000000000000 ) ) ;
#5315 = ORIENTED_EDGE ( 'NONE', *, *, #19878, .T. ) ;
#5316 = CARTESIAN_POINT ( 'NONE',  ( 77.99999999999998579, 42.50000000000000000, 1.500000000000000222 ) ) ;
#5317 = CARTESIAN_POINT ( 'NONE',  ( 6.899999999999999467, 5.196152422706624030, 9.000000000000001776 ) ) ;
#5318 = CARTESIAN_POINT ( 'NONE',  ( 15.41296542101254552, 5.939519782021115191, 24.50000000000000000 ) ) ;
#5319 = CARTESIAN_POINT ( 'NONE',  ( 12.86231920026284925, 36.90765539456646849, 34.50000000000000000 ) ) ;
#5320 = CIRCLE ( 'NONE', #26749, 9.084132297865673777 ) ;
#5321 = AXIS2_PLACEMENT_3D ( 'NONE', #11971, #19592, #26624 ) ;
#5322 = DIRECTION ( 'NONE',  ( -1.000000000000000000, 0.000000000000000000, 0.000000000000000000 ) ) ;
#5323 = CARTESIAN_POINT ( 'NONE',  ( -19.54426622602688468, -37.07991288358296345, 1.499999999999999778 ) ) ;
#5324 = CARTESIAN_POINT ( 'NONE',  ( -8.134323311075783991, -1.438332125858144295, -1.500000000000001776 ) ) ;
#5325 = ORIENTED_EDGE ( 'NONE', *, *, #6049, .T. ) ;
#5326 = CARTESIAN_POINT ( 'NONE',  ( 18.33599632111990729, -7.986941774664182425, 7.652108011868850035 ) ) ;
#5327 = DIRECTION ( 'NONE',  ( 0.000000000000000000, 0.000000000000000000, -1.000000000000000000 ) ) ;
#5328 = AXIS2_PLACEMENT_3D ( 'NONE', #21950, #12463, #14630 ) ;
#5329 = CARTESIAN_POINT ( 'NONE',  ( -40.89187623478217404, 5.790488632116478129, -19.50000000000000355 ) ) ;
#5330 = DIRECTION ( 'NONE',  ( 0.000000000000000000, -1.000000000000000000, 0.000000000000000000 ) ) ;
#5331 = ORIENTED_EDGE ( 'NONE', *, *, #6695, .F. ) ;
#5332 = CARTESIAN_POINT ( 'NONE',  ( 28.30074574513791674, -29.24255319736864323, 14.75302129891823988 ) ) ;
#5333 = CARTESIAN_POINT ( 'NONE',  ( 9.301547456646380496, 8.591538895647095941, 1.500000000000000000 ) ) ;
#5334 = CARTESIAN_POINT ( 'NONE',  ( -15.17333614897415650, 13.03014763290140721, 20.32243167357988867 ) ) ;
#5335 = CARTESIAN_POINT ( 'NONE',  ( 4.303751186762871939, 16.48600304569812991, 7.626437579292366209 ) ) ;
#5336 = CARTESIAN_POINT ( 'NONE',  ( 23.96732207937828463, 33.98584080152456011, -1.500000000000000000 ) ) ;
#5337 = FILL_AREA_STYLE ('',( #26559 ) ) ;
#5338 = CARTESIAN_POINT ( 'NONE',  ( 28.40292615218646688, 29.15708363699292249, 30.13690029699395012 ) ) ;
#5339 = CARTESIAN_POINT ( 'NONE',  ( -36.00000000000000000, -1.100768691257133318E-12, 34.75735931288076586 ) ) ;
#5340 = ORIENTED_EDGE ( 'NONE', *, *, #4808, .F. ) ;
#5341 = CIRCLE ( 'NONE', #25787, 1.447898107987198646 ) ;
#5342 = CARTESIAN_POINT ( 'NONE',  ( 127.5000000000000000, 0.000000000000000000, 0.000000000000000000 ) ) ;
#5343 = ORIENTED_EDGE ( 'NONE', *, *, #30546, .F. ) ;
#5344 = CIRCLE ( 'NONE', #20289, 2.061368542273053883 ) ;
#5345 = EDGE_CURVE ( 'NONE', #4954, #4066, #20204, .T. ) ;
#5346 = CARTESIAN_POINT ( 'NONE',  ( 27.03074382657074182, -6.449748410230990991, 42.96778633356034049 ) ) ;
#5347 = CYLINDRICAL_SURFACE ( 'NONE', #23379, 0.7500000000000006661 ) ;
#5348 = VERTEX_POINT ( 'NONE', #3537 ) ;
#5349 = ORIENTED_EDGE ( 'NONE', *, *, #12980, .T. ) ;
#5350 = AXIS2_PLACEMENT_3D ( 'NONE', #2827, #29029, #26538 ) ;
#5351 = CARTESIAN_POINT ( 'NONE',  ( 32.50000000000000000, 3.980102097228898626E-15, -87.50000000000000000 ) ) ;
#5352 = ADVANCED_FACE ( 'NONE', ( #13200 ), #13054, .T. ) ;
#5353 = EDGE_LOOP ( 'NONE', ( #729, #13270, #16495, #14119 ) ) ;
#5354 = AXIS2_PLACEMENT_3D ( 'NONE', #16823, #26336, #9959 ) ;
#5355 = ORIENTED_EDGE ( 'NONE', *, *, #25009, .F. ) ;
#5356 = EDGE_LOOP ( 'NONE', ( #7772, #14650, #7406, #29746 ) ) ;
#5357 = LINE ( 'NONE', #17364, #28800 ) ;
#5358 = CARTESIAN_POINT ( 'NONE',  ( -33.53437127389221928, 14.37219272518421853, 34.49999999999999289 ) ) ;
#5359 = CARTESIAN_POINT ( 'NONE',  ( 4.510281037539698445E-13, -4.926614671774132148E-13, 79.49999999999998579 ) ) ;
#5360 = VECTOR ( 'NONE', #13631, 1000.000000000000000 ) ;
#5361 = DIRECTION ( 'NONE',  ( 0.000000000000000000, -1.132880637372608986E-16, 1.000000000000000000 ) ) ;
#5362 = EDGE_CURVE ( 'NONE', #16582, #526, #11846, .T. ) ;
#5363 = ORIENTED_EDGE ( 'NONE', *, *, #24082, .F. ) ;
#5364 = EDGE_CURVE ( 'NONE', #30675, #11240, #25192, .T. ) ;
#5365 = CARTESIAN_POINT ( 'NONE',  ( -49.99999999999998579, 70.00000000000000000, -75.50000000000002842 ) ) ;
#5366 = DIRECTION ( 'NONE',  ( -1.000000000000000000, 0.000000000000000000, 0.000000000000000000 ) ) ;
#5367 = DIRECTION ( 'NONE',  ( -0.000000000000000000, -0.000000000000000000, 1.000000000000000000 ) ) ;
#5368 = CARTESIAN_POINT ( 'NONE',  ( 0.000000000000000000, 0.000000000000000000, -1.500000000000000000 ) ) ;
#5369 = AXIS2_PLACEMENT_3D ( 'NONE', #25176, #3673, #3821 ) ;
#5370 = ORIENTED_EDGE ( 'NONE', *, *, #1570, .F. ) ;
#5371 = CARTESIAN_POINT ( 'NONE',  ( -4.163336342344337027E-14, -1.387778780781445676E-14, -1.500000000000000000 ) ) ;
#5372 = CARTESIAN_POINT ( 'NONE',  ( -17.60607916434269526, -9.525343863633429109, 6.447548852708279377 ) ) ;
#5373 = CARTESIAN_POINT ( 'NONE',  ( -6.855891330591546762, 18.80700764124136271, 6.233981582756856987 ) ) ;
#5374 = DIRECTION ( 'NONE',  ( 1.000000000000000000, 0.000000000000000000, 0.000000000000000000 ) ) ;
#5375 = DIRECTION ( 'NONE',  ( 1.000000000000000000, 0.000000000000000000, 0.000000000000000000 ) ) ;
#5376 = DIRECTION ( 'NONE',  ( -0.000000000000000000, -0.000000000000000000, 1.000000000000000000 ) ) ;
#5377 = AXIS2_PLACEMENT_3D ( 'NONE', #17445, #26968, #5589 ) ;
#5378 = ORIENTED_EDGE ( 'NONE', *, *, #13579, .T. ) ;
#5379 = EDGE_LOOP ( 'NONE', ( #4794, #20659, #19453, #6625 ) ) ;
#5380 = VECTOR ( 'NONE', #12222, 1000.000000000000000 ) ;
#5381 = CARTESIAN_POINT ( 'NONE',  ( 0.000000000000000000, 0.000000000000000000, 1.500000000000000000 ) ) ;
#5382 = CARTESIAN_POINT ( 'NONE',  ( -5.380257496407078399, 19.26296000801971431, 18.54479204710283824 ) ) ;
#5383 = EDGE_CURVE ( 'NONE', #15220, #26699, #2383, .T. ) ;
#5384 = CARTESIAN_POINT ( 'NONE',  ( -9.185733585337896301, 2.352830851074203533, 21.50000000000000000 ) ) ;
#5385 = EDGE_CURVE ( 'NONE', #17362, #30019, #18909, .T. ) ;
#5386 = CARTESIAN_POINT ( 'NONE',  ( 0.000000000000000000, 0.000000000000000000, 1.500000000000001332 ) ) ;
#5387 = ORIENTED_EDGE ( 'NONE', *, *, #5617, .F. ) ;
#5388 = APPLICATION_PROTOCOL_DEFINITION ( 'draft international standard', 'automotive_design', 1998, #17357 ) ;
#5389 = EDGE_CURVE ( 'NONE', #6549, #28201, #6849, .T. ) ;
#5390 = CARTESIAN_POINT ( 'NONE',  ( 15.81416325002590817, -6.360572704314725101, 18.34798005862930736 ) ) ;
#5391 = ADVANCED_FACE ( 'NONE', ( #6780 ), #18959, .F. ) ;
#5392 = CARTESIAN_POINT ( 'NONE',  ( 3.221450758838616757, -1.621276839356792454, -1.500000000000000000 ) ) ;
#5393 = ORIENTED_EDGE ( 'NONE', *, *, #18135, .T. ) ;
#5394 = CARTESIAN_POINT ( 'NONE',  ( -23.21352257770656990, -10.78826658734919519, 45.15942333309109813 ) ) ;
#5395 = ADVANCED_FACE ( 'NONE', ( #4285 ), #9590, .F. ) ;
#5396 = VECTOR ( 'NONE', #27361, 1000.000000000000000 ) ;
#5397 = CARTESIAN_POINT ( 'NONE',  ( -40.00000000000002842, 80.00000000000001421, 52.50000000000014921 ) ) ;
#5398 = CYLINDRICAL_SURFACE ( 'NONE', #17825, 0.7499999999999988898 ) ;
#5399 = CARTESIAN_POINT ( 'NONE',  ( -36.21276101124586688, -16.00154621764524165, 34.83087659172860384 ) ) ;
#5400 = VERTEX_POINT ( 'NONE', #4744 ) ;
#5401 = EDGE_CURVE ( 'NONE', #13443, #24159, #26267, .T. ) ;
#5402 = DIRECTION ( 'NONE',  ( 0.000000000000000000, 0.000000000000000000, -1.000000000000000000 ) ) ;
#5403 = ADVANCED_FACE ( 'NONE', ( #13962 ), #16147, .F. ) ;
#5404 = CARTESIAN_POINT ( 'NONE',  ( 22.58267429318971864, 26.57182937991349903, 26.54355021145563143 ) ) ;
#5405 = AXIS2_PLACEMENT_3D ( 'NONE', #22034, #21886, #17518 ) ;
#5406 = CARTESIAN_POINT ( 'NONE',  ( 0.7083562926195156040, -9.056472324687613096, 21.50000000000000000 ) ) ;
#5407 = EDGE_LOOP ( 'NONE', ( #25318, #3596 ) ) ;
#5408 = FACE_OUTER_BOUND ( 'NONE', #13542, .T. ) ;
#5409 = FACE_OUTER_BOUND ( 'NONE', #25094, .T. ) ;
#5410 = CARTESIAN_POINT ( 'NONE',  ( 16.65122935894595813, 13.93942108199718888, -1.500000000000000000 ) ) ;
#5411 = CARTESIAN_POINT ( 'NONE',  ( -4.163336342344337027E-14, -1.387778780781445676E-14, 1.500000000000000000 ) ) ;
#5412 = DIRECTION ( 'NONE',  ( 0.000000000000000000, 0.000000000000000000, -1.000000000000000000 ) ) ;
#5413 = CARTESIAN_POINT ( 'NONE',  ( 0.000000000000000000, 0.000000000000000000, 1.500000000000001332 ) ) ;
#5414 = CARTESIAN_POINT ( 'NONE',  ( -3.000000000000041744, 1.387778780781445676E-14, 24.50000000000000000 ) ) ;
#5415 = CARTESIAN_POINT ( 'NONE',  ( -4.776122516674677878E-15, -42.50000000000000000, 32.33822642395377045 ) ) ;
#5416 = EDGE_LOOP ( 'NONE', ( #30246, #5071, #3786, #1010 ) ) ;
#5417 = EDGE_CURVE ( 'NONE', #25523, #28836, #28618, .T. ) ;
#5418 = CIRCLE ( 'NONE', #20780, 9.482273699623480212 ) ;
#5419 = CYLINDRICAL_SURFACE ( 'NONE', #22709, 9.482273699623480212 ) ;
#5420 = DIRECTION ( 'NONE',  ( 1.000000000000000000, 0.000000000000000000, 0.000000000000000000 ) ) ;
#5421 = AXIS2_PLACEMENT_3D ( 'NONE', #28656, #22083, #2922 ) ;
#5422 = ORIENTED_EDGE ( 'NONE', *, *, #25429, .F. ) ;
#5423 = VECTOR ( 'NONE', #3707, 1000.000000000000000 ) ;
#5424 = ORIENTED_EDGE ( 'NONE', *, *, #21388, .F. ) ;
#5425 = CARTESIAN_POINT ( 'NONE',  ( 6.899999999999999467, -5.196152422706639129, -9.000000000000000000 ) ) ;
#5426 = ADVANCED_FACE ( 'NONE', ( #25821 ), #1803, .F. ) ;
#5427 = CARTESIAN_POINT ( 'NONE',  ( -6.672226544319371122, 49.56122815818398664, -41.52977849429709067 ) ) ;
#5428 = EDGE_CURVE ( 'NONE', #7702, #4497, #29782, .T. ) ;
#5429 = ORIENTED_EDGE ( 'NONE', *, *, #18916, .T. ) ;
#5430 = AXIS2_PLACEMENT_3D ( 'NONE', #21476, #23969, #12600 ) ;
#5431 = CARTESIAN_POINT ( 'NONE',  ( 12.77540468287705444, 11.25967455357098679, 20.12545155307891065 ) ) ;
#5432 = CARTESIAN_POINT ( 'NONE',  ( -11.33306590618138543, -16.50086680533498296, 6.974106381145714018 ) ) ;
#5433 = ORIENTED_EDGE ( 'NONE', *, *, #5934, .F. ) ;
#5434 = CARTESIAN_POINT ( 'NONE',  ( 18.41033144393026078, -7.859752488074927435, 20.33971507717571114 ) ) ;
#5435 = VECTOR ( 'NONE', #14219, 1000.000000000000000 ) ;
#5436 = CYLINDRICAL_SURFACE ( 'NONE', #27723, 3.000000000000002665 ) ;
#5437 = CARTESIAN_POINT ( 'NONE',  ( 6.899999999999999467, 9.000000000000000000, 0.000000000000000000 ) ) ;
#5438 = VERTEX_POINT ( 'NONE', #30342 ) ;
#5439 = CARTESIAN_POINT ( 'NONE',  ( -6.187077094091591789, 11.47693674426096955, 1.500000000000001332 ) ) ;
#5440 = ORIENTED_EDGE ( 'NONE', *, *, #26578, .F. ) ;
#5441 = CARTESIAN_POINT ( 'NONE',  ( 14.91216081148350270, 35.95613889121786855, 27.50000000000000711 ) ) ;
#5442 = VECTOR ( 'NONE', #21116, 1000.000000000000000 ) ;
#5443 = ORIENTED_EDGE ( 'NONE', *, *, #20483, .F. ) ;
#5444 = CARTESIAN_POINT ( 'NONE',  ( 32.08353429544116864, -26.68014823150863890, -14.83332872412183789 ) ) ;
#5445 = CARTESIAN_POINT ( 'NONE',  ( -6.575147850411302564, 18.90724948634255753, 20.13759033520874908 ) ) ;
#5446 = CARTESIAN_POINT ( 'NONE',  ( -13.09005700315871579, 10.89973235955168107, 20.25336174263950184 ) ) ;
#5447 = VECTOR ( 'NONE', #30090, 1000.000000000000000 ) ;
#5448 = LINE ( 'NONE', #596, #11248 ) ;
#5449 = CARTESIAN_POINT ( 'NONE',  ( -38.16194395454053989, 8.856611044372645125, 31.97620825923344512 ) ) ;
#5450 = CARTESIAN_POINT ( 'NONE',  ( -5.976018955020170331, 19.08630078664910812, 5.652196082369963293 ) ) ;
#5451 = ORIENTED_EDGE ( 'NONE', *, *, #17497, .T. ) ;
#5452 = EDGE_CURVE ( 'NONE', #30374, #4497, #2098, .T. ) ;
#5453 = CARTESIAN_POINT ( 'NONE',  ( 10.92986663323816821, -16.77091174116444705, 5.670038381137163519 ) ) ;
#5454 = AXIS2_PLACEMENT_3D ( 'NONE', #8164, #27188, #15316 ) ;
#5455 = CARTESIAN_POINT ( 'NONE',  ( -28.29454325412426030, 29.24967321222531780, 14.73627230915420583 ) ) ;
#5456 = CARTESIAN_POINT ( 'NONE',  ( 19.86476987328767763, 2.322391784566621542, 6.144783687052517429 ) ) ;
#5457 = ORIENTED_EDGE ( 'NONE', *, *, #13187, .T. ) ;
#5458 = ORIENTED_EDGE ( 'NONE', *, *, #4112, .F. ) ;
#5459 = DIRECTION ( 'NONE',  ( 0.000000000000000000, -1.132880637372608986E-16, 1.000000000000000000 ) ) ;
#5460 = CARTESIAN_POINT ( 'NONE',  ( 10.25394813640221692, -17.17138746996171506, 6.781503518395080476 ) ) ;
#5461 = PRODUCT_DEFINITION_SHAPE ( 'NONE', 'NONE',  #30871 ) ;
#5462 = DIRECTION ( 'NONE',  ( 1.000000000000000000, 0.000000000000000000, 0.000000000000000000 ) ) ;
#5463 = CARTESIAN_POINT ( 'NONE',  ( 11.66432357650252349, 12.47412091822830149, 6.521906765011497242 ) ) ;
#5464 = DIRECTION ( 'NONE',  ( 1.000000000000000000, 0.000000000000000000, 0.000000000000000000 ) ) ;
#5465 = CARTESIAN_POINT ( 'NONE',  ( 6.139601762201234436, 19.03438667047814903, 6.144783687052517429 ) ) ;
#5466 = VERTEX_POINT ( 'NONE', #24392 ) ;
#5467 = CARTESIAN_POINT ( 'NONE',  ( -35.00000000000000000, 70.00000000000000000, 12.49999999999999112 ) ) ;
#5468 = CIRCLE ( 'NONE', #30382, 5.035999999999999588 ) ;
#5469 = CARTESIAN_POINT ( 'NONE',  ( 37.16608720827707657, -36.86186943028246787, 57.49999999999999289 ) ) ;
#5470 = CARTESIAN_POINT ( 'NONE',  ( 16.85411910731515306, 2.412525337365569733, 6.018569869498933578 ) ) ;
#5471 = ORIENTED_EDGE ( 'NONE', *, *, #13002, .F. ) ;
#5472 = CARTESIAN_POINT ( 'NONE',  ( 15.25711736267466812, 12.95927645368826298, 7.500898271101006820 ) ) ;
#5473 = ORIENTED_EDGE ( 'NONE', *, *, #4253, .T. ) ;
#5474 = CARTESIAN_POINT ( 'NONE',  ( 16.19384365167809392, -5.424445124423267650, 6.782048567692550378 ) ) ;
#5475 = CARTESIAN_POINT ( 'NONE',  ( 30.74201181684197337, -15.50830195949553314, 36.32560960729286847 ) ) ;
#5476 = AXIS2_PLACEMENT_3D ( 'NONE', #1515, #5719, #1356 ) ;
#5477 = DIRECTION ( 'NONE',  ( 1.000000000000000000, 0.000000000000000000, 0.000000000000000000 ) ) ;
#5478 = ORIENTED_EDGE ( 'NONE', *, *, #24996, .F. ) ;
#5479 = CYLINDRICAL_SURFACE ( 'NONE', #313, 1.447898107987198646 ) ;
#5480 = B_SPLINE_CURVE_WITH_KNOTS ( 'NONE', 3,
 ( #17009, #26530, #18631, #19508, #10002, #29020, #20943, #21997, #4435, #21845, #5007, #12182, #21679, #7358, #2822, #14667 ),
 .UNSPECIFIED., .F., .F.,
 ( 4, 2, 2, 2, 2, 2, 2, 4 ),
 ( 0.5000000000000000000, 0.6250000000000014433, 0.6875000000000021094, 0.7187500000000024425, 0.7500000000000028866, 0.8125000000000018874, 0.8750000000000008882, 1.000000000000000000 ),
 .UNSPECIFIED. ) ;
#5481 = CARTESIAN_POINT ( 'NONE',  ( 24.03057240117691862, 26.57182937991349903, -1.500000000000001332 ) ) ;
#5482 = DIRECTION ( 'NONE',  ( -0.000000000000000000, -0.000000000000000000, 1.000000000000000000 ) ) ;
#5483 = CARTESIAN_POINT ( 'NONE',  ( 0.000000000000000000, 0.000000000000000000, 1.500000000000000000 ) ) ;
#5484 = CARTESIAN_POINT ( 'NONE',  ( -29.61203839202723032, -15.40012917324033381, 37.38016955275590192 ) ) ;
#5485 = CARTESIAN_POINT ( 'NONE',  ( 9.326937650406419422, -14.24778824691897050, 20.12545155307891065 ) ) ;
#5486 = CARTESIAN_POINT ( 'NONE',  ( -4.375757216953428294E-15, -39.50000000000000000, 34.49999999999999289 ) ) ;
#5487 = VERTEX_POINT ( 'NONE', #26904 ) ;
#5488 = CARTESIAN_POINT ( 'NONE',  ( 24.58208797071834439, 7.298293523701641305, 49.35779847067223614 ) ) ;
#5489 = AXIS2_PLACEMENT_3D ( 'NONE', #311, #19351, #28406 ) ;
#5490 = CARTESIAN_POINT ( 'NONE',  ( -13.65791587866002388, 10.22062306005669541, 20.25542030744407640 ) ) ;
#5491 = CARTESIAN_POINT ( 'NONE',  ( 5.291486201320592997, 19.28729773841935469, 5.652196082369963293 ) ) ;
#5492 = VERTEX_POINT ( 'NONE', #12403 ) ;
#5493 = CARTESIAN_POINT ( 'NONE',  ( 32.52407683584942788, -23.45431533902839405, 17.97980913012589710 ) ) ;
#5494 = DIRECTION ( 'NONE',  ( 0.000000000000000000, -0.000000000000000000, -1.000000000000000000 ) ) ;
#5495 = CARTESIAN_POINT ( 'NONE',  ( -15.34618562042307843, 12.82554431217322310, 18.34798005863227388 ) ) ;
#5496 = SURFACE_SIDE_STYLE ('',( #20147 ) ) ;
#5497 = CARTESIAN_POINT ( 'NONE',  ( -5.374868878256215510, -44.10336124695545124, -19.50000000000000355 ) ) ;
#5498 = CARTESIAN_POINT ( 'NONE',  ( 0.000000000000000000, 0.000000000000000000, 12.49999999999999112 ) ) ;
#5499 = LINE ( 'NONE', #806, #9917 ) ;
#5500 = DIRECTION ( 'NONE',  ( -0.000000000000000000, 1.132880637372608986E-16, -1.000000000000000000 ) ) ;
#5501 = ORIENTED_EDGE ( 'NONE', *, *, #19304, .T. ) ;
#5502 = DIRECTION ( 'NONE',  ( -1.000000000000000000, 0.000000000000000000, 0.000000000000000000 ) ) ;
#5503 = CARTESIAN_POINT ( 'NONE',  ( -23.59115238065502851, -12.85789229732232997, 43.88988317752900770 ) ) ;
#5504 = ORIENTED_EDGE ( 'NONE', *, *, #29254, .T. ) ;
#5505 = EDGE_LOOP ( 'NONE', ( #7577, #18196, #6030, #2181 ) ) ;
#5506 = CYLINDRICAL_SURFACE ( 'NONE', #30209, 20.00000000000000000 ) ;
#5507 = VERTEX_POINT ( 'NONE', #12557 ) ;
#5508 = CIRCLE ( 'NONE', #4021, 0.7499999999999997780 ) ;
#5509 = VERTEX_POINT ( 'NONE', #28771 ) ;
#5510 = DIRECTION ( 'NONE',  ( -1.000000000000000000, 0.000000000000000000, 0.000000000000000000 ) ) ;
#5511 = CARTESIAN_POINT ( 'NONE',  ( -37.99999999999999289, 70.00000000000000000, -34.49999999999999289 ) ) ;
#5512 = CYLINDRICAL_SURFACE ( 'NONE', #19977, 2.000000000000001776 ) ;
#5513 = CARTESIAN_POINT ( 'NONE',  ( -9.436481611552759219, -0.9307681286968216838, 21.50000000000000000 ) ) ;
#5514 = DIRECTION ( 'NONE',  ( -0.000000000000000000, -0.000000000000000000, 1.000000000000000000 ) ) ;
#5515 = ORIENTED_EDGE ( 'NONE', *, *, #2170, .F. ) ;
#5516 = ADVANCED_FACE ( 'NONE', ( #17382 ), #17219, .F. ) ;
#5517 = CARTESIAN_POINT ( 'NONE',  ( -11.35972605147146020, -16.46076013017339434, 6.518927109361845496 ) ) ;
#5518 = DIRECTION ( 'NONE',  ( 1.000000000000000000, 0.000000000000000000, 0.000000000000000000 ) ) ;
#5519 = CYLINDRICAL_SURFACE ( 'NONE', #18222, 20.00000000000000355 ) ;
#5520 = DIRECTION ( 'NONE',  ( 0.000000000000000000, -1.132880637372608986E-16, 1.000000000000000000 ) ) ;
#5521 = ORIENTED_EDGE ( 'NONE', *, *, #26339, .T. ) ;
#5522 = CARTESIAN_POINT ( 'NONE',  ( -11.29739510359497423, -16.52539200402570785, 19.77662771831109367 ) ) ;
#5523 = CYLINDRICAL_SURFACE ( 'NONE', #9799, 0.7441270634457181066 ) ;
#5524 = CARTESIAN_POINT ( 'NONE',  ( -5.870757325077154754, 16.01346137069357667, 5.704143890883081269 ) ) ;
#5525 = CARTESIAN_POINT ( 'NONE',  ( 11.77505735701808121, -16.18809529858903318, 6.041646659195333058 ) ) ;
#5526 = EDGE_CURVE ( 'NONE', #17814, #5509, #842, .T. ) ;
#5527 = VECTOR ( 'NONE', #4856, 1000.000000000000000 ) ;
#5528 = CARTESIAN_POINT ( 'NONE',  ( 2.687479363073301819, 44.39187623479102740, -19.50000000000000355 ) ) ;
#5529 = VECTOR ( 'NONE', #19949, 1000.000000000000000 ) ;
#5530 = CARTESIAN_POINT ( 'NONE',  ( -57.50000000000001421, -50.00000000000000000, 97.07879600563551037 ) ) ;
#5531 = VERTEX_POINT ( 'NONE', #12235 ) ;
#5532 = ORIENTED_EDGE ( 'NONE', *, *, #22201, .F. ) ;
#5533 = FACE_OUTER_BOUND ( 'NONE', #22627, .T. ) ;
#5534 = CARTESIAN_POINT ( 'NONE',  ( -5.027435569059560905, 19.35787894679205934, 19.08232364404840098 ) ) ;
#5535 = CARTESIAN_POINT ( 'NONE',  ( 1.860660329155702231, -42.45830717661258547, 34.61210867867529828 ) ) ;
#5536 = CARTESIAN_POINT ( 'NONE',  ( 1.195154792889395079, 9.406652940105990623, 21.50000000000000000 ) ) ;
#5537 = ORIENTED_EDGE ( 'NONE', *, *, #8603, .F. ) ;
#5538 = APPLICATION_PROTOCOL_DEFINITION ( 'draft international standard', 'automotive_design', 1998, #8789 ) ;
#5539 = DIRECTION ( 'NONE',  ( 1.000000000000000000, 0.000000000000000000, 0.000000000000000000 ) ) ;
#5540 = EDGE_CURVE ( 'NONE', #4862, #26649, #11573, .T. ) ;
#5541 = ORIENTED_EDGE ( 'NONE', *, *, #1572, .T. ) ;
#5542 = CARTESIAN_POINT ( 'NONE',  ( 5.409330662328859063, 19.27307614344555020, 18.35377592296120497 ) ) ;
#5543 = DIRECTION ( 'NONE',  ( 0.000000000000000000, 0.000000000000000000, -1.000000000000000000 ) ) ;
#5544 = DIRECTION ( 'NONE',  ( -1.000000000000000000, 0.000000000000000000, 0.000000000000000000 ) ) ;
#5545 = CARTESIAN_POINT ( 'NONE',  ( -38.67597152258920801, -5.617507608258466512, 32.13009641412468653 ) ) ;
#5546 = EDGE_LOOP ( 'NONE', ( #24679, #8107 ) ) ;
#5547 = CARTESIAN_POINT ( 'NONE',  ( -9.248129367672078160, -2.094186647214714814, 13.00000000000000178 ) ) ;
#5548 = CARTESIAN_POINT ( 'NONE',  ( -13.93942108199721730, 16.65122935894503442, 1.500000000000000000 ) ) ;
#5549 = ADVANCED_FACE ( 'NONE', ( #12709 ), #11410, .T. ) ;
#5550 = AXIS2_PLACEMENT_3D ( 'NONE', #6274, #15786, #25308 ) ;
#5551 = FACE_BOUND ( 'NONE', #6686, .T. ) ;
#5552 = CARTESIAN_POINT ( 'NONE',  ( 39.99999999999998579, 80.00000000000001421, 17.49999999999999645 ) ) ;
#5553 = ORIENTED_EDGE ( 'NONE', *, *, #12219, .F. ) ;
#5554 = DIRECTION ( 'NONE',  ( -0.000000000000000000, -0.000000000000000000, -1.000000000000000000 ) ) ;
#5555 = CARTESIAN_POINT ( 'NONE',  ( 31.22486525274646496, 15.32888848509420221, 35.97296397489736108 ) ) ;
#5556 = ADVANCED_FACE ( 'NONE', ( #3338 ), #20487, .T. ) ;
#5557 = DIRECTION ( 'NONE',  ( -1.000000000000000000, 0.000000000000000000, 0.000000000000000000 ) ) ;
#5558 = EDGE_CURVE ( 'NONE', #29647, #18139, #22368, .T. ) ;
#5559 = DIRECTION ( 'NONE',  ( 0.000000000000000000, -1.000000000000000000, 0.000000000000000000 ) ) ;
#5560 = AXIS2_PLACEMENT_3D ( 'NONE', #1012, #19886, #8038 ) ;
#5561 = FACE_OUTER_BOUND ( 'NONE', #17940, .T. ) ;
#5562 = DIRECTION ( 'NONE',  ( -1.000000000000000000, 0.000000000000000000, 0.000000000000000000 ) ) ;
#5563 = CARTESIAN_POINT ( 'NONE',  ( -42.49999999999998579, -50.00000000000000000, 62.49999999999999289 ) ) ;
#5564 = EDGE_CURVE ( 'NONE', #25162, #2292, #1475, .T. ) ;
#5565 = FACE_OUTER_BOUND ( 'NONE', #8730, .T. ) ;
#5566 = EDGE_LOOP ( 'NONE', ( #17118, #10038, #16960, #17238 ) ) ;
#5567 = EDGE_CURVE ( 'NONE', #3020, #5531, #25324, .T. ) ;
#5568 = VECTOR ( 'NONE', #25236, 1000.000000000000000 ) ;
#5569 = CYLINDRICAL_SURFACE ( 'NONE', #7804, 20.00000000000000000 ) ;
#5570 = CARTESIAN_POINT ( 'NONE',  ( 5.163176754322195805, 19.32250783072323230, 5.652912763329821288 ) ) ;
#5571 = VERTEX_POINT ( 'NONE', #13326 ) ;
#5572 = ORIENTED_EDGE ( 'NONE', *, *, #4607, .F. ) ;
#5573 = EDGE_CURVE ( 'NONE', #752, #30725, #10663, .T. ) ;
#5574 = CARTESIAN_POINT ( 'NONE',  ( -8.074094344234884818E-15, 42.50000000000000000, 19.72227980406325543 ) ) ;
#5575 = EDGE_CURVE ( 'NONE', #2154, #2241, #27201, .T. ) ;
#5576 = CARTESIAN_POINT ( 'NONE',  ( -4.851473655640472948, 49.77239851816440108, -69.22750204485392089 ) ) ;
#5577 =( NAMED_UNIT ( * ) PLANE_ANGLE_UNIT ( ) SI_UNIT ( $, .RADIAN. ) );
#5578 = ORIENTED_EDGE ( 'NONE', *, *, #7927, .F. ) ;
#5579 = AXIS2_PLACEMENT_3D ( 'NONE', #4312, #13393, #13843 ) ;
#5580 = CARTESIAN_POINT ( 'NONE',  ( -33.67377525255856341, -13.97887046878493500, 27.50000000000000000 ) ) ;
#5581 = EDGE_CURVE ( 'NONE', #24520, #13253, #5097, .T. ) ;
#5582 = LINE ( 'NONE', #8080, #21121 ) ;
#5583 = EDGE_CURVE ( 'NONE', #8511, #15390, #8142, .T. ) ;
#5584 = ORIENTED_EDGE ( 'NONE', *, *, #16213, .T. ) ;
#5585 = DIRECTION ( 'NONE',  ( 0.000000000000000000, 0.000000000000000000, 1.000000000000000000 ) ) ;
#5586 = CARTESIAN_POINT ( 'NONE',  ( 0.9621688436939442868, 9.033033306777458193, 13.22130136205108997 ) ) ;
#5587 = CYLINDRICAL_SURFACE ( 'NONE', #1533, 0.7500000000000006661 ) ;
#5588 = EDGE_LOOP ( 'NONE', ( #24455, #3172, #6613, #24294 ) ) ;
#5589 = DIRECTION ( 'NONE',  ( 0.9096319953545183301, 0.4154150130018864906, 0.000000000000000000 ) ) ;
#5590 = VERTEX_POINT ( 'NONE', #5992 ) ;
#5591 = CIRCLE ( 'NONE', #26005, 6.000000000000001776 ) ;
#5592 = CARTESIAN_POINT ( 'NONE',  ( -16.93068695967834358, 1.913742347823925938, 20.32222155561919053 ) ) ;
#5593 = ORIENTED_EDGE ( 'NONE', *, *, #17182, .F. ) ;
#5594 = EDGE_CURVE ( 'NONE', #18416, #3499, #14805, .T. ) ;
#5595 = CARTESIAN_POINT ( 'NONE',  ( -6.453144054752233849, 18.93070788617553646, 20.22386025856690139 ) ) ;
#5596 = EDGE_CURVE ( 'NONE', #27593, #19541, #22658, .T. ) ;
#5597 = CARTESIAN_POINT ( 'NONE',  ( -6.414842543015754295, 17.06554576617236307, -1.500000000000000000 ) ) ;
#5598 = CARTESIAN_POINT ( 'NONE',  ( 16.57618148055193430, 4.095680178559270246, 7.098451512883313441 ) ) ;
#5599 = CARTESIAN_POINT ( 'NONE',  ( -5.141690706682821244, 7.488956955540452043, 21.50000000000000000 ) ) ;
#5600 = B_SPLINE_CURVE_WITH_KNOTS ( 'NONE', 3,
 ( #16648, #26154, #4781, #23805, #24576, #8065, #12126, #17570, #2608, #262, #19745, #14756, #15062, #22082, #5256, #7448, #21781, #2765, #7597, #4947, #19446, #26943, #24428, #12592, #21627, #28962, #26789, #19918, #24276, #12278, #3069, #3220, #24116, #19292, #29432, #9775, #14459, #28811, #23961, #21934, #22242, #7916, #16951, #716 ),
 .UNSPECIFIED., .F., .F.,
 ( 4, 2, 2, 2, 2, 2, 2, 2, 2, 2, 2, 2, 2, 2, 2, 2, 2, 2, 2, 2, 2, 4 ),
 ( 6.938893903907228378E-18, 0.003866689226559128639, 0.005800033839838692959, 0.007733378453118257279, 0.009666723066397821598, 0.01160006767967738592, 0.01256673998631717241, 0.01353341229295695718, 0.01401674844627684956, 0.01450008459959674367, 0.01498342075291663779, 0.01522508882957658398, 0.01546675690623653190, 0.01595009305955642429, 0.01643342921287630973, 0.01740010151951609102, 0.01836677382615587231, 0.01933344613279565360, 0.02126679074607521619, 0.02320013535935478224, 0.02706682458591391088, 0.03093351381247303605 ),
 .UNSPECIFIED. ) ;
#5601 = AXIS2_PLACEMENT_3D ( 'NONE', #13314, #4097, #3958 ) ;
#5602 = EDGE_CURVE ( 'NONE', #15417, #30269, #28429, .T. ) ;
#5603 = CARTESIAN_POINT ( 'NONE',  ( -8.416592248870401249, -14.82768166143396193, 18.35718225375110180 ) ) ;
#5604 = CARTESIAN_POINT ( 'NONE',  ( -12.64130592652783136, 40.29950990793869892, 29.03293690792085258 ) ) ;
#5605 = DIRECTION ( 'NONE',  ( -0.000000000000000000, -0.000000000000000000, -1.000000000000000000 ) ) ;
#5606 = CARTESIAN_POINT ( 'NONE',  ( 14.83584055149749759, 17.84153987719500734, -1.500000000000000000 ) ) ;
#5607 = ORIENTED_EDGE ( 'NONE', *, *, #19301, .F. ) ;
#5608 = CARTESIAN_POINT ( 'NONE',  ( 10.83635815962788307, -16.83143582838889074, 5.701226463332907279 ) ) ;
#5609 = CARTESIAN_POINT ( 'NONE',  ( 34.45795948451156221, -11.47936083950614794, 34.50000000000000000 ) ) ;
#5610 = DIRECTION ( 'NONE',  ( 0.000000000000000000, 0.000000000000000000, 1.000000000000000000 ) ) ;
#5611 = EDGE_LOOP ( 'NONE', ( #13562, #25775, #26393, #14237 ) ) ;
#5612 = ORIENTED_EDGE ( 'NONE', *, *, #865, .T. ) ;
#5613 = APPLICATION_CONTEXT ( 'automotive_design' ) ;
#5614 = CARTESIAN_POINT ( 'NONE',  ( 4.340342926364955112, 8.430595340551274575, 21.50000000000000000 ) ) ;
#5615 = AXIS2_PLACEMENT_3D ( 'NONE', #22980, #20643, #8796 ) ;
#5616 = CARTESIAN_POINT ( 'NONE',  ( 11.10715495309692891, -16.63223102436628409, 7.652108011868850035 ) ) ;
#5617 = EDGE_CURVE ( 'NONE', #27291, #8486, #6075, .T. ) ;
#5618 = AXIS2_PLACEMENT_3D ( 'NONE', #11663, #9171, #18683 ) ;
#5619 = DIRECTION ( 'NONE',  ( -1.000000000000000000, 0.000000000000000000, 0.000000000000000000 ) ) ;
#5620 = ORIENTED_EDGE ( 'NONE', *, *, #10768, .T. ) ;
#5621 = DIRECTION ( 'NONE',  ( 0.000000000000000000, 0.000000000000000000, 1.000000000000000000 ) ) ;
#5622 = CARTESIAN_POINT ( 'NONE',  ( -5.349779314757643789, -7.341751895053219457, 21.50000000000000000 ) ) ;
#5623 = CARTESIAN_POINT ( 'NONE',  ( 5.783356563690326801, 19.14595685992715346, 7.526993102356318133 ) ) ;
#5624 = ORIENTED_EDGE ( 'NONE', *, *, #15656, .F. ) ;
#5625 = CARTESIAN_POINT ( 'NONE',  ( 69.99999999999998579, 70.00000000000000000, -92.50000000000000000 ) ) ;
#5626 = FACE_OUTER_BOUND ( 'NONE', #15609, .T. ) ;
#5627 = CARTESIAN_POINT ( 'NONE',  ( -50.00000000000000000, -70.00000000000000000, -92.50000000000000000 ) ) ;
#5628 = ORIENTED_EDGE ( 'NONE', *, *, #27520, .F. ) ;
#5629 = CARTESIAN_POINT ( 'NONE',  ( 23.17581250239729940, 34.50630206824671831, 1.499999999999999778 ) ) ;
#5630 = ORIENTED_EDGE ( 'NONE', *, *, #17536, .T. ) ;
#5631 = ADVANCED_FACE ( 'NONE', ( #11585 ), #25486, .F. ) ;
#5632 = CARTESIAN_POINT ( 'NONE',  ( 19.18576292979354392, -22.55620591602728453, 1.500000000000001332 ) ) ;
#5633 = ADVANCED_FACE ( 'NONE', ( #11735 ), #30758, .T. ) ;
#5634 = CARTESIAN_POINT ( 'NONE',  ( 31.79271162922634630, -14.90794587988476927, 35.64318943584540733 ) ) ;
#5635 = ORIENTED_EDGE ( 'NONE', *, *, #429, .T. ) ;
#5636 = DIRECTION ( 'NONE',  ( 0.000000000000000000, 0.000000000000000000, 1.000000000000000000 ) ) ;
#5637 = VECTOR ( 'NONE', #10990, 1000.000000000000000 ) ;
#5638 = FACE_OUTER_BOUND ( 'NONE', #5125, .T. ) ;
#5639 = DIRECTION ( 'NONE',  ( 0.000000000000000000, 0.000000000000000000, 1.000000000000000000 ) ) ;
#5640 = CARTESIAN_POINT ( 'NONE',  ( 23.05503963851395000, 30.35185526021188807, 34.49999999999999289 ) ) ;
#5641 = CARTESIAN_POINT ( 'NONE',  ( -31.29501345865529061, -26.27841684422010360, -6.500000000000000888 ) ) ;
#5642 = CARTESIAN_POINT ( 'NONE',  ( 10.65605551513794680, -16.94611923951457300, 20.19668224736330941 ) ) ;
#5643 = CARTESIAN_POINT ( 'NONE',  ( 10.36464550818150876, -17.10487384371581143, 18.84056766331482180 ) ) ;
#5644 = ORIENTED_EDGE ( 'NONE', *, *, #23523, .T. ) ;
#5645 = CARTESIAN_POINT ( 'NONE',  ( -24.50428919468314248, -7.442132857256927636, 49.39104690844366274 ) ) ;
#5646 = CARTESIAN_POINT ( 'NONE',  ( -15.98601489809225740, 12.04791232832106118, 19.47783254395485031 ) ) ;
#5647 = CARTESIAN_POINT ( 'NONE',  ( 23.62400240902267967, -9.724154461249520764, 49.47829057475696146 ) ) ;
#5648 = ORIENTED_EDGE ( 'NONE', *, *, #20619, .F. ) ;
#5649 = CARTESIAN_POINT ( 'NONE',  ( 9.675133109038689838, -8.168544852422947145, 1.500000000000000000 ) ) ;
#5650 = DIRECTION ( 'NONE',  ( -0.000000000000000000, -0.000000000000000000, -1.000000000000000000 ) ) ;
#5651 = B_SPLINE_SURFACE_WITH_KNOTS ( 'NONE', 3, 1, ( 
 ( #6319, #25350 ),
 ( #3988, #13511 ),
 ( #4131, #21574 ),
 ( #2240, #7399 ),
 ( #2565, #2406 ),
 ( #2716, #30622 ),
 ( #211, #24065 ),
 ( #18950, #19234 ),
 ( #9268, #23448 ),
 ( #7085, #28760 ),
 ( #9724, #18789 ),
 ( #12224, #25811 ),
 ( #16909, #11933 ),
 ( #9434, #21724 ),
 ( #28459, #16590 ),
 ( #26105, #26425 ),
 ( #66, #6935 ),
 ( #5054, #364 ),
 ( #4735, #21103 ),
 ( #14236, #2086 ),
 ( #9885, #28310 ),
 ( #11608, #4897 ),
 ( #19402, #11759 ),
 ( #28920, #7553 ),
 ( #4442, #13953 ),
 ( #16445, #25959 ),
 ( #21424, #9579 ),
 ( #23918, #14416 ),
 ( #4587, #14087 ),
 ( #23597, #21257 ),
 ( #30785, #19090 ) ),
 .UNSPECIFIED., .F., .F., .F.,
 ( 4, 3, 3, 3, 3, 3, 3, 3, 3, 3, 4 ),
 ( 2, 2 ),
 ( 0.4999999998345686647, 0.5360336730431939367, 0.5907651151589012883, 0.6456034593241830599, 0.6998270958050434309, 0.7529536536315937223, 0.8052385063053260073, 0.8575343587103997356, 0.9106564858195042023, 0.9648414833209685293, 1.000000006602610014 ),
 ( 0.000000000000000000, 1.000000000000000000 ),
 .UNSPECIFIED. ) ;
#5652 = CARTESIAN_POINT ( 'NONE',  ( -15.34307810681595186, 12.82926163924265950, 20.34789198813115263 ) ) ;
#5653 = CARTESIAN_POINT ( 'NONE',  ( -34.07766914599908148, -21.40380666528021081, -1.500000000000000000 ) ) ;
#5654 = FACE_OUTER_BOUND ( 'NONE', #7086, .T. ) ;
#5655 = CARTESIAN_POINT ( 'NONE',  ( 14.14241404620503317, 39.63505646587483255, 34.54980534962761141 ) ) ;
#5656 = AXIS2_PLACEMENT_3D ( 'NONE', #28237, #2188, #6867 ) ;
#5657 = ORIENTED_EDGE ( 'NONE', *, *, #10940, .T. ) ;
#5658 = DIRECTION ( 'NONE',  ( 0.000000000000000000, -1.000000000000000000, -1.132880637372608986E-16 ) ) ;
#5659 = CARTESIAN_POINT ( 'NONE',  ( 14.88222593340887023, 13.36111339922579866, 20.34789198813115263 ) ) ;
#5660 = FACE_OUTER_BOUND ( 'NONE', #19726, .T. ) ;
#5661 = ORIENTED_EDGE ( 'NONE', *, *, #23269, .T. ) ;
#5662 = ORIENTED_EDGE ( 'NONE', *, *, #22148, .T. ) ;
#5663 = DIRECTION ( 'NONE',  ( 1.000000000000000000, 0.000000000000000000, -1.369518533665900065E-16 ) ) ;
#5664 = ORIENTED_EDGE ( 'NONE', *, *, #20517, .T. ) ;
#5665 = DIRECTION ( 'NONE',  ( -1.000000000000000000, 0.000000000000000000, 0.000000000000000000 ) ) ;
#5666 = EDGE_CURVE ( 'NONE', #2660, #18536, #23572, .T. ) ;
#5667 = LINE ( 'NONE', #8167, #21228 ) ;
#5668 = DIRECTION ( 'NONE',  ( 0.000000000000000000, 0.000000000000000000, 1.000000000000000000 ) ) ;
#5669 = AXIS2_PLACEMENT_3D ( 'NONE', #742, #3245, #15094 ) ;
#5670 = CARTESIAN_POINT ( 'NONE',  ( -4.390207617113899730, 7.856594496258241023, -1.500000000000000888 ) ) ;
#5671 = CARTESIAN_POINT ( 'NONE',  ( -20.48466473087059470, 26.10042409808303887, -16.50001200000000168 ) ) ;
#5672 = AXIS2_PLACEMENT_3D ( 'NONE', #22092, #25526, #18359 ) ;
#5673 = DIRECTION ( 'NONE',  ( 0.000000000000000000, 0.000000000000000000, -1.000000000000000000 ) ) ;
#5674 = FACE_OUTER_BOUND ( 'NONE', #21417, .T. ) ;
#5675 = CYLINDRICAL_SURFACE ( 'NONE', #17626, 0.7500000000000006661 ) ;
#5676 = ORIENTED_EDGE ( 'NONE', *, *, #2539, .T. ) ;
#5677 = AXIS2_PLACEMENT_3D ( 'NONE', #18237, #27758, #4040 ) ;
#5678 = CARTESIAN_POINT ( 'NONE',  ( -14.84326473672823887, -8.425446036094902169, 7.366751648393900176 ) ) ;
#5679 = CARTESIAN_POINT ( 'NONE',  ( -5.062693764981381683, 16.26276758967398095, 5.774779864094945481 ) ) ;
#5680 = CARTESIAN_POINT ( 'NONE',  ( 11.70583205457081810, -16.23839729645239416, 7.366751648393900176 ) ) ;
#5681 = CARTESIAN_POINT ( 'NONE',  ( -10.64374042650306862, 42.96126232887723972, -19.50000000000000355 ) ) ;
#5682 = CARTESIAN_POINT ( 'NONE',  ( 33.51208342369034199, -9.877893692955343141, 35.81995677910244780 ) ) ;
#5683 = ORIENTED_EDGE ( 'NONE', *, *, #15859, .T. ) ;
#5684 = ORIENTED_EDGE ( 'NONE', *, *, #19878, .F. ) ;
#5685 = DIRECTION ( 'NONE',  ( -0.4495526574063634095, 0.8932538319083086487, 0.000000000000000000 ) ) ;
#5686 = CARTESIAN_POINT ( 'NONE',  ( -12.56641067637617759, -40.32935944494947478, -1.500000000000000000 ) ) ;
#5687 = CARTESIAN_POINT ( 'NONE',  ( -15.33339156390900371, 12.86857621502489479, 5.651989602109218858 ) ) ;
#5688 = DIRECTION ( 'NONE',  ( 0.000000000000000000, -0.000000000000000000, 1.000000000000000000 ) ) ;
#5689 = ORIENTED_EDGE ( 'NONE', *, *, #25026, .F. ) ;
#5690 = CONTEXT_DEPENDENT_SHAPE_REPRESENTATION ( #11988, #12168 ) ;
#5691 = CARTESIAN_POINT ( 'NONE',  ( 3.062271323958281499, 16.80150817659524520, 6.783738457429056012 ) ) ;
#5692 = DIRECTION ( 'NONE',  ( 1.000000000000000000, 0.000000000000000000, 0.000000000000000000 ) ) ;
#5693 = VECTOR ( 'NONE', #18548, 1000.000000000000000 ) ;
#5694 = EDGE_LOOP ( 'NONE', ( #6793, #18652, #23579, #22900, #7663 ) ) ;
#5695 = FACE_OUTER_BOUND ( 'NONE', #2785, .T. ) ;
#5696 = DIRECTION ( 'NONE',  ( 1.000000000000000000, 0.000000000000000000, 0.000000000000000000 ) ) ;
#5697 = CARTESIAN_POINT ( 'NONE',  ( -25.50709904238008008, -27.59382699987884280, 37.50000000002468425 ) ) ;
#5698 = VERTEX_POINT ( 'NONE', #1917 ) ;
#5699 = DIRECTION ( 'NONE',  ( 0.000000000000000000, -1.132880637372608986E-16, 1.000000000000000000 ) ) ;
#5700 = ADVANCED_FACE ( 'NONE', ( #20778 ), #6748, .F. ) ;
#5701 = CARTESIAN_POINT ( 'NONE',  ( -38.00000000000000000, 65.00000000000000000, 15.49999999999998579 ) ) ;
#5702 = LINE ( 'NONE', #15196, #4864 ) ;
#5703 = ORIENTED_EDGE ( 'NONE', *, *, #12646, .F. ) ;
#5704 = CARTESIAN_POINT ( 'NONE',  ( -18.09182123201595971, -8.567353834808582036, 5.653912893140659257 ) ) ;
#5705 = CARTESIAN_POINT ( 'NONE',  ( 32.19782014694307293, 14.25394737442116444, 35.54550565580007770 ) ) ;
#5706 = CARTESIAN_POINT ( 'NONE',  ( 15.91946090795792657, -6.118695898272386025, 5.653604225791664106 ) ) ;
#5708 = B_SPLINE_CURVE_WITH_KNOTS ( 'NONE', 3,
 ( #30219, #15878, #18673, #20853, #4485, #18835, #20693, #6977, #1988, #4633, #18385, #16488, #6517, #26004 ),
 .UNSPECIFIED., .F., .F.,
 ( 4, 2, 2, 2, 2, 2, 4 ),
 ( 2.108610145906054180E-07, 0.0004867403503157751322, 0.0009732698396169596391, 0.001459799328918144146, 0.001946328818219328653, 0.002919387796821705256, 0.003892446775424082076 ),
 .UNSPECIFIED. ) ;
#5707 = DIRECTION ( 'NONE',  ( 0.000000000000000000, -1.132880637372608986E-16, 1.000000000000000000 ) ) ;
#5709 = CARTESIAN_POINT ( 'NONE',  ( -40.56315269328749196, 1.166124675481670092, -16.50000000000000000 ) ) ;
#5710 = CARTESIAN_POINT ( 'NONE',  ( 0.000000000000000000, 0.000000000000000000, 1.500000000000001332 ) ) ;
#5711 = CIRCLE ( 'NONE', #14674, 5.000000000000004441 ) ;
#5712 = FACE_OUTER_BOUND ( 'NONE', #24372, .T. ) ;
#5713 = DIRECTION ( 'NONE',  ( 1.000000000000000000, 0.000000000000000000, 0.000000000000000000 ) ) ;
#5714 = ORIENTED_EDGE ( 'NONE', *, *, #23526, .T. ) ;
#5715 = LINE ( 'NONE', #15208, #8306 ) ;
#5716 = DIRECTION ( 'NONE',  ( 1.000000000000000000, 0.000000000000000000, 0.000000000000000000 ) ) ;
#5717 = ORIENTED_EDGE ( 'NONE', *, *, #16017, .F. ) ;
#5718 = ORIENTED_EDGE ( 'NONE', *, *, #1153, .T. ) ;
#5719 = DIRECTION ( 'NONE',  ( 0.000000000000000000, 0.000000000000000000, -1.000000000000000000 ) ) ;
#5720 = CARTESIAN_POINT ( 'NONE',  ( 24.03057240117690441, -26.57182937991349903, 26.54355021145562787 ) ) ;
#5721 = CARTESIAN_POINT ( 'NONE',  ( 0.3563104543936347901, 6.049278984716042196, 7.522341449313135975 ) ) ;
#5722 = CARTESIAN_POINT ( 'NONE',  ( -15.48249060714018199, -35.68301910287905088, 27.50000000000000355 ) ) ;
#5723 = CARTESIAN_POINT ( 'NONE',  ( 12.50580948684386051, 11.57370347876661221, 18.36582235739946611 ) ) ;
#5724 = ADVANCED_FACE ( 'NONE', ( #21227 ), #2374, .F. ) ;
#5725 = VERTEX_POINT ( 'NONE', #25929 ) ;
#5726 = ORIENTED_EDGE ( 'NONE', *, *, #9575, .T. ) ;
#5727 = EDGE_CURVE ( 'NONE', #27254, #27382, #23492, .T. ) ;
#5728 = DIRECTION ( 'NONE',  ( 0.4539545692076743522, -0.8910248307962438385, 0.000000000000000000 ) ) ;
#5729 = CARTESIAN_POINT ( 'NONE',  ( 17.92197892105642154, -8.877232523309842804, 6.386539667786092167 ) ) ;
#5730 = ADVANCED_FACE ( 'NONE', ( #30600 ), #27828, .F. ) ;
#5731 = CARTESIAN_POINT ( 'NONE',  ( -16.69721919944057831, 13.88429941593312122, 1.500000000000000000 ) ) ;
#5732 = ORIENTED_EDGE ( 'NONE', *, *, #5782, .T. ) ;
#5733 = DIRECTION ( 'NONE',  ( -0.000000000000000000, -1.000000000000000000, -0.000000000000000000 ) ) ;
#5734 = CIRCLE ( 'NONE', #17196, 9.482273699623480212 ) ;
#5735 = ADVANCED_FACE ( 'NONE', ( #16114 ), #15966, .F. ) ;
#5736 = ORIENTED_EDGE ( 'NONE', *, *, #12838, .T. ) ;
#5737 = ADVANCED_FACE ( 'NONE', ( #21078 ), #9242, .F. ) ;
#5738 = CARTESIAN_POINT ( 'NONE',  ( -16.83599852035921884, 2.522587596188540449, 18.83976166372255534 ) ) ;
#5739 = EDGE_LOOP ( 'NONE', ( #26528, #21334, #18292, #19438 ) ) ;
#5740 = CARTESIAN_POINT ( 'NONE',  ( -6.934930584103120133, 18.75917743548997763, 19.21940439362674269 ) ) ;
#5741 = EDGE_CURVE ( 'NONE', #13876, #3241, #23121, .T. ) ;
#5742 = CARTESIAN_POINT ( 'NONE',  ( 31.70481081259145384, -24.75827009233382725, 30.59596842323437116 ) ) ;
#5743 = CARTESIAN_POINT ( 'NONE',  ( 19.65054205152827649, 3.817440173033142425, 7.441806358946449151 ) ) ;
#5744 = CARTESIAN_POINT ( 'NONE',  ( 42.49999999999998579, -50.00000000000000000, 97.07879600563551037 ) ) ;
#5745 = EDGE_CURVE ( 'NONE', #16359, #25738, #8953, .T. ) ;
#5746 = CARTESIAN_POINT ( 'NONE',  ( -9.668922248712513934, -17.52764785324847452, 19.58863275299554019 ) ) ;
#5747 = ADVANCED_FACE ( 'NONE', ( #25636 ), #4251, .F. ) ;
#5748 = CARTESIAN_POINT ( 'NONE',  ( -28.23311950821117122, 29.32737283093239711, 30.11920113326423376 ) ) ;
#5749 = DIRECTION ( 'NONE',  ( 1.000000000000000000, 0.000000000000000000, 0.000000000000000000 ) ) ;
#5750 = LINE ( 'NONE', #1392, #14847 ) ;
#5751 = VERTEX_POINT ( 'NONE', #13096 ) ;
#5752 = CARTESIAN_POINT ( 'NONE',  ( 10.51735345234056851, -17.03234025559531162, 5.940635272151477686 ) ) ;
#5753 = CARTESIAN_POINT ( 'NONE',  ( -8.817355867515827228, -2.185336383880175593, -1.500000000000001998 ) ) ;
#5754 = DIRECTION ( 'NONE',  ( 1.000000000000000000, 0.000000000000000000, -0.000000000000000000 ) ) ;
#5755 = VERTEX_POINT ( 'NONE', #5024 ) ;
#5756 = VERTEX_POINT ( 'NONE', #22590 ) ;
#5757 = B_SPLINE_CURVE_WITH_KNOTS ( 'NONE', 3,
 ( #6881, #30736, #18901, #8935, #28107, #19045 ),
 .UNSPECIFIED., .F., .F.,
 ( 4, 2, 4 ),
 ( 0.1293062580255212313, 0.1318912024619483814, 0.1344761468983755315 ),
 .UNSPECIFIED. ) ;
#5758 = CIRCLE ( 'NONE', #29174, 1.447898107987198646 ) ;
#5759 = DIRECTION ( 'NONE',  ( 0.000000000000000000, 0.000000000000000000, -1.000000000000000000 ) ) ;
#5760 = CARTESIAN_POINT ( 'NONE',  ( 43.34097750826426676, -11.89502811014148698, -1.500000000000000444 ) ) ;
#5761 = DIRECTION ( 'NONE',  ( -0.000000000000000000, -0.000000000000000000, -1.000000000000000000 ) ) ;
#5762 = ORIENTED_EDGE ( 'NONE', *, *, #20655, .F. ) ;
#5763 = CARTESIAN_POINT ( 'NONE',  ( -33.42925964089140933, 11.06161099612212695, 39.78814634291943264 ) ) ;
#5764 = EDGE_CURVE ( 'NONE', #10221, #20799, #24035, .T. ) ;
#5765 = EDGE_CURVE ( 'NONE', #29085, #3383, #9699, .T. ) ;
#5766 = LINE ( 'NONE', #7970, #2959 ) ;
#5767 = ORIENTED_EDGE ( 'NONE', *, *, #3632, .T. ) ;
#5768 = EDGE_CURVE ( 'NONE', #16514, #281, #5591, .T. ) ;
#5769 = ADVANCED_FACE ( 'NONE', ( #19208 ), #12944, .T. ) ;
#5770 = CARTESIAN_POINT ( 'NONE',  ( -10.28466407052217235, -17.15343732189304404, 18.37545668562167478 ) ) ;
#5771 = DIRECTION ( 'NONE',  ( -0.000000000000000000, -0.000000000000000000, 1.000000000000000000 ) ) ;
#5772 = CARTESIAN_POINT ( 'NONE',  ( 19.77948086832033425, 3.081792779576176589, 7.652108011868850035 ) ) ;
#5773 = ORIENTED_EDGE ( 'NONE', *, *, #23301, .T. ) ;
#5774 = CARTESIAN_POINT ( 'NONE',  ( 14.99999999999995737, 1.387778780781445676E-14, 92.49999999999998579 ) ) ;
#5775 = VERTEX_POINT ( 'NONE', #24937 ) ;
#5776 = DIRECTION ( 'NONE',  ( 0.000000000000000000, 0.000000000000000000, -1.000000000000000000 ) ) ;
#5777 = EDGE_CURVE ( 'NONE', #28158, #23071, #9569, .T. ) ;
#5778 = DIRECTION ( 'NONE',  ( 0.7416830501633135952, -0.6707505147970024284, 0.000000000000000000 ) ) ;
#5779 = ORIENTED_EDGE ( 'NONE', *, *, #2346, .T. ) ;
#5780 = EDGE_CURVE ( 'NONE', #12085, #477, #29622, .T. ) ;
#5781 = CIRCLE ( 'NONE', #14220, 2.898871837527149609 ) ;
#5782 = EDGE_CURVE ( 'NONE', #14763, #13104, #27016, .T. ) ;
#5783 = CARTESIAN_POINT ( 'NONE',  ( 4.606472074292932817, 19.48056636435423528, 7.366751648393900176 ) ) ;
#5784 = DIRECTION ( 'NONE',  ( 0.000000000000000000, 1.000000000000000000, 0.000000000000000000 ) ) ;
#5785 = CARTESIAN_POINT ( 'NONE',  ( 5.422617586916729238, 19.25129646183502174, 20.34789198813115618 ) ) ;
#5786 = CARTESIAN_POINT ( 'NONE',  ( 33.53348741818256684, 14.37470038618140933, 34.49999999999998579 ) ) ;
#5787 = CIRCLE ( 'NONE', #12758, 7.500000000000007105 ) ;
#5788 = FACE_OUTER_BOUND ( 'NONE', #23786, .T. ) ;
#5789 = CARTESIAN_POINT ( 'NONE',  ( 10.26788185420488375, -17.18392197670719312, 19.22654678686458141 ) ) ;
#5790 = CARTESIAN_POINT ( 'NONE',  ( 30.50204315964897717, 15.53056155674291539, 40.77182279853379754 ) ) ;
#5791 = VERTEX_POINT ( 'NONE', #10441 ) ;
#5792 = CARTESIAN_POINT ( 'NONE',  ( 25.18096005886327760, 6.640581704039639988, 48.95928115109020240 ) ) ;
#5793 = CARTESIAN_POINT ( 'NONE',  ( -13.91614452448632555, 9.890357823660679060, 19.89182036555910571 ) ) ;
#5794 = CIRCLE ( 'NONE', #27214, 36.25735931288072322 ) ;
#5795 = DIRECTION ( 'NONE',  ( 0.000000000000000000, -0.000000000000000000, -1.000000000000000000 ) ) ;
#5796 = DIRECTION ( 'NONE',  ( 1.000000000000000000, 0.000000000000000000, 0.000000000000000000 ) ) ;
#5797 = ORIENTED_EDGE ( 'NONE', *, *, #15767, .T. ) ;
#5798 = CARTESIAN_POINT ( 'NONE',  ( 2.185336383880204014, -8.817355867515821899, 21.50000000000000000 ) ) ;
#5799 = VECTOR ( 'NONE', #17977, 1000.000000000000000 ) ;
#5800 = DIRECTION ( 'NONE',  ( -1.000000000000000000, 0.000000000000000000, 0.000000000000000000 ) ) ;
#5801 = EDGE_CURVE ( 'NONE', #5466, #21772, #19060, .T. ) ;
#5802 = CARTESIAN_POINT ( 'NONE',  ( -15.25895845836713072, 12.92986402562787696, 20.34789198813115618 ) ) ;
#5803 = DIRECTION ( 'NONE',  ( -1.000000000000000000, 0.000000000000000000, 0.000000000000000000 ) ) ;
#5804 = ADVANCED_FACE ( 'NONE', ( #24777 ), #21543, .T. ) ;
#5805 = DIRECTION ( 'NONE',  ( 0.000000000000000000, 0.000000000000000000, 1.000000000000000000 ) ) ;
#5806 = CARTESIAN_POINT ( 'NONE',  ( -7.827050521741844236, 5.352643706120543854, 13.00000000000000178 ) ) ;
#5807 = AXIS2_PLACEMENT_3D ( 'NONE', #3152, #24976, #19836 ) ;
#5808 = CARTESIAN_POINT ( 'NONE',  ( 16.86493654370565665, 2.320966539639655490, 7.156916968540300239 ) ) ;
#5809 = ORIENTED_EDGE ( 'NONE', *, *, #6087, .T. ) ;
#5810 = VECTOR ( 'NONE', #13804, 1000.000000000000000 ) ;
#5811 = AXIS2_PLACEMENT_3D ( 'NONE', #13385, #6354, #8697 ) ;
#5812 = CARTESIAN_POINT ( 'NONE',  ( 24.58208797071834439, 7.298293523701643082, 45.11515778355294515 ) ) ;
#5813 = DIRECTION ( 'NONE',  ( 0.000000000000000000, 0.000000000000000000, -1.000000000000000000 ) ) ;
#5814 = CARTESIAN_POINT ( 'NONE',  ( 0.000000000000000000, 0.000000000000000000, -87.50000000000000000 ) ) ;
#5815 = ORIENTED_EDGE ( 'NONE', *, *, #24003, .F. ) ;
#5816 = ORIENTED_EDGE ( 'NONE', *, *, #27689, .F. ) ;
#5817 = CYLINDRICAL_SURFACE ( 'NONE', #7460, 15.00000000000000000 ) ;
#5818 = CIRCLE ( 'NONE', #15257, 0.7500000000000006661 ) ;
#5819 = EDGE_LOOP ( 'NONE', ( #7696, #14472 ) ) ;
#5820 = FACE_OUTER_BOUND ( 'NONE', #7033, .T. ) ;
#5821 = MECHANICAL_DESIGN_GEOMETRIC_PRESENTATION_REPRESENTATION (  '', ( #18749 ), #19698 ) ;
#5822 = CARTESIAN_POINT ( 'NONE',  ( 14.22989400835912832, 47.93398237600714396, -59.84665844486981001 ) ) ;
#5823 = CYLINDRICAL_SURFACE ( 'NONE', #29449, 0.7499999999999997780 ) ;
#5824 = CARTESIAN_POINT ( 'NONE',  ( -33.62358953728911359, 21.54311338121501507, 8.031451707336353607 ) ) ;
#5825 = AXIS2_PLACEMENT_3D ( 'NONE', #23624, #94, #9755 ) ;
#5826 = DIRECTION ( 'NONE',  ( -0.000000000000000000, -0.000000000000000000, -1.000000000000000000 ) ) ;
#5827 = AXIS2_PLACEMENT_3D ( 'NONE', #24997, #18294, #15956 ) ;
#5828 = CARTESIAN_POINT ( 'NONE',  ( -8.549050687778191104, -4.102102735472429096, 13.00000000000000178 ) ) ;
#5829 = LINE ( 'NONE', #833, #8130 ) ;
#5830 = CARTESIAN_POINT ( 'NONE',  ( 8.159193615868398197, -3.993622308618910210, -1.500000000000002220 ) ) ;
#5831 = DIRECTION ( 'NONE',  ( -0.000000000000000000, -0.000000000000000000, 1.000000000000000000 ) ) ;
#5832 = ORIENTED_EDGE ( 'NONE', *, *, #19927, .T. ) ;
#5833 = AXIS2_PLACEMENT_3D ( 'NONE', #26308, #4944, #9771 ) ;
#5834 = AXIS2_PLACEMENT_3D ( 'NONE', #21080, #25487, #25637 ) ;
#5835 = CARTESIAN_POINT ( 'NONE',  ( -8.744978663125428042, -14.62407600317563272, 20.32842677360128292 ) ) ;
#5836 = CARTESIAN_POINT ( 'NONE',  ( 16.52525247487311333, -14.36006998371588317, 1.500000000000000000 ) ) ;
#5837 = CARTESIAN_POINT ( 'NONE',  ( -17.75446986341067301, 9.207540381081360081, 24.50000000000000000 ) ) ;
#5838 = CARTESIAN_POINT ( 'NONE',  ( 11.76322808224952254, -16.19669642467957615, 7.280727868105637768 ) ) ;
#5839 = EDGE_CURVE ( 'NONE', #4843, #18506, #27282, .T. ) ;
#5840 = CARTESIAN_POINT ( 'NONE',  ( 39.83602371822922095, -11.57901747687539640, -19.50000000000000355 ) ) ;
#5841 = DIRECTION ( 'NONE',  ( -0.000000000000000000, 1.000000000000000000, -0.000000000000000000 ) ) ;
#5842 = VECTOR ( 'NONE', #14495, 1000.000000000000000 ) ;
#5843 = EDGE_LOOP ( 'NONE', ( #43, #18790, #29373, #22465 ) ) ;
#5844 = ORIENTED_EDGE ( 'NONE', *, *, #29402, .T. ) ;
#5845 = CARTESIAN_POINT ( 'NONE',  ( -32.06827542805549314, 14.53851282002520762, 35.54771035678272995 ) ) ;
#5846 = CARTESIAN_POINT ( 'NONE',  ( 34.07766914600081520, 21.40380666527109810, -1.500000000000000000 ) ) ;
#5847 = CARTESIAN_POINT ( 'NONE',  ( -15.21204208253569412, 13.01227270423824045, 5.670038381137163519 ) ) ;
#5848 = CARTESIAN_POINT ( 'NONE',  ( 26.73000961532937225, -9.331429872129930914, 1.500000000000000000 ) ) ;
#5849 = VERTEX_POINT ( 'NONE', #3420 ) ;
#5850 = DIRECTION ( 'NONE',  ( 0.000000000000000000, 1.132880637372608986E-16, -1.000000000000000000 ) ) ;
#5851 = CARTESIAN_POINT ( 'NONE',  ( 13.22505861668195237, -42.10773672056998862, -19.50000000000000355 ) ) ;
#5852 = ORIENTED_EDGE ( 'NONE', *, *, #7671, .T. ) ;
#5853 = CARTESIAN_POINT ( 'NONE',  ( -32.98805937973593672, 0.000000000000000000, 18.00000000000000000 ) ) ;
#5854 = CIRCLE ( 'NONE', #6345, 3.000000000000002665 ) ;
#5855 = FACE_OUTER_BOUND ( 'NONE', #12457, .T. ) ;
#5856 = CARTESIAN_POINT ( 'NONE',  ( -38.65970988490578719, -5.757014596993029976, 35.04328188762917051 ) ) ;
#5857 = EDGE_LOOP ( 'NONE', ( #903, #26096 ) ) ;
#5858 = CARTESIAN_POINT ( 'NONE',  ( 11.33091155972628350, -16.48105488812122488, 5.679672709359370408 ) ) ;
#5859 = VECTOR ( 'NONE', #10010, 1000.000000000000000 ) ;
#5860 = AXIS2_PLACEMENT_3D ( 'NONE', #9198, #16836, #21179 ) ;
#5861 = DIRECTION ( 'NONE',  ( 0.000000000000000000, -1.000000000000000000, 0.000000000000000000 ) ) ;
#5862 = CARTESIAN_POINT ( 'NONE',  ( -19.71415773217921696, 3.369653345580893689, 19.85261563089511938 ) ) ;
#5863 = CIRCLE ( 'NONE', #25301, 7.500000000000013323 ) ;
#5864 = ORIENTED_EDGE ( 'NONE', *, *, #28978, .T. ) ;
#5865 = CARTESIAN_POINT ( 'NONE',  ( -32.98805937973593672, 80.00000000000000000, 8.000000000000003553 ) ) ;
#5866 = CARTESIAN_POINT ( 'NONE',  ( 26.36764545593179676, 31.31467416275351923, -1.500000000000000000 ) ) ;
#5867 = FACE_OUTER_BOUND ( 'NONE', #8602, .T. ) ;
#5868 = CIRCLE ( 'NONE', #23288, 9.084132297865673777 ) ;
#5869 = CARTESIAN_POINT ( 'NONE',  ( -40.57398644816432665, 0.5759020631866372808, -16.50000000000000000 ) ) ;
#5870 = CIRCLE ( 'NONE', #19799, 0.7500000000000006661 ) ;
#5871 = FACE_OUTER_BOUND ( 'NONE', #7763, .T. ) ;
#5872 = DIRECTION ( 'NONE',  ( -0.000000000000000000, -0.000000000000000000, -1.000000000000000000 ) ) ;
#5873 = CARTESIAN_POINT ( 'NONE',  ( -70.00000000000000000, 70.00000000000000000, 12.49999999999999112 ) ) ;
#5874 = VERTEX_POINT ( 'NONE', #336 ) ;
#5875 = CYLINDRICAL_SURFACE ( 'NONE', #1841, 2.999999999999999112 ) ;
#5876 = DIRECTION ( 'NONE',  ( 1.000000000000000000, 0.000000000000000000, 0.000000000000000000 ) ) ;
#5877 = ORIENTED_EDGE ( 'NONE', *, *, #24461, .F. ) ;
#5878 = ORIENTED_EDGE ( 'NONE', *, *, #25979, .T. ) ;
#5879 = FACE_OUTER_BOUND ( 'NONE', #20137, .T. ) ;
#5880 = CIRCLE ( 'NONE', #14820, 20.00000000000000355 ) ;
#5881 = CARTESIAN_POINT ( 'NONE',  ( 1.687027447297431371, 8.840471615930075799, 1.500000000000001332 ) ) ;
#5882 = ORIENTED_EDGE ( 'NONE', *, *, #16786, .F. ) ;
#5883 =( NAMED_UNIT ( * ) PLANE_ANGLE_UNIT ( ) SI_UNIT ( $, .RADIAN. ) );
#5884 = VECTOR ( 'NONE', #28837, 1000.000000000000000 ) ;
#5885 = DIRECTION ( 'NONE',  ( -0.000000000000000000, -0.000000000000000000, -1.000000000000000000 ) ) ;
#5886 = AXIS2_PLACEMENT_3D ( 'NONE', #19328, #12479, #23989 ) ;
#5887 = CARTESIAN_POINT ( 'NONE',  ( 37.16608720827707657, -65.00000000000000000, 12.49999999999999112 ) ) ;
#5888 = ORIENTED_EDGE ( 'NONE', *, *, #2882, .F. ) ;
#5889 = EDGE_LOOP ( 'NONE', ( #29000, #27416, #18759, #20539 ) ) ;
#5890 = CARTESIAN_POINT ( 'NONE',  ( 18.38084888341871093, -7.928499866610144942, 20.34789198813115263 ) ) ;
#5891 = CARTESIAN_POINT ( 'NONE',  ( -4.163336342344337027E-14, 1.387778780781445676E-14, 1.500000000000000000 ) ) ;
#5892 = VECTOR ( 'NONE', #15518, 1000.000000000000000 ) ;
#5893 = CARTESIAN_POINT ( 'NONE',  ( -4.608906612435655248, -7.730328572437724866, -3.621320343559650379 ) ) ;
#5894 = ORIENTED_EDGE ( 'NONE', *, *, #14922, .T. ) ;
#5895 = CARTESIAN_POINT ( 'NONE',  ( -4.773373620122390193, 16.34284820694567486, 18.72771030977187579 ) ) ;
#5896 = VERTEX_POINT ( 'NONE', #26230 ) ;
#5897 = DIRECTION ( 'NONE',  ( 0.000000000000000000, 0.000000000000000000, -1.000000000000000000 ) ) ;
#5898 = ORIENTED_EDGE ( 'NONE', *, *, #1710, .F. ) ;
#5899 = DIRECTION ( 'NONE',  ( -0.000000000000000000, 0.000000000000000000, 1.000000000000000000 ) ) ;
#5900 = AXIS2_PLACEMENT_3D ( 'NONE', #3425, #10446, #5462 ) ;
#5901 = CARTESIAN_POINT ( 'NONE',  ( 36.69132079237465405, -14.42015626554423235, 31.58303039899921316 ) ) ;
#5902 = CARTESIAN_POINT ( 'NONE',  ( 16.58472157312809259, 4.055073576757204812, 6.131018562779544823 ) ) ;
#5903 = CARTESIAN_POINT ( 'NONE',  ( -15.00589365688690435, 13.24944937571967962, 18.49267272388512140 ) ) ;
#5904 = CIRCLE ( 'NONE', #13875, 9.084132297865673777 ) ;
#5905 = AXIS2_PLACEMENT_3D ( 'NONE', #21469, #110, #9630 ) ;
#5906 = CARTESIAN_POINT ( 'NONE',  ( -7.931808866138725378, -15.11281102451791547, 20.06253562465620632 ) ) ;
#5907 = EDGE_CURVE ( 'NONE', #21461, #9461, #4868, .T. ) ;
#5908 = CARTESIAN_POINT ( 'NONE',  ( -19.62935297797563905, -3.832558109936532897, 24.50000000000000000 ) ) ;
#5909 = CARTESIAN_POINT ( 'NONE',  ( -19.91230480659700319, 2.053870633397347323, 18.44527579819791185 ) ) ;
#5910 = DIRECTION ( 'NONE',  ( 0.000000000000000000, -1.000000000000000000, 0.000000000000000000 ) ) ;
#5911 = EDGE_LOOP ( 'NONE', ( #921, #16729, #4788, #17379 ) ) ;
#5912 = CYLINDRICAL_SURFACE ( 'NONE', #28244, 3.559164065751841743 ) ;
#5913 = CARTESIAN_POINT ( 'NONE',  ( 11.24508296785401917, -16.56092475412858889, 18.35718225375110180 ) ) ;
#5914 = AXIS2_PLACEMENT_3D ( 'NONE', #13375, #30048, #15072 ) ;
#5915 = CARTESIAN_POINT ( 'NONE',  ( 35.00000000000000000, 90.00000000000001421, -22.50000000000002487 ) ) ;
#5916 = VERTEX_POINT ( 'NONE', #7372 ) ;
#5917 = EDGE_LOOP ( 'NONE', ( #27094, #348, #5878, #19538 ) ) ;
#5918 = CARTESIAN_POINT ( 'NONE',  ( 18.28487737789067324, -8.104377114558884543, 18.34726407865098707 ) ) ;
#5919 = DIRECTION ( 'NONE',  ( 1.000000000000000000, 0.000000000000000000, 0.000000000000000000 ) ) ;
#5920 = EDGE_CURVE ( 'NONE', #16597, #19689, #29504, .T. ) ;
#5921 = DIRECTION ( 'NONE',  ( 1.000000000000000000, 0.000000000000000000, 0.000000000000000000 ) ) ;
#5922 = EDGE_LOOP ( 'NONE', ( #5864, #16546, #15139, #199 ) ) ;
#5923 = CARTESIAN_POINT ( 'NONE',  ( -24.35970437652574105, 13.37404834226503247, 42.96778633356043287 ) ) ;
#5924 = DIRECTION ( 'NONE',  ( 1.000000000000000000, 0.000000000000000000, 0.000000000000000000 ) ) ;
#5925 = DIRECTION ( 'NONE',  ( 0.000000000000000000, 1.000000000000000000, 0.000000000000000000 ) ) ;
#5926 = ORIENTED_EDGE ( 'NONE', *, *, #22730, .F. ) ;
#5927 = DIRECTION ( 'NONE',  ( 0.000000000000000000, 0.000000000000000000, 1.000000000000000000 ) ) ;
#5928 = ADVANCED_FACE ( 'NONE', ( #23891 ), #27131, .F. ) ;
#5929 = AXIS2_PLACEMENT_3D ( 'NONE', #30799, #23461, #20668 ) ;
#5930 = CARTESIAN_POINT ( 'NONE',  ( 12.20325286834225942, 11.91007939804258875, 5.678370764302467677 ) ) ;
#5931 = AXIS2_PLACEMENT_3D ( 'NONE', #3778, #8614, #27341 ) ;
#5932 = CARTESIAN_POINT ( 'NONE',  ( 19.88037316481945282, 2.342382300094909553, 7.176035686813569292 ) ) ;
#5933 = ORIENTED_EDGE ( 'NONE', *, *, #18705, .F. ) ;
#5934 = EDGE_CURVE ( 'NONE', #5507, #24431, #22542, .T. ) ;
#5935 = CARTESIAN_POINT ( 'NONE',  ( 14.97043017101258400, 13.28903844302880444, 5.657991946698900598 ) ) ;
#5936 = ORIENTED_EDGE ( 'NONE', *, *, #16826, .T. ) ;
#5937 = CARTESIAN_POINT ( 'NONE',  ( 9.471281197126602436, 0.4564504349074720024, 21.50000000000000000 ) ) ;
#5938 = CARTESIAN_POINT ( 'NONE',  ( 29.81954908927654202, -15.48017614753372584, 37.15913391342340333 ) ) ;
#5939 = ORIENTED_EDGE ( 'NONE', *, *, #5951, .T. ) ;
#5940 = AXIS2_PLACEMENT_3D ( 'NONE', #18280, #30574, #21051 ) ;
#5941 = ORIENTED_EDGE ( 'NONE', *, *, #18725, .T. ) ;
#5942 = CARTESIAN_POINT ( 'NONE',  ( 4.592382419210019329, 19.48389062382846504, 5.951255046771932733 ) ) ;
#5943 = CARTESIAN_POINT ( 'NONE',  ( 33.56327786402390245, 10.34181101807379299, 39.87954049117193023 ) ) ;
#5944 = LINE ( 'NONE', #8457, #20790 ) ;
#5945 = VECTOR ( 'NONE', #5685, 1000.000000000000000 ) ;
#5946 = CARTESIAN_POINT ( 'NONE',  ( -35.45878215871336181, -7.046087300371452145, 34.64822579837505856 ) ) ;
#5947 = CARTESIAN_POINT ( 'NONE',  ( 35.00000000000000000, 70.00000000000000000, -22.50000000000003908 ) ) ;
#5948 = CYLINDRICAL_SURFACE ( 'NONE', #28791, 0.7499999999999997780 ) ;
#5949 = EDGE_CURVE ( 'NONE', #1513, #19394, #7957, .T. ) ;
#5950 = ORIENTED_EDGE ( 'NONE', *, *, #4110, .T. ) ;
#5951 = EDGE_CURVE ( 'NONE', #28288, #984, #19565, .T. ) ;
#5952 = CARTESIAN_POINT ( 'NONE',  ( 9.471281197126604212, 0.4564504349074710587, 1.500000000000001332 ) ) ;
#5953 = CARTESIAN_POINT ( 'NONE',  ( 15.58729175431055047, -6.863221649612943231, 7.500898271101006820 ) ) ;
#5954 = CARTESIAN_POINT ( 'NONE',  ( -14.00963640524698306, 9.767049959719264152, 19.47783254395485031 ) ) ;
#5955 = VECTOR ( 'NONE', #22061, 1000.000000000000000 ) ;
#5956 = CARTESIAN_POINT ( 'NONE',  ( 42.15079010498045875, 66.40049817264792864, 62.28254144336177944 ) ) ;
#5957 = DIRECTION ( 'NONE',  ( -0.4154150130018972598, -0.9096319953545133341, 0.000000000000000000 ) ) ;
#5958 = CARTESIAN_POINT ( 'NONE',  ( 37.99999999999999289, 70.00000000000000000, -69.50000000000000000 ) ) ;
#5959 = EDGE_CURVE ( 'NONE', #15686, #3764, #24621, .T. ) ;
#5960 = DIRECTION ( 'NONE',  ( 0.000000000000000000, 0.000000000000000000, 1.000000000000000000 ) ) ;
#5961 = EDGE_CURVE ( 'NONE', #6583, #1130, #27443, .T. ) ;
#5962 = CARTESIAN_POINT ( 'NONE',  ( -5.025762778208110682, 19.37674427759095863, 19.56050940960062690 ) ) ;
#5963 = DIRECTION ( 'NONE',  ( 0.000000000000000000, 1.132880637372608986E-16, -1.000000000000000000 ) ) ;
#5964 = DIRECTION ( 'NONE',  ( -1.000000000000000000, 0.000000000000000000, 0.000000000000000000 ) ) ;
#5965 = ADVANCED_FACE ( 'NONE', ( #11372 ), #15354, .T. ) ;
#5966 = DIRECTION ( 'NONE',  ( 1.000000000000000000, 0.000000000000000000, 0.000000000000000000 ) ) ;
#5967 = DIRECTION ( 'NONE',  ( -0.000000000000000000, -0.000000000000000000, 1.000000000000000000 ) ) ;
#5968 = EDGE_CURVE ( 'NONE', #21915, #16485, #30511, .T. ) ;
#5969 = ORIENTED_EDGE ( 'NONE', *, *, #20809, .F. ) ;
#5970 = CARTESIAN_POINT ( 'NONE',  ( -33.52437897089259877, -10.76376600292166863, 35.54771035675473456 ) ) ;
#5971 = CARTESIAN_POINT ( 'NONE',  ( -33.51206231511395117, 9.871883628028008673, 40.06435153362845369 ) ) ;
#5972 = ORIENTED_EDGE ( 'NONE', *, *, #22924, .F. ) ;
#5973 = EDGE_CURVE ( 'NONE', #897, #27328, #8113, .T. ) ;
#5974 = ORIENTED_EDGE ( 'NONE', *, *, #30325, .T. ) ;
#5975 = CARTESIAN_POINT ( 'NONE',  ( -19.72722132040463450, 3.293256439147198122, 6.033082186765059696 ) ) ;
#5976 = CARTESIAN_POINT ( 'NONE',  ( -19.91205802435384697, 1.875831072725641313, 18.54958172136248251 ) ) ;
#5977 = VERTEX_POINT ( 'NONE', #23965 ) ;
#5978 = LINE ( 'NONE', #3022, #15867 ) ;
#5979 = CARTESIAN_POINT ( 'NONE',  ( 2.454608198648450479, 49.94209336002347044, -69.80612517421458563 ) ) ;
#5980 = DIRECTION ( 'NONE',  ( 0.000000000000000000, 0.000000000000000000, -1.000000000000000000 ) ) ;
#5981 = DIRECTION ( 'NONE',  ( 0.000000000000000000, -1.132880637372608986E-16, 1.000000000000000000 ) ) ;
#5982 = CARTESIAN_POINT ( 'NONE',  ( -5.978582532085236600, 19.10413086404602723, 18.34798005862662507 ) ) ;
#5983 = DIRECTION ( 'NONE',  ( 0.000000000000000000, 0.000000000000000000, 1.000000000000000000 ) ) ;
#5984 = DIRECTION ( 'NONE',  ( 0.000000000000000000, 0.000000000000000000, -1.000000000000000000 ) ) ;
#5985 = CARTESIAN_POINT ( 'NONE',  ( 14.59923040764597957, 13.69601292063889275, 20.25542030744407640 ) ) ;
#5986 = EDGE_CURVE ( 'NONE', #16618, #24186, #19544, .T. ) ;
#5987 = ORIENTED_EDGE ( 'NONE', *, *, #4231, .T. ) ;
#5988 = ADVANCED_FACE ( 'NONE', ( #7143 ), #6987, .F. ) ;
#5989 = CIRCLE ( 'NONE', #9463, 9.482273699623480212 ) ;
#5990 = CARTESIAN_POINT ( 'NONE',  ( 0.000000000000000000, 0.000000000000000000, 21.50000000000000000 ) ) ;
#5991 = ADVANCED_FACE ( 'NONE', ( #21008 ), #14005, .F. ) ;
#5992 = CARTESIAN_POINT ( 'NONE',  ( 9.406652940105985294, -1.195154792889423057, 21.50000000000000000 ) ) ;
#5993 = CARTESIAN_POINT ( 'NONE',  ( 10.45210396439254197, -13.49311571392157028, 7.366751648393900176 ) ) ;
#5994 = CARTESIAN_POINT ( 'NONE',  ( -5.374868878254082105, 44.10336124695542992, -19.50000000000000355 ) ) ;
#5995 = CARTESIAN_POINT ( 'NONE',  ( -33.03011559203990544, 8.976883822286589876, 36.52918211139306237 ) ) ;
#5996 = ORIENTED_EDGE ( 'NONE', *, *, #14149, .T. ) ;
#5997 = ORIENTED_EDGE ( 'NONE', *, *, #11106, .F. ) ;
#5998 = CYLINDRICAL_SURFACE ( 'NONE', #15904, 15.00000000000000000 ) ;
#5999 = CARTESIAN_POINT ( 'NONE',  ( -23.96732207938974213, -33.98584080153308662, -1.500000000000000000 ) ) ;
#6000 = DIRECTION ( 'NONE',  ( 1.000000000000000000, 0.000000000000000000, 0.000000000000000000 ) ) ;
#6001 = DIRECTION ( 'NONE',  ( 1.000000000000000000, 0.000000000000000000, 0.000000000000000000 ) ) ;
#6002 = ORIENTED_EDGE ( 'NONE', *, *, #28246, .F. ) ;
#6003 = VECTOR ( 'NONE', #981, 1000.000000000000000 ) ;
#6004 = DIRECTION ( 'NONE',  ( 0.000000000000000000, -0.000000000000000000, -1.000000000000000000 ) ) ;
#6005 = CARTESIAN_POINT ( 'NONE',  ( -2.687479362164884034, -44.39187623478217404, -19.50000000000000355 ) ) ;
#6006 = EDGE_LOOP ( 'NONE', ( #59, #25868, #11734, #28083 ) ) ;
#6007 = DIRECTION ( 'NONE',  ( -1.000000000000000000, 0.000000000000000000, 0.000000000000000000 ) ) ;
#6008 = CARTESIAN_POINT ( 'NONE',  ( -7.885088086771752991, -41.65010312772935208, 28.91342085574027720 ) ) ;
#6009 = VERTEX_POINT ( 'NONE', #21152 ) ;
#6010 = DIRECTION ( 'NONE',  ( -0.000000000000000000, -0.000000000000000000, -1.000000000000000000 ) ) ;
#6011 = ADVANCED_FACE ( 'NONE', ( #28190 ), #28661, .F. ) ;
#6012 = CARTESIAN_POINT ( 'NONE',  ( 8.999114229549594057, -0.1262659238204522361, -3.621320343559650379 ) ) ;
#6013 = ADVANCED_FACE ( 'NONE', ( #14618 ), #16654, .F. ) ;
#6014 = CYLINDRICAL_SURFACE ( 'NONE', #4371, 20.00000000000000000 ) ;
#6015 = DIRECTION ( 'NONE',  ( 0.000000000000000000, 0.000000000000000000, 1.000000000000000000 ) ) ;
#6016 = EDGE_LOOP ( 'NONE', ( #7658, #1225, #30802, #28376, #8126, #10649, #14585, #14876 ) ) ;
#6017 = CARTESIAN_POINT ( 'NONE',  ( 12.35522425158188931, 11.74279415389956327, 18.34798005863078885 ) ) ;
#6018 = CARTESIAN_POINT ( 'NONE',  ( 17.79239818699415920, 14.89473990422378158, 1.500000000000000000 ) ) ;
#6019 = DIRECTION ( 'NONE',  ( 0.000000000000000000, -0.000000000000000000, -1.000000000000000000 ) ) ;
#6020 = VECTOR ( 'NONE', #26334, 1000.000000000000000 ) ;
#6021 = CARTESIAN_POINT ( 'NONE',  ( 0.000000000000000000, -2.322405306613848348E-14, 117.5000000000000000 ) ) ;
#6022 = PLANE ( 'NONE',  #30766 ) ;
#6023 = DIRECTION ( 'NONE',  ( -0.000000000000000000, -0.000000000000000000, -1.000000000000000000 ) ) ;
#6024 = FACE_OUTER_BOUND ( 'NONE', #7908, .T. ) ;
#6025 = ORIENTED_EDGE ( 'NONE', *, *, #5099, .T. ) ;
#6026 = CARTESIAN_POINT ( 'NONE',  ( 9.051788058582081575, -14.41610800086747801, 6.973843882838225205 ) ) ;
#6027 = CARTESIAN_POINT ( 'NONE',  ( 33.36623411648999848, -9.470136927103574465, 40.31594401536676031 ) ) ;
#6028 = CARTESIAN_POINT ( 'NONE',  ( -8.546423435383418976, -14.74799740001549786, 18.34798005863078885 ) ) ;
#6029 = ORIENTED_EDGE ( 'NONE', *, *, #266, .T. ) ;
#6030 = ORIENTED_EDGE ( 'NONE', *, *, #14679, .T. ) ;
#6031 = B_SPLINE_CURVE_WITH_KNOTS ( 'NONE', 3,
 ( #6500, #11029, #22870, #10876, #11182, #18203, #1362 ),
 .UNSPECIFIED., .F., .F.,
 ( 4, 3, 4 ),
 ( 0.000000000000000000, 0.005031266823827981044, 0.01006253384101580411 ),
 .UNSPECIFIED. ) ;
#6032 = CARTESIAN_POINT ( 'NONE',  ( 0.000000000000000000, 0.000000000000000000, 12.49999999999999112 ) ) ;
#6033 = CARTESIAN_POINT ( 'NONE',  ( 32.74775157611827581, 27.21557300921217859, -19.50000000000000355 ) ) ;
#6034 = DIRECTION ( 'NONE',  ( 1.000000000000000000, 0.000000000000000000, -0.000000000000000000 ) ) ;
#6035 = VERTEX_POINT ( 'NONE', #21472 ) ;
#6036 = CARTESIAN_POINT ( 'NONE',  ( -6.047835543816287185, 15.95440705816254479, 18.45571264222803975 ) ) ;
#6037 = CARTESIAN_POINT ( 'NONE',  ( 9.436006877715755081, -14.17980878084792629, 20.22273502201483808 ) ) ;
#6038 = EDGE_LOOP ( 'NONE', ( #25329, #3027, #16141, #23402 ) ) ;
#6039 = VERTEX_POINT ( 'NONE', #2291 ) ;
#6040 = CARTESIAN_POINT ( 'NONE',  ( -37.99999999999999289, 209.2686044187655909, -69.49999999999998579 ) ) ;
#6041 = CARTESIAN_POINT ( 'NONE',  ( 19.73705937795079635, 3.341332093703275330, 20.33971507717571114 ) ) ;
#6042 = AXIS2_PLACEMENT_3D ( 'NONE', #1345, #20667, #10863 ) ;
#6043 = DIRECTION ( 'NONE',  ( 0.000000000000000000, 0.000000000000000000, -1.000000000000000000 ) ) ;
#6044 = CARTESIAN_POINT ( 'NONE',  ( -12.81862250463242781, 40.16661589154484346, 29.04586181293521108 ) ) ;
#6045 = VERTEX_POINT ( 'NONE', #28364 ) ;
#6046 = CARTESIAN_POINT ( 'NONE',  ( -4.623640074040875625, 16.38233772743891947, 19.66962785902261857 ) ) ;
#6047 = VERTEX_POINT ( 'NONE', #16497 ) ;
#6048 = CARTESIAN_POINT ( 'NONE',  ( 7.500000000000000000, 10.39230484541327471, 0.000000000000000000 ) ) ;
#6049 = EDGE_CURVE ( 'NONE', #14664, #1286, #28818, .T. ) ;
#6050 = VERTEX_POINT ( 'NONE', #2002 ) ;
#6051 = CARTESIAN_POINT ( 'NONE',  ( 14.87898187659695992, 13.36471393577513389, 18.34798005863227388 ) ) ;
#6052 = AXIS2_PLACEMENT_3D ( 'NONE', #28185, #2456, #9315 ) ;
#6053 = CARTESIAN_POINT ( 'NONE',  ( -4.776122516674677878E-15, -42.50000000000000000, 28.83974596215560737 ) ) ;
#6054 = LINE ( 'NONE', #25080, #29279 ) ;
#6055 = LINE ( 'NONE', #15564, #5147 ) ;
#6056 = CARTESIAN_POINT ( 'NONE',  ( 1.047421501149297329, -17.02264912680942643, 5.653604225791661442 ) ) ;
#6057 = CARTESIAN_POINT ( 'NONE',  ( -16.99797872337576266, 1.390050218429698115, 20.34789198813115263 ) ) ;
#6058 = CARTESIAN_POINT ( 'NONE',  ( -8.658642352887948590, -14.67867993418359340, 5.651492010659114662 ) ) ;
#6059 = LINE ( 'NONE', #30227, #2907 ) ;
#6060 = EDGE_LOOP ( 'NONE', ( #29299, #30194, #5717, #15131 ) ) ;
#6061 = CYLINDRICAL_SURFACE ( 'NONE', #6822, 7.500000000000000000 ) ;
#6062 = CARTESIAN_POINT ( 'NONE',  ( -32.05743189141918492, 24.22168755390175576, 17.93996624350626590 ) ) ;
#6063 = CIRCLE ( 'NONE', #18518, 9.482273699623480212 ) ;
#6064 = CARTESIAN_POINT ( 'NONE',  ( -19.84403786039537465, 2.492757843112275218, 18.34798005863227388 ) ) ;
#6065 = ORIENTED_EDGE ( 'NONE', *, *, #7292, .T. ) ;
#6066 = EDGE_LOOP ( 'NONE', ( #5644, #20685, #8967, #4187 ) ) ;
#6067 = CARTESIAN_POINT ( 'NONE',  ( 42.08856419149575601, 68.37167730218320116, 12.71573695841679985 ) ) ;
#6068 = CYLINDRICAL_SURFACE ( 'NONE', #30052, 45.00000000000000711 ) ;
#6069 = CARTESIAN_POINT ( 'NONE',  ( -4.721574378597743760, 16.35655934831870795, 6.111214848085761986 ) ) ;
#6070 = VERTEX_POINT ( 'NONE', #21318 ) ;
#6071 = DIRECTION ( 'NONE',  ( 1.000000000000000000, 0.000000000000000000, 0.000000000000000000 ) ) ;
#6072 = CARTESIAN_POINT ( 'NONE',  ( 9.864937699929955173, -13.90063973435163724, 5.652196082368482699 ) ) ;
#6073 = DIRECTION ( 'NONE',  ( 1.000000000000000000, 0.000000000000000000, -0.000000000000000000 ) ) ;
#6074 = ORIENTED_EDGE ( 'NONE', *, *, #19110, .F. ) ;
#6075 = CIRCLE ( 'NONE', #28005, 0.7441270634457198829 ) ;
#6076 = CARTESIAN_POINT ( 'NONE',  ( 0.1262659238204208167, 8.999114229549594057, 21.50000000000000000 ) ) ;
#6077 = CARTESIAN_POINT ( 'NONE',  ( 14.66647055262614785, 13.62412221374329846, 5.704143890883081269 ) ) ;
#6078 = CARTESIAN_POINT ( 'NONE',  ( 19.79578860058543910, 2.975267875541940832, 5.670038381137163519 ) ) ;
#6079 = ORIENTED_EDGE ( 'NONE', *, *, #18399, .F. ) ;
#6080 = CYLINDRICAL_SURFACE ( 'NONE', #8860, 0.7500000000000006661 ) ;
#6081 = CARTESIAN_POINT ( 'NONE',  ( -13.88720712124151468, 9.928229803686351218, 18.73314399819311760 ) ) ;
#6082 = CIRCLE ( 'NONE', #28990, 0.7500000000000006661 ) ;
#6083 = ORIENTED_EDGE ( 'NONE', *, *, #1549, .F. ) ;
#6084 = EDGE_LOOP ( 'NONE', ( #19487, #14226, #1883, #22909 ) ) ;
#6085 = EDGE_CURVE ( 'NONE', #18, #12762, #11814, .T. ) ;
#6086 = CARTESIAN_POINT ( 'NONE',  ( 3.077027262763125215, 16.79827892558873970, 6.447548852708279377 ) ) ;
#6087 = EDGE_CURVE ( 'NONE', #26020, #3416, #26159, .T. ) ;
#6088 = DIRECTION ( 'NONE',  ( 1.000000000000000000, -0.000000000000000000, -0.000000000000000000 ) ) ;
#6089 = CARTESIAN_POINT ( 'NONE',  ( 6.070111251556830290, 19.05682731086504944, 19.96302680909623817 ) ) ;
#6090 = ORIENTED_EDGE ( 'NONE', *, *, #7080, .F. ) ;
#6091 = CARTESIAN_POINT ( 'NONE',  ( 9.025811419443954264, -14.43167044742871497, 19.11611934778430921 ) ) ;
#6092 = CARTESIAN_POINT ( 'NONE',  ( 16.09518941752841670, 6.251081041772567737, 1.500000000000000000 ) ) ;
#6093 = ORIENTED_EDGE ( 'NONE', *, *, #20279, .F. ) ;
#6094 = VECTOR ( 'NONE', #29902, 1000.000000000000000 ) ;
#6095 = CARTESIAN_POINT ( 'NONE',  ( 39.99999999999998579, 80.00000000000001421, 57.49999999999998579 ) ) ;
#6096 = CARTESIAN_POINT ( 'NONE',  ( 18.13085077595200190, -8.485104792618537672, 5.796888747622817029 ) ) ;
#6097 = CARTESIAN_POINT ( 'NONE',  ( -13.92530307126622802, 9.878387810998203733, 18.82680253904184298 ) ) ;
#6098 = FACE_OUTER_BOUND ( 'NONE', #788, .T. ) ;
#6099 = ORIENTED_EDGE ( 'NONE', *, *, #13186, .F. ) ;
#6100 = ORIENTED_EDGE ( 'NONE', *, *, #28425, .F. ) ;
#6101 = DIRECTION ( 'NONE',  ( -1.000000000000000000, 0.000000000000000000, -0.000000000000000000 ) ) ;
#6102 = FACE_OUTER_BOUND ( 'NONE', #18357, .T. ) ;
#6103 = CARTESIAN_POINT ( 'NONE',  ( -5.147812317479953492, 19.34466387292044232, 19.87181966307587544 ) ) ;
#6104 = CARTESIAN_POINT ( 'NONE',  ( -2.523760598493608232, -1.621922452366769907, 24.50000000000000000 ) ) ;
#6105 = DIRECTION ( 'NONE',  ( -0.000000000000000000, -0.000000000000000000, -1.000000000000000000 ) ) ;
#6106 = CARTESIAN_POINT ( 'NONE',  ( 0.000000000000000000, 0.000000000000000000, 21.50000000000000000 ) ) ;
#6107 = EDGE_LOOP ( 'NONE', ( #11555, #27093, #27569, #3308 ) ) ;
#6108 = EDGE_CURVE ( 'NONE', #9077, #4023, #28509, .T. ) ;
#6109 = DIRECTION ( 'NONE',  ( 1.000000000000000000, 0.000000000000000000, 0.000000000000000000 ) ) ;
#6110 = CARTESIAN_POINT ( 'NONE',  ( 33.42925964089140933, 11.06161099612213405, 39.78814634291935448 ) ) ;
#6111 = CARTESIAN_POINT ( 'NONE',  ( 7.500000000000000000, 0.000000000000000000, 0.000000000000000000 ) ) ;
#6112 = EDGE_LOOP ( 'NONE', ( #17352, #23201, #18330, #6297 ) ) ;
#6113 = VECTOR ( 'NONE', #22834, 1000.000000000000227 ) ;
#6114 = VECTOR ( 'NONE', #26857, 1000.000000000000227 ) ;
#6115 = EDGE_CURVE ( 'NONE', #15627, #15944, #23026, .T. ) ;
#6116 = ORIENTED_EDGE ( 'NONE', *, *, #5839, .T. ) ;
#6117 = DIRECTION ( 'NONE',  ( 1.000000000000000000, 0.000000000000000000, 0.000000000000000000 ) ) ;
#6118 = AXIS2_PLACEMENT_3D ( 'NONE', #10274, #8256, #12782 ) ;
#6119 = UNCERTAINTY_MEASURE_WITH_UNIT (LENGTH_MEASURE( 1.000000000000000082E-05 ), #26801, 'distance_accuracy_value', 'NONE');
#6120 = CARTESIAN_POINT ( 'NONE',  ( -8.637616862297813114, 3.912171961292039590, 13.00000000000000178 ) ) ;
#6121 = ORIENTED_EDGE ( 'NONE', *, *, #24601, .F. ) ;
#6122 = CARTESIAN_POINT ( 'NONE',  ( -32.28307784207223108, 8.475829241206282560, 37.38016955275591613 ) ) ;
#6123 = EDGE_CURVE ( 'NONE', #29565, #1203, #12131, .T. ) ;
#6124 = CARTESIAN_POINT ( 'NONE',  ( 11.91715319254153371, 48.56235700707689062, -45.83731355574434474 ) ) ;
#6125 = EDGE_CURVE ( 'NONE', #22613, #19044, #7921, .T. ) ;
#6126 = CARTESIAN_POINT ( 'NONE',  ( -12.13118772005164026, -40.43574026512624897, 21.42753784591547017 ) ) ;
#6127 = DIRECTION ( 'NONE',  ( -1.000000000000000000, 0.000000000000000000, 0.000000000000000000 ) ) ;
#6128 = CARTESIAN_POINT ( 'NONE',  ( 9.216505592218814158, -7.781333699927420966, 1.500000000000000000 ) ) ;
#6129 = CARTESIAN_POINT ( 'NONE',  ( 4.340342926364956888, 8.430595340551274575, 1.500000000000001332 ) ) ;
#6130 = CARTESIAN_POINT ( 'NONE',  ( 8.499586724479435418, 2.959227181723830036, -1.500000000000001332 ) ) ;
#6131 = CARTESIAN_POINT ( 'NONE',  ( 5.687793815610356241, -6.974883619896809606, -3.621320343559650379 ) ) ;
#6132 = EDGE_CURVE ( 'NONE', #5146, #9927, #22030, .T. ) ;
#6133 = ORIENTED_EDGE ( 'NONE', *, *, #2115, .T. ) ;
#6134 = EDGE_CURVE ( 'NONE', #13976, #15490, #19451, .T. ) ;
#6135 = CARTESIAN_POINT ( 'NONE',  ( -11.05774036494470103, -16.68675304545164195, 18.55820869691756769 ) ) ;
#6136 = LINE ( 'NONE', #25011, #13791 ) ;
#6137 = CARTESIAN_POINT ( 'NONE',  ( -5.755751318732963639, 16.05090033862148857, 7.627891251804737927 ) ) ;
#6138 = ADVANCED_FACE ( 'NONE', ( #10407 ), #12596, .T. ) ;
#6139 = AXIS2_PLACEMENT_3D ( 'NONE', #7163, #21174, #30698 ) ;
#6140 = CARTESIAN_POINT ( 'NONE',  ( -14.80332652839582863, -8.501125445468646902, 18.73743063545763121 ) ) ;
#6141 = AXIS2_PLACEMENT_3D ( 'NONE', #25826, #28624, #11626 ) ;
#6142 = CARTESIAN_POINT ( 'NONE',  ( -40.89187623478217404, 5.790488632116478129, -19.50000000000000355 ) ) ;
#6143 = CARTESIAN_POINT ( 'NONE',  ( -33.43024933835881285, 9.611735609129386404, 35.97296397483977159 ) ) ;
#6144 = VERTEX_POINT ( 'NONE', #19601 ) ;
#6145 = ORIENTED_EDGE ( 'NONE', *, *, #22910, .T. ) ;
#6146 = CARTESIAN_POINT ( 'NONE',  ( -31.79271162922631788, 14.90794587988477815, 35.64318943584552812 ) ) ;
#6147 = CARTESIAN_POINT ( 'NONE',  ( -13.22505861668333083, 42.10773672057167261, -19.50000000000000355 ) ) ;
#6148 = CIRCLE ( 'NONE', #21562, 9.482273699623480212 ) ;
#6149 = CARTESIAN_POINT ( 'NONE',  ( -14.79144470604038375, 13.48820156989937047, 6.111214848085761986 ) ) ;
#6150 = PLANE ( 'NONE',  #15055 ) ;
#6151 = ORIENTED_EDGE ( 'NONE', *, *, #19904, .T. ) ;
#6152 = CARTESIAN_POINT ( 'NONE',  ( 4.049916833591940879, 16.55712665779027049, 7.652108011868850923 ) ) ;
#6153 = CARTESIAN_POINT ( 'NONE',  ( -20.65888525914364493, -38.75220717792906555, -19.50000000000000355 ) ) ;
#6154 = CARTESIAN_POINT ( 'NONE',  ( -8.579043560828052861, -14.72784502467623291, 5.651989602109218858 ) ) ;
#6155 = EDGE_CURVE ( 'NONE', #12669, #27956, #19923, .T. ) ;
#6156 = ORIENTED_EDGE ( 'NONE', *, *, #23869, .T. ) ;
#6157 = EDGE_CURVE ( 'NONE', #6669, #10785, #9105, .T. ) ;
#6158 = B_SPLINE_SURFACE_WITH_KNOTS ( 'NONE', 3, 1, ( 
 ( #13509, #22991 ),
 ( #20362, #20657 ),
 ( #13661, #29887 ),
 ( #23143, #30331 ),
 ( #18487, #27991 ),
 ( #16139, #25654 ),
 ( #4272, #2714 ),
 ( #4894, #23751 ),
 ( #16907, #4733 ),
 ( #16443, #24063 ),
 ( #9882, #362 ),
 ( #19400, #11930 ),
 ( #12221, #2403 ),
 ( #21571, #6932 ),
 ( #21101, #2083 ),
 ( #21421, #26423 ),
 ( #25956, #21722 ),
 ( #21254, #9266 ),
 ( #28918, #28307 ),
 ( #23595, #23446 ),
 ( #14565, #16289 ),
 ( #9722, #5052 ),
 ( #7081, #25808 ),
 ( #64, #7227 ),
 ( #18948, #7397 ),
 ( #2238, #16588 ),
 ( #9576, #19087 ),
 ( #12076, #4439 ),
 ( #11606, #28457 ),
 ( #30619, #11757 ),
 ( #4584, #14085 ) ),
 .UNSPECIFIED., .F., .F., .F.,
 ( 4, 3, 3, 3, 3, 3, 3, 3, 3, 3, 4 ),
 ( 2, 2 ),
 ( 0.4999999998345686092, 0.5360336730431942698, 0.5907651151589017324, 0.6456034593241839481, 0.6998270958050443191, 0.7529536536315944995, 0.8052385063053264513, 0.8575343587103996246, 0.9106564858195047574, 0.9648414833209688624, 1.000000006602610014 ),
 ( 0.000000000000000000, 1.000000000000000000 ),
 .UNSPECIFIED. ) ;
#6159 = VECTOR ( 'NONE', #28989, 1000.000000000000000 ) ;
#6160 = CARTESIAN_POINT ( 'NONE',  ( -0.9370274472974918778, -8.840471615930066918, -1.500000000000002665 ) ) ;
#6161 = EDGE_CURVE ( 'NONE', #27927, #24914, #17718, .T. ) ;
#6162 = CARTESIAN_POINT ( 'NONE',  ( -12.34832590236237237, -40.32090071188812885, 34.56244595848355772 ) ) ;
#6163 = ORIENTED_EDGE ( 'NONE', *, *, #28673, .T. ) ;
#6164 = CARTESIAN_POINT ( 'NONE',  ( -30.03792366816882620, -15.52577997660842435, 41.18702913624207440 ) ) ;
#6165 = CIRCLE ( 'NONE', #29567, 45.00000000000000711 ) ;
#6166 = AXIS2_PLACEMENT_3D ( 'NONE', #3941, #20148, #29978 ) ;
#6167 = EDGE_CURVE ( 'NONE', #22024, #24302, #568, .T. ) ;
#6168 = B_SPLINE_CURVE_WITH_KNOTS ( 'NONE', 3,
 ( #13188, #13345, #18175, #27681, #6310, #29663, #15300, #3466, #10480, #501 ),
 .UNSPECIFIED., .F., .F.,
 ( 4, 2, 2, 2, 4 ),
 ( 0.0007598054600062437158, 0.001542965791078105241, 0.002326126122149966766, 0.003109286453221827857, 0.003892446784293689382 ),
 .UNSPECIFIED. ) ;
#6169 = DIRECTION ( 'NONE',  ( 1.000000000000000000, 0.000000000000000000, 0.000000000000000000 ) ) ;
#6170 = CARTESIAN_POINT ( 'NONE',  ( -24.44496207165490276, 7.595930209050158588, 45.15942333309111945 ) ) ;
#6171 = ORIENTED_EDGE ( 'NONE', *, *, #14771, .T. ) ;
#6172 = CARTESIAN_POINT ( 'NONE',  ( 23.10264100946039534, 11.84391650453516043, 44.79593483593096437 ) ) ;
#6173 = CARTESIAN_POINT ( 'NONE',  ( 31.89119714134807637, 14.79609055705961573, 35.60128781023431799 ) ) ;
#6174 = CARTESIAN_POINT ( 'NONE',  ( 16.18505772753977823, -5.447928388670486122, 6.917457548096561659 ) ) ;
#6175 = EDGE_CURVE ( 'NONE', #22154, #544, #7758, .T. ) ;
#6176 = DIRECTION ( 'NONE',  ( -1.000000000000000000, 0.000000000000000000, 0.000000000000000000 ) ) ;
#6177 = DIRECTION ( 'NONE',  ( -1.000000000000000000, 0.000000000000000000, 0.000000000000000000 ) ) ;
#6178 = DIRECTION ( 'NONE',  ( 1.000000000000000000, 0.000000000000000000, 0.000000000000000000 ) ) ;
#6179 = CARTESIAN_POINT ( 'NONE',  ( 3.221450758838616757, 1.621276839356792454, 1.500000000000000000 ) ) ;
#6180 = CARTESIAN_POINT ( 'NONE',  ( 0.000000000000000000, -2.435693370351110282E-15, 21.50000000000000355 ) ) ;
#6181 = DIRECTION ( 'NONE',  ( -0.7557495743542579358, 0.6548607339452854337, -0.000000000000000000 ) ) ;
#6182 = CARTESIAN_POINT ( 'NONE',  ( 33.41032657756569790, -9.567127522732029377, 40.24698379951695415 ) ) ;
#6183 = CARTESIAN_POINT ( 'NONE',  ( 0.000000000000000000, 0.000000000000000000, -87.50000000000000000 ) ) ;
#6184 = VERTEX_POINT ( 'NONE', #27241 ) ;
#6185 = VERTEX_POINT ( 'NONE', #29121 ) ;
#6186 = DIRECTION ( 'NONE',  ( 0.000000000000000000, 0.000000000000000000, 1.000000000000000000 ) ) ;
#6187 = AXIS2_PLACEMENT_3D ( 'NONE', #20381, #4149, #3849 ) ;
#6188 = CYLINDRICAL_SURFACE ( 'NONE', #23089, 20.00000000000000355 ) ;
#6189 = EDGE_CURVE ( 'NONE', #1222, #2571, #22406, .T. ) ;
#6190 = CARTESIAN_POINT ( 'NONE',  ( 49.99999999999998579, -50.00000000000000000, 59.49999999999999289 ) ) ;
#6191 = ORIENTED_EDGE ( 'NONE', *, *, #2901, .T. ) ;
#6192 = EDGE_CURVE ( 'NONE', #7470, #18090, #5090, .T. ) ;
#6193 = CARTESIAN_POINT ( 'NONE',  ( -33.78553900464347493, 24.40792682089791654, -16.50000000000000000 ) ) ;
#6194 = CARTESIAN_POINT ( 'NONE',  ( 11.11118388262826784, -16.62953976291649028, 18.34798005863226678 ) ) ;
#6195 = EDGE_LOOP ( 'NONE', ( #9343, #21599 ) ) ;
#6196 = ORIENTED_EDGE ( 'NONE', *, *, #19905, .F. ) ;
#6197 = CARTESIAN_POINT ( 'NONE',  ( -19.85166970746585946, 2.573860339590178903, 5.653912893140659257 ) ) ;
#6198 = DIRECTION ( 'NONE',  ( -0.000000000000000000, -0.000000000000000000, 1.000000000000000000 ) ) ;
#6199 = CARTESIAN_POINT ( 'NONE',  ( 15.45572804192159211, 12.69342571624615523, 6.144783687052517429 ) ) ;
#6200 = CARTESIAN_POINT ( 'NONE',  ( -13.58027524052048562, 34.95958275926333414, 37.50000000001884359 ) ) ;
#6201 = ORIENTED_EDGE ( 'NONE', *, *, #17435, .F. ) ;
#6202 = CARTESIAN_POINT ( 'NONE',  ( -12.24063095261064227, 4.490763173670005770, 1.500000000000001332 ) ) ;
#6203 = VERTEX_POINT ( 'NONE', #24283 ) ;
#6204 = CYLINDRICAL_SURFACE ( 'NONE', #5579, 0.7499999999999997780 ) ;
#6205 = CARTESIAN_POINT ( 'NONE',  ( 37.99999999999999289, 209.2686044187655909, -34.50000000000000000 ) ) ;
#6206 = ORIENTED_EDGE ( 'NONE', *, *, #16258, .T. ) ;
#6207 = B_SPLINE_CURVE_WITH_KNOTS ( 'NONE', 3,
 ( #27194, #24382, #22193, #7712 ),
 .UNSPECIFIED., .F., .F.,
 ( 4, 4 ),
 ( 3.018024802580205417E-07, 0.007932103453629116285 ),
 .UNSPECIFIED. ) ;
#6208 = CIRCLE ( 'NONE', #23615, 0.7500000000000002220 ) ;
#6209 = CARTESIAN_POINT ( 'NONE',  ( -27.03074382657074537, 6.449748410230984774, 47.21042702067971675 ) ) ;
#6210 = CARTESIAN_POINT ( 'NONE',  ( 19.50335127913461974, -36.90537731026830670, 29.35045827479529024 ) ) ;
#6211 = CARTESIAN_POINT ( 'NONE',  ( 16.55849529797291098, 4.179294809495486263, 6.447548852708279377 ) ) ;
#6212 = CARTESIAN_POINT ( 'NONE',  ( -13.02951369420309646, 10.96858531083378985, 18.49267272388512140 ) ) ;
#6213 = CARTESIAN_POINT ( 'NONE',  ( -7.870033247355587847, -15.14769711951102771, 19.97651184436794125 ) ) ;
#6214 = CARTESIAN_POINT ( 'NONE',  ( 12.72536390617885438, -2.839914339433650348, 24.50000000000000000 ) ) ;
#6215 = CARTESIAN_POINT ( 'NONE',  ( -19.87987511945007313, 2.346632672767393402, 18.35718225375110180 ) ) ;
#6216 = DIRECTION ( 'NONE',  ( -0.000000000000000000, -0.000000000000000000, 1.000000000000000000 ) ) ;
#6217 = ORIENTED_EDGE ( 'NONE', *, *, #17597, .T. ) ;
#6218 = DIRECTION ( 'NONE',  ( 1.000000000000000000, 0.000000000000000000, 0.000000000000000000 ) ) ;
#6219 = CARTESIAN_POINT ( 'NONE',  ( 34.13832859401787090, 12.80067323710188809, 27.50000000000001066 ) ) ;
#6220 = ORIENTED_EDGE ( 'NONE', *, *, #4412, .T. ) ;
#6221 = VERTEX_POINT ( 'NONE', #21939 ) ;
#6222 = DIRECTION ( 'NONE',  ( 1.000000000000000000, 0.000000000000000000, 0.000000000000000000 ) ) ;
#6223 = CARTESIAN_POINT ( 'NONE',  ( -6.414842543015754295, -17.06554576617236307, 1.500000000000000000 ) ) ;
#6224 = CARTESIAN_POINT ( 'NONE',  ( -5.439684697860721840, 16.15075171424584610, 5.657991946698900598 ) ) ;
#6225 = ORIENTED_EDGE ( 'NONE', *, *, #11907, .F. ) ;
#6226 = DIRECTION ( 'NONE',  ( -0.000000000000000000, -1.000000000000000000, -0.000000000000000000 ) ) ;
#6227 = CARTESIAN_POINT ( 'NONE',  ( -12.33859880789484365, 8.132258305203428961, -16.50000000000000000 ) ) ;
#6228 = EDGE_CURVE ( 'NONE', #29559, #606, #26794, .T. ) ;
#6229 = VECTOR ( 'NONE', #17548, 1000.000000000000000 ) ;
#6230 = DIRECTION ( 'NONE',  ( -0.000000000000000000, -0.000000000000000000, -1.000000000000000000 ) ) ;
#6231 = VERTEX_POINT ( 'NONE', #3074 ) ;
#6232 = DIRECTION ( 'NONE',  ( 0.000000000000000000, 0.000000000000000000, -1.000000000000000000 ) ) ;
#6233 = CARTESIAN_POINT ( 'NONE',  ( 11.85823002435686924, 12.27640118502221256, 5.951255046771932733 ) ) ;
#6234 = CARTESIAN_POINT ( 'NONE',  ( 16.74250592919980818, 3.198927888535953112, 5.652196082367002994 ) ) ;
#6235 = ORIENTED_EDGE ( 'NONE', *, *, #16442, .F. ) ;
#6236 = CARTESIAN_POINT ( 'NONE',  ( 24.03057240117690441, -26.57182937991349903, 1.500000000000001332 ) ) ;
#6237 = ORIENTED_EDGE ( 'NONE', *, *, #29402, .F. ) ;
#6238 = CARTESIAN_POINT ( 'NONE',  ( -14.01114995435608890, 9.765040422203625781, 19.28454053338348473 ) ) ;
#6239 = VERTEX_POINT ( 'NONE', #22087 ) ;
#6240 = ORIENTED_EDGE ( 'NONE', *, *, #1382, .F. ) ;
#6241 = CARTESIAN_POINT ( 'NONE',  ( 3.160432912108486203, 16.77963207014078861, 7.098451512883313441 ) ) ;
#6242 = DIRECTION ( 'NONE',  ( 1.000000000000000000, 0.000000000000000000, 0.000000000000000000 ) ) ;
#6243 = DIRECTION ( 'NONE',  ( 1.000000000000000000, 0.000000000000000000, 0.000000000000000000 ) ) ;
#6244 = ORIENTED_EDGE ( 'NONE', *, *, #14740, .F. ) ;
#6245 = VECTOR ( 'NONE', #8619, 1000.000000000000000 ) ;
#6246 = CARTESIAN_POINT ( 'NONE',  ( -36.00000000000000000, 2.601438916704200466, 34.80090346875804386 ) ) ;
#6247 = CARTESIAN_POINT ( 'NONE',  ( 10.27954044202352968, -17.17695407163359533, 19.11611934778430921 ) ) ;
#6248 = CARTESIAN_POINT ( 'NONE',  ( 35.00000000000000000, 0.000000000000000000, 0.000000000000000000 ) ) ;
#6249 = ORIENTED_EDGE ( 'NONE', *, *, #19476, .F. ) ;
#6250 = CARTESIAN_POINT ( 'NONE',  ( -19.71764211798356925, 3.454211555243456910, 19.66989035740801839 ) ) ;
#6251 = CARTESIAN_POINT ( 'NONE',  ( 17.96497429814991875, -8.830595420483335900, 7.080843742048788414 ) ) ;
#6252 = CARTESIAN_POINT ( 'NONE',  ( -14.00963640524697418, 9.767049959719264152, 6.782048567692550378 ) ) ;
#6253 = CARTESIAN_POINT ( 'NONE',  ( 3.905960108394943564, 16.59621863701447708, 20.33971507717571114 ) ) ;
#6254 = VERTEX_POINT ( 'NONE', #10237 ) ;
#6255 = EDGE_LOOP ( 'NONE', ( #19790, #2644, #10684, #21349 ) ) ;
#6256 = CARTESIAN_POINT ( 'NONE',  ( -30.75232512042845556, -9.966982604840850968, 1.500000000000000000 ) ) ;
#6257 = FACE_OUTER_BOUND ( 'NONE', #26474, .T. ) ;
#6258 = PLANE ( 'NONE',  #29286 ) ;
#6259 = CARTESIAN_POINT ( 'NONE',  ( 12.76326067953069021, 11.27442216563262356, 5.848946451764563292 ) ) ;
#6260 =( NAMED_UNIT ( * ) SI_UNIT ( $, .STERADIAN. ) SOLID_ANGLE_UNIT ( ) );
#6261 = CYLINDRICAL_SURFACE ( 'NONE', #14624, 9.482273699623480212 ) ;
#6262 = AXIS2_PLACEMENT_3D ( 'NONE', #4024, #20993, #14132 ) ;
#6263 = DIRECTION ( 'NONE',  ( 1.000000000000000000, 0.000000000000000000, 0.000000000000000000 ) ) ;
#6264 = CARTESIAN_POINT ( 'NONE',  ( -50.00000000000000000, 70.00000000000000000, 12.49999999999999112 ) ) ;
#6265 = VERTEX_POINT ( 'NONE', #19750 ) ;
#6266 = CARTESIAN_POINT ( 'NONE',  ( -1.000000000000016875, 29.50000000000000000, 1.500000000000001332 ) ) ;
#6267 = CARTESIAN_POINT ( 'NONE',  ( -33.18396177295070260, 9.163667207889121258, 40.57409041144032358 ) ) ;
#6268 = CARTESIAN_POINT ( 'NONE',  ( 39.87350638640939593, 4.706224724266460768, -6.500000000000000888 ) ) ;
#6269 = ORIENTED_EDGE ( 'NONE', *, *, #29385, .F. ) ;
#6270 = AXIS2_PLACEMENT_3D ( 'NONE', #3588, #8122, #12799 ) ;
#6271 = ORIENTED_EDGE ( 'NONE', *, *, #13466, .F. ) ;
#6272 = CARTESIAN_POINT ( 'NONE',  ( 0.000000000000000000, -14.99999999999997158, -55.00000000000000711 ) ) ;
#6273 = CIRCLE ( 'NONE', #3287, 15.00000000000000000 ) ;
#6274 = CARTESIAN_POINT ( 'NONE',  ( 0.4269445148198864892, 2.969464325642835689, 24.50000000000000000 ) ) ;
#6275 = ORIENTED_EDGE ( 'NONE', *, *, #27609, .T. ) ;
#6276 = CARTESIAN_POINT ( 'NONE',  ( -23.27838112031802709, -36.10018649381529343, -16.50000600000000262 ) ) ;
#6277 = DIRECTION ( 'NONE',  ( 0.000000000000000000, -0.000000000000000000, -1.000000000000000000 ) ) ;
#6278 = DIRECTION ( 'NONE',  ( -0.000000000000000000, -0.000000000000000000, -1.000000000000000000 ) ) ;
#6279 = CARTESIAN_POINT ( 'NONE',  ( 24.03057240117691862, 26.57182937991349903, -1.500000000000000000 ) ) ;
#6280 = FACE_OUTER_BOUND ( 'NONE', #10225, .T. ) ;
#6281 = AXIS2_PLACEMENT_3D ( 'NONE', #13357, #11472, #11166 ) ;
#6282 = CARTESIAN_POINT ( 'NONE',  ( 0.000000000000000000, -5.590849009245238754, 1.500000000000000000 ) ) ;
#6283 = CARTESIAN_POINT ( 'NONE',  ( -4.163336342344337027E-14, -1.387778780781445676E-14, -1.500000000000000000 ) ) ;
#6284 = CARTESIAN_POINT ( 'NONE',  ( -16.81375614428661791, 2.649924382790501021, 6.519181285484531685 ) ) ;
#6285 = VERTEX_POINT ( 'NONE', #29280 ) ;
#6286 = AXIS2_PLACEMENT_3D ( 'NONE', #10030, #19537, #12530 ) ;
#6287 = DIRECTION ( 'NONE',  ( -0.000000000000000000, -1.000000000000000000, -0.000000000000000000 ) ) ;
#6288 = CARTESIAN_POINT ( 'NONE',  ( 52.16608720827707657, 51.86186943028246787, 97.07879600563551037 ) ) ;
#6289 = CARTESIAN_POINT ( 'NONE',  ( -5.419526071979801074, 16.15737324486737947, 7.652108011868851811 ) ) ;
#6290 = AXIS2_PLACEMENT_3D ( 'NONE', #11662, #23810, #18997 ) ;
#6291 = CARTESIAN_POINT ( 'NONE',  ( -18.05883735157482661, -8.636530476581221194, 18.34798005862662507 ) ) ;
#6292 = B_SPLINE_CURVE_WITH_KNOTS ( 'NONE', 3,
 ( #15709, #30063, #8703, #25225 ),
 .UNSPECIFIED., .F., .F.,
 ( 4, 4 ),
 ( 3.018024802580205417E-07, 0.007932103453629112816 ),
 .UNSPECIFIED. ) ;
#6293 = AXIS2_PLACEMENT_3D ( 'NONE', #17415, #21925, #19588 ) ;
#6294 = CARTESIAN_POINT ( 'NONE',  ( -39.00000000000000000, -5.563236990218529243, -1.500000000000000000 ) ) ;
#6295 = CARTESIAN_POINT ( 'NONE',  ( -23.16753609997193664, 35.74416776803685281, -13.16661218272965783 ) ) ;
#6296 = EDGE_CURVE ( 'NONE', #23760, #14253, #4364, .T. ) ;
#6297 = ORIENTED_EDGE ( 'NONE', *, *, #23476, .T. ) ;
#6298 = DIRECTION ( 'NONE',  ( -0.000000000000000000, 0.000000000000000000, 1.000000000000000000 ) ) ;
#6299 = CARTESIAN_POINT ( 'NONE',  ( -2.552544030762004645, -42.50000000000000000, -1.500000000000000000 ) ) ;
#6300 = CARTESIAN_POINT ( 'NONE',  ( 16.58685200597968290, -38.49307988151863213, 29.20042932998627094 ) ) ;
#6301 = EDGE_CURVE ( 'NONE', #11660, #1290, #28174, .T. ) ;
#6302 = DIRECTION ( 'NONE',  ( 0.000000000000000000, -1.132880637372608986E-16, 1.000000000000000000 ) ) ;
#6303 = ORIENTED_EDGE ( 'NONE', *, *, #13371, .T. ) ;
#6304 = DIRECTION ( 'NONE',  ( -0.000000000000000000, -0.000000000000000000, 1.000000000000000000 ) ) ;
#6305 = CARTESIAN_POINT ( 'NONE',  ( 13.22505861668094340, 42.10773672057246841, -19.50000000000000355 ) ) ;
#6306 = CARTESIAN_POINT ( 'NONE',  ( -9.269489102446176076, -14.27959628656686597, 6.111214848085761986 ) ) ;
#6307 = AXIS2_PLACEMENT_3D ( 'NONE', #23730, #3005, #14388 ) ;
#6308 = ORIENTED_EDGE ( 'NONE', *, *, #23292, .T. ) ;
#6309 = EDGE_CURVE ( 'NONE', #29624, #18134, #20826, .T. ) ;
#6310 = CARTESIAN_POINT ( 'NONE',  ( -23.36057818983817924, -12.54850586925978284, 48.48255250177239617 ) ) ;
#6311 = DIRECTION ( 'NONE',  ( 0.000000000000000000, 1.000000000000000000, 1.193512090021232842E-16 ) ) ;
#6312 = ORIENTED_EDGE ( 'NONE', *, *, #3093, .T. ) ;
#6313 = CARTESIAN_POINT ( 'NONE',  ( 23.27838111857050407, -36.10018641471199174, -16.50000599999999906 ) ) ;
#6315 = EDGE_CURVE ( 'NONE', #7923, #10711, #13524, .T. ) ;
#6314 = VECTOR ( 'NONE', #9388, 1000.000000000000000 ) ;
#6316 = CARTESIAN_POINT ( 'NONE',  ( -24.44496207165490276, -7.595930209050158588, -16.55003854064094426 ) ) ;
#6317 = VECTOR ( 'NONE', #8954, 1000.000000000000000 ) ;
#6318 = CARTESIAN_POINT ( 'NONE',  ( 3.914781618004695929, 8.197313248159961319, -1.500000000000000888 ) ) ;
#6319 = CARTESIAN_POINT ( 'NONE',  ( 0.3541522971493302196, -20.01464067411590264, 18.34798005862662507 ) ) ;
#6320 = ORIENTED_EDGE ( 'NONE', *, *, #1153, .F. ) ;
#6321 = CARTESIAN_POINT ( 'NONE',  ( 11.65972768484889954, 12.47873923859708079, 19.47952243369111258 ) ) ;
#6322 = DIRECTION ( 'NONE',  ( -0.000000000000000000, 1.132880637372608986E-16, -1.000000000000000000 ) ) ;
#6323 = DIRECTION ( 'NONE',  ( -0.000000000000000000, 0.000000000000000000, 1.000000000000000000 ) ) ;
#6324 = CARTESIAN_POINT ( 'NONE',  ( 46.99999999999998579, 90.00000000000001421, 52.49999999999999289 ) ) ;
#6325 = CARTESIAN_POINT ( 'NONE',  ( -15.52789627656017224, -6.978352780261414701, 19.85270094495842486 ) ) ;
#6326 = CARTESIAN_POINT ( 'NONE',  ( 26.36764545593179676, 31.31467416275351923, -1.500000000000000000 ) ) ;
#6327 = DIRECTION ( 'NONE',  ( 0.000000000000000000, 0.8660254037844382635, -0.5000000000000006661 ) ) ;
#6328 = DIRECTION ( 'NONE',  ( 0.9594929736144974797, -0.2817325568414297265, 0.000000000000000000 ) ) ;
#6329 = ADVANCED_FACE ( 'NONE', ( #23005 ), #11173, .F. ) ;
#6330 = EDGE_CURVE ( 'NONE', #22249, #540, #7613, .T. ) ;
#6331 = EDGE_CURVE ( 'NONE', #20319, #2261, #20670, .T. ) ;
#6332 = CARTESIAN_POINT ( 'NONE',  ( 9.118789845666759319, -14.37574228026362988, 6.143977687428010093 ) ) ;
#6333 = CARTESIAN_POINT ( 'NONE',  ( -9.369089179316107519, -14.21146650728099381, 19.60617949693493856 ) ) ;
#6334 = AXIS2_PLACEMENT_3D ( 'NONE', #26539, #7364, #14373 ) ;
#6335 = ORIENTED_EDGE ( 'NONE', *, *, #11073, .F. ) ;
#6336 = EDGE_CURVE ( 'NONE', #7694, #26229, #6612, .T. ) ;
#6337 = ORIENTED_EDGE ( 'NONE', *, *, #12052, .F. ) ;
#6338 = AXIS2_PLACEMENT_3D ( 'NONE', #21928, #557, #10077 ) ;
#6339 = DIRECTION ( 'NONE',  ( 0.1423148382732889461, 0.9898214418809321291, 0.000000000000000000 ) ) ;
#6340 = CARTESIAN_POINT ( 'NONE',  ( -13.68208811019134785, -10.53240720452297374, 1.500000000000000000 ) ) ;
#6341 = PLANE ( 'NONE',  #22365 ) ;
#6342 = EDGE_CURVE ( 'NONE', #7128, #281, #4145, .T. ) ;
#6343 = ORIENTED_EDGE ( 'NONE', *, *, #21967, .T. ) ;
#6344 =( NAMED_UNIT ( * ) SI_UNIT ( $, .STERADIAN. ) SOLID_ANGLE_UNIT ( ) );
#6345 = AXIS2_PLACEMENT_3D ( 'NONE', #10278, #21979, #19957 ) ;
#6346 = DIRECTION ( 'NONE',  ( 0.000000000000000000, -1.000000000000000000, 0.000000000000000000 ) ) ;
#6347 = DIRECTION ( 'NONE',  ( -1.000000000000000000, 0.000000000000000000, 0.000000000000000000 ) ) ;
#6348 = ADVANCED_FACE ( 'NONE', ( #23159 ), #13209, .T. ) ;
#6349 = ADVANCED_FACE ( 'NONE', ( #1202 ), #24904, .F. ) ;
#6350 = ORIENTED_EDGE ( 'NONE', *, *, #13012, .F. ) ;
#6351 = EDGE_LOOP ( 'NONE', ( #2530, #13783, #8315, #56, #1126, #30652, #565, #30623, #28984, #197, #7390, #13612, #25640, #20397, #1083, #13098, #8215, #1676, #26864, #777, #30251, #20777, #759, #6029, #10352, #20885, #18447, #8992, #3076, #28564, #13195, #19452, #4351, #17913, #20629, #20500, #2246, #6133, #26132, #9168, #3955, #15267, #26335, #28977, #24268, #20534, #29212, #14479, #12323, #26645, #11536, #16061, #28300, #29913, #7360, #3255, #16934, #17039, #84, #4215, #28043, #2160, #12284, #23345, #29390, #10462, #16670, #27598, #17689, #28149, #24749, #5939, #8617, #10057, #5987, #26763, #15662, #24701, #14294, #25511, #24121, #10588, #25111 ) ) ;
#6352 = CARTESIAN_POINT ( 'NONE',  ( -16.85109579167143679, 2.433552959544808658, 6.018569869498933578 ) ) ;
#6353 = CIRCLE ( 'NONE', #29779, 9.084132297865673777 ) ;
#6354 = DIRECTION ( 'NONE',  ( 0.000000000000000000, 1.132880637372608986E-16, -1.000000000000000000 ) ) ;
#6355 = CARTESIAN_POINT ( 'NONE',  ( -1.045628782875250185, -44.07656352898515451, -16.50000000000000000 ) ) ;
#6356 = CARTESIAN_POINT ( 'NONE',  ( 2.261640607880582632, 42.53980470135267211, 28.83615268921961672 ) ) ;
#6357 = VERTEX_POINT ( 'NONE', #15685 ) ;
#6358 = CARTESIAN_POINT ( 'NONE',  ( -1.073881485057738949, -0.9711784013061123266, 1.500000000000000000 ) ) ;
#6359 = ORIENTED_EDGE ( 'NONE', *, *, #17938, .T. ) ;
#6360 = AXIS2_PLACEMENT_3D ( 'NONE', #14982, #21851, #5166 ) ;
#6361 = CARTESIAN_POINT ( 'NONE',  ( -14.76455652122660211, -8.574248774020551522, 6.147510495896840510 ) ) ;
#6362 = FACE_OUTER_BOUND ( 'NONE', #14584, .T. ) ;
#6363 = EDGE_LOOP ( 'NONE', ( #30767, #20212, #3852, #420 ) ) ;
#6364 = CIRCLE ( 'NONE', #26278, 1.447898107987198646 ) ;
#6365 = CIRCLE ( 'NONE', #26279, 1.000000000000004441 ) ;
#6366 = CARTESIAN_POINT ( 'NONE',  ( 16.83292851409026980, 2.581421006622409031, 20.14907003336613300 ) ) ;
#6367 = DIRECTION ( 'NONE',  ( -1.000000000000000000, 0.000000000000000000, 0.000000000000000000 ) ) ;
#6368 = ADVANCED_FACE ( 'NONE', ( #13368 ), #11021, .F. ) ;
#6369 = PLANE ( 'NONE',  #9618 ) ;
#6370 = DIRECTION ( 'NONE',  ( -0.000000000000000000, -0.000000000000000000, -1.000000000000000000 ) ) ;
#6371 = AXIS2_PLACEMENT_3D ( 'NONE', #19909, #29423, #27077 ) ;
#6372 = CARTESIAN_POINT ( 'NONE',  ( 1.788804076111017549, -16.98411955790531991, 6.521906765011497242 ) ) ;
#6373 = CARTESIAN_POINT ( 'NONE',  ( -16.96556290498877573, 1.647560670993253540, 18.34798005863078885 ) ) ;
#6374 = CARTESIAN_POINT ( 'NONE',  ( 1.073881485057758711, 0.9711784013061475207, -1.500000000000000000 ) ) ;
#6375 = CYLINDRICAL_SURFACE ( 'NONE', #16367, 0.7500000000000011102 ) ;
#6376 = ORIENTED_EDGE ( 'NONE', *, *, #19964, .F. ) ;
#6377 = EDGE_CURVE ( 'NONE', #17660, #26457, #26119, .T. ) ;
#6378 = VECTOR ( 'NONE', #16777, 1000.000000000000000 ) ;
#6379 = EDGE_CURVE ( 'NONE', #25657, #6669, #2579, .T. ) ;
#6380 = CARTESIAN_POINT ( 'NONE',  ( -29.78995557804746497, 27.43027642362437390, 16.84702627303446221 ) ) ;
#6381 = CARTESIAN_POINT ( 'NONE',  ( 34.13832859401787090, 12.80067323710188809, 34.80090346875810070 ) ) ;
#6382 = VERTEX_POINT ( 'NONE', #14251 ) ;
#6383 = ORIENTED_EDGE ( 'NONE', *, *, #1790, .T. ) ;
#6384 = CARTESIAN_POINT ( 'NONE',  ( 39.99999999999998579, 67.32050807568877815, 12.49999999999999112 ) ) ;
#6385 = FACE_OUTER_BOUND ( 'NONE', #25780, .T. ) ;
#6386 = CARTESIAN_POINT ( 'NONE',  ( 0.000000000000000000, 0.000000000000000000, 82.49999999999998579 ) ) ;
#6387 = ORIENTED_EDGE ( 'NONE', *, *, #25009, .T. ) ;
#6388 = LINE ( 'NONE', #13566, #20051 ) ;
#6389 = CIRCLE ( 'NONE', #30773, 9.084132297865673777 ) ;
#6390 = CARTESIAN_POINT ( 'NONE',  ( -13.05132497920473611, 10.94401179279875969, 5.774779864094943704 ) ) ;
#6391 = AXIS2_PLACEMENT_3D ( 'NONE', #6593, #15958, #16247 ) ;
#6392 = CARTESIAN_POINT ( 'NONE',  ( -4.163336342344337027E-14, 1.387778780781445676E-14, 62.49999999999999289 ) ) ;
#6393 = ORIENTED_EDGE ( 'NONE', *, *, #25579, .T. ) ;
#6394 = CARTESIAN_POINT ( 'NONE',  ( -33.54152001338305666, -10.01313039630840152, 39.99603010802629655 ) ) ;
#6395 = EDGE_LOOP ( 'NONE', ( #12597, #22084, #27133, #10403 ) ) ;
#6396 = CARTESIAN_POINT ( 'NONE',  ( 0.000000000000000000, 0.000000000000000000, 1.500000000000001332 ) ) ;
#6397 = ORIENTED_EDGE ( 'NONE', *, *, #9642, .T. ) ;
#6398 = AXIS2_PLACEMENT_3D ( 'NONE', #3119, #12639, #22132 ) ;
#6399 = LINE ( 'NONE', #25576, #20887 ) ;
#6400 = ORIENTED_EDGE ( 'NONE', *, *, #12419, .T. ) ;
#6401 = ORIENTED_EDGE ( 'NONE', *, *, #22169, .T. ) ;
#6402 = CARTESIAN_POINT ( 'NONE',  ( 3.085425824774463255, 16.79642356368105283, 6.892848776733236704 ) ) ;
#6403 = EDGE_CURVE ( 'NONE', #16254, #4466, #30637, .T. ) ;
#6404 = DIRECTION ( 'NONE',  ( 0.000000000000000000, 0.000000000000000000, -1.000000000000000000 ) ) ;
#6405 = CARTESIAN_POINT ( 'NONE',  ( -17.22181377296915272, -14.41708049311147555, 1.500000000000000000 ) ) ;
#6406 = ADVANCED_FACE ( 'NONE', ( #7101 ), #4459, .F. ) ;
#6407 = ORIENTED_EDGE ( 'NONE', *, *, #6693, .T. ) ;
#6408 = AXIS2_PLACEMENT_3D ( 'NONE', #8166, #15477, #5665 ) ;
#6409 = CARTESIAN_POINT ( 'NONE',  ( 10.92986663323816465, -16.77091174116444350, 18.36582235739946611 ) ) ;
#6410 = CARTESIAN_POINT ( 'NONE',  ( 30.26724724045341119, 27.72993536918018265, -6.500000000000000888 ) ) ;
#6411 = ORIENTED_EDGE ( 'NONE', *, *, #16063, .F. ) ;
#6412 = CARTESIAN_POINT ( 'NONE',  ( 37.99999999999999289, 209.2686044187655909, -75.50000000000001421 ) ) ;
#6413 = FACE_OUTER_BOUND ( 'NONE', #18578, .T. ) ;
#6414 = CARTESIAN_POINT ( 'NONE',  ( -13.98072106069837517, 9.805336070574281138, 6.341840715582230281 ) ) ;
#6415 = CARTESIAN_POINT ( 'NONE',  ( 3.122919890997783110, 16.78802993858287707, 19.69140814234746273 ) ) ;
#6416 = ORIENTED_EDGE ( 'NONE', *, *, #24246, .T. ) ;
#6417 = ORIENTED_EDGE ( 'NONE', *, *, #907, .T. ) ;
#6418 = DIRECTION ( 'NONE',  ( 0.000000000000000000, -0.4961389383568337030, 0.8682431421244592995 ) ) ;
#6419 = PRODUCT_DEFINITION_FORMATION_WITH_SPECIFIED_SOURCE ( 'ANY', '', #21363, .NOT_KNOWN. ) ;
#6420 = CARTESIAN_POINT ( 'NONE',  ( 16.79415820840736728, -38.40031270401642871, 23.10897800509315658 ) ) ;
#6421 = CARTESIAN_POINT ( 'NONE',  ( 12.35522425158189108, 11.74279415389956505, 5.652196082368482699 ) ) ;
#6422 = DIRECTION ( 'NONE',  ( 1.000000000000000000, 0.000000000000000000, 0.000000000000000000 ) ) ;
#6423 = VECTOR ( 'NONE', #26742, 1000.000000000000000 ) ;
#6424 = CARTESIAN_POINT ( 'NONE',  ( -2.516121109503243414, -8.728722367416578365, 13.22130136205108641 ) ) ;
#6425 = CIRCLE ( 'NONE', #2435, 9.482273699623480212 ) ;
#6426 = CIRCLE ( 'NONE', #8442, 4.999999999999997335 ) ;
#6427 = CYLINDRICAL_SURFACE ( 'NONE', #6902, 0.7500000000000002220 ) ;
#6428 = CARTESIAN_POINT ( 'NONE',  ( 23.94669763007064134, -13.17250946182262972, 47.66948656108987592 ) ) ;
#6429 = ORIENTED_EDGE ( 'NONE', *, *, #30719, .T. ) ;
#6430 = CARTESIAN_POINT ( 'NONE',  ( 0.9770435002939149571, -19.97634058022567771, 5.853797745100181693 ) ) ;
#6431 = AXIS2_PLACEMENT_3D ( 'NONE', #28012, #6497, #23163 ) ;
#6432 = CYLINDRICAL_SURFACE ( 'NONE', #8235, 0.7499999999999997780 ) ;
#6433 = CARTESIAN_POINT ( 'NONE',  ( 0.000000000000000000, 0.000000000000000000, 1.500000000000001332 ) ) ;
#6434 = VERTEX_POINT ( 'NONE', #2422 ) ;
#6435 = DIRECTION ( 'NONE',  ( 0.000000000000000000, -1.132880637372608986E-16, 1.000000000000000000 ) ) ;
#6436 = EDGE_LOOP ( 'NONE', ( #30599, #14041 ) ) ;
#6437 = CARTESIAN_POINT ( 'NONE',  ( -19.80980381183503525, 2.754394816484158515, 5.676722608126683056 ) ) ;
#6438 = UNCERTAINTY_MEASURE_WITH_UNIT (LENGTH_MEASURE( 1.000000000000000082E-05 ), #1443, 'distance_accuracy_value', 'NONE');
#6439 = MECHANICAL_DESIGN_GEOMETRIC_PRESENTATION_REPRESENTATION (  '', ( #19881 ), #14397 ) ;
#6440 = DIRECTION ( 'NONE',  ( 0.000000000000000000, 0.000000000000000000, 1.000000000000000000 ) ) ;
#6441 = ORIENTED_EDGE ( 'NONE', *, *, #4973, .F. ) ;
#6442 = CARTESIAN_POINT ( 'NONE',  ( -0.6573828633908590513, -19.98919327533015533, 6.781503518395075147 ) ) ;
#6443 = CARTESIAN_POINT ( 'NONE',  ( 7.522556813806144937, 49.43282481825458774, -67.98671092651753156 ) ) ;
#6444 = CARTESIAN_POINT ( 'NONE',  ( -4.776122516674677878E-15, -42.50000000000000000, 19.72227980406325543 ) ) ;
#6445 = CARTESIAN_POINT ( 'NONE',  ( -37.16608720827707657, 65.00000000000000000, 97.07879600563551037 ) ) ;
#6446 = CARTESIAN_POINT ( 'NONE',  ( -33.42925964089140933, 11.06161099612212695, 35.54550565580014876 ) ) ;
#6447 = VECTOR ( 'NONE', #25194, 1000.000000000000000 ) ;
#6448 = EDGE_CURVE ( 'NONE', #9580, #15627, #24524, .T. ) ;
#6449 = CARTESIAN_POINT ( 'NONE',  ( -24.03057240117691862, 26.57182937991349903, 1.500000000000000000 ) ) ;
#6450 = DIRECTION ( 'NONE',  ( 0.000000000000000000, 1.000000000000000000, 0.000000000000000000 ) ) ;
#6451 = CARTESIAN_POINT ( 'NONE',  ( -16.96556290498877573, 1.647560670993253540, 5.652196082368482699 ) ) ;
#6452 = EDGE_LOOP ( 'NONE', ( #10370, #3859, #2915, #19681 ) ) ;
#6453 = CARTESIAN_POINT ( 'NONE',  ( 0.000000000000000000, 0.000000000000000000, 0.000000000000000000 ) ) ;
#6454 = VECTOR ( 'NONE', #5967, 1000.000000000000000 ) ;
#6455 = CARTESIAN_POINT ( 'NONE',  ( 0.000000000000000000, -2.435693370351110282E-15, 21.50000000000000355 ) ) ;
#6456 = CARTESIAN_POINT ( 'NONE',  ( 6.543385983536345485, 6.301234758012618009, 21.50000000000000000 ) ) ;
#6457 = DIRECTION ( 'NONE',  ( 1.000000000000000000, 0.000000000000000000, 0.000000000000000000 ) ) ;
#6458 = CARTESIAN_POINT ( 'NONE',  ( -15.01497154418443891, -8.089954645606729500, 18.39992786714538298 ) ) ;
#6459 = CARTESIAN_POINT ( 'NONE',  ( 0.5590800469813657081, 9.968355046870088998, 0.7343025909353930736 ) ) ;
#6460 = CIRCLE ( 'NONE', #2469, 9.000000000000000000 ) ;
#6461 = DIRECTION ( 'NONE',  ( -0.000000000000000000, 0.000000000000000000, 1.000000000000000000 ) ) ;
#6462 = ORIENTED_EDGE ( 'NONE', *, *, #12893, .T. ) ;
#6463 = CARTESIAN_POINT ( 'NONE',  ( -0.5282983270408734278, -19.99308596983832587, 18.84056766331481825 ) ) ;
#6464 = PLANE ( 'NONE',  #2684 ) ;
#6465 = CARTESIAN_POINT ( 'NONE',  ( 20.12759350631650079, -36.43173182286896150, 29.39766878516364912 ) ) ;
#6466 = DIRECTION ( 'NONE',  ( -0.000000000000000000, -0.000000000000000000, -1.000000000000000000 ) ) ;
#6467 = ORIENTED_EDGE ( 'NONE', *, *, #5564, .T. ) ;
#6468 = CARTESIAN_POINT ( 'NONE',  ( -39.83602371821034183, 11.57901747687032490, -19.50000000000000355 ) ) ;
#6469 = DIRECTION ( 'NONE',  ( -1.000000000000000000, 0.000000000000000000, 0.000000000000000000 ) ) ;
#6470 = ORIENTED_EDGE ( 'NONE', *, *, #24313, .T. ) ;
#6471 = VECTOR ( 'NONE', #6618, 1000.000000000000000 ) ;
#6472 = CARTESIAN_POINT ( 'NONE',  ( -22.65044984052701338, -34.60503960346625263, 29.57823825362870807 ) ) ;
#6473 = EDGE_CURVE ( 'NONE', #4214, #16129, #20054, .T. ) ;
#6474 = ORIENTED_EDGE ( 'NONE', *, *, #14850, .F. ) ;
#6475 = CARTESIAN_POINT ( 'NONE',  ( -31.89119714134806927, -14.79609055705960863, 39.84392849735367292 ) ) ;
#6476=STYLED_ITEM('',(#30914),#12830);
#6477 = LINE ( 'NONE', #8814, #27739 ) ;
#6478 = FACE_OUTER_BOUND ( 'NONE', #30530, .T. ) ;
#6479 = ORIENTED_EDGE ( 'NONE', *, *, #395, .F. ) ;
#6480 = CARTESIAN_POINT ( 'NONE',  ( 11.75084321055936520, 12.38658771204268128, 18.84329447212444109 ) ) ;
#6481 = LINE ( 'NONE', #28146, #29833 ) ;
#6482 = LINE ( 'NONE', #3992, #14210 ) ;
#6483 = EDGE_CURVE ( 'NONE', #17576, #8468, #20966, .T. ) ;
#6484 = DIRECTION ( 'NONE',  ( -1.000000000000000000, -0.000000000000000000, -0.000000000000000000 ) ) ;
#6485 = CARTESIAN_POINT ( 'NONE',  ( 31.29501345866090389, 26.27841684422296353, -6.500000000000000888 ) ) ;
#6486 = CARTESIAN_POINT ( 'NONE',  ( -4.163336342344337027E-14, 1.387778780781445676E-14, 67.49999999999997158 ) ) ;
#6487 = CARTESIAN_POINT ( 'NONE',  ( -6.778663211761418061, 6.630478080506979843, 13.00000000000000178 ) ) ;
#6488 = CARTESIAN_POINT ( 'NONE',  ( -18.15587082468813307, -8.389233089038011570, 20.32243167357988156 ) ) ;
#6489 = DIRECTION ( 'NONE',  ( -0.5406408174555976665, 0.8412535328311810945, 0.000000000000000000 ) ) ;
#6490 = AXIS2_PLACEMENT_3D ( 'NONE', #4842, #4690, #11877 ) ;
#6491 = CARTESIAN_POINT ( 'NONE',  ( 35.78163722268750746, -27.43648963448195133, -1.500000000000000000 ) ) ;
#6492 = ORIENTED_EDGE ( 'NONE', *, *, #25807, .F. ) ;
#6493 = ORIENTED_EDGE ( 'NONE', *, *, #26799, .F. ) ;
#6494 = EDGE_CURVE ( 'NONE', #12057, #7501, #21061, .T. ) ;
#6495 = CARTESIAN_POINT ( 'NONE',  ( -50.00000000000000000, 50.00000000000000000, 59.49999999999999289 ) ) ;
#6496 = CARTESIAN_POINT ( 'NONE',  ( 5.374868878254059013, -44.10336124695543703, -19.50000000000000355 ) ) ;
#6497 = DIRECTION ( 'NONE',  ( -0.000000000000000000, -0.000000000000000000, 1.000000000000000000 ) ) ;
#6498 = ORIENTED_EDGE ( 'NONE', *, *, #26501, .T. ) ;
#6499 = CARTESIAN_POINT ( 'NONE',  ( 0.000000000000000000, 0.000000000000000000, 0.000000000000000000 ) ) ;
#6500 = CARTESIAN_POINT ( 'NONE',  ( 22.94541271838008356, -35.03073867843704647, -6.500000000000000888 ) ) ;
#6501 = CIRCLE ( 'NONE', #27374, 12.66227964008302287 ) ;
#6502 = LINE ( 'NONE', #16011, #3744 ) ;
#6503 = ORIENTED_EDGE ( 'NONE', *, *, #7707, .T. ) ;
#6504 = CARTESIAN_POINT ( 'NONE',  ( -19.74686063004095971, 3.283826233409512074, 6.018569869498933578 ) ) ;
#6505 = ADVANCED_FACE ( 'NONE', ( #19106 ), #30800, .T. ) ;
#6506 = CARTESIAN_POINT ( 'NONE',  ( 14.96781329949620698, 13.26582956964654159, 5.651480102388687143 ) ) ;
#6507 = CARTESIAN_POINT ( 'NONE',  ( -8.682310844383327009, 41.46098991953741120, 34.58670143013237919 ) ) ;
#6508 = ORIENTED_EDGE ( 'NONE', *, *, #1182, .T. ) ;
#6509 = DIRECTION ( 'NONE',  ( 0.000000000000000000, 0.5000000000000015543, -0.8660254037844378194 ) ) ;
#6510 = EDGE_CURVE ( 'NONE', #2261, #2130, #9175, .T. ) ;
#6511 = ORIENTED_EDGE ( 'NONE', *, *, #21639, .F. ) ;
#6512 = EDGE_CURVE ( 'NONE', #30374, #9285, #18084, .T. ) ;
#6513 = CARTESIAN_POINT ( 'NONE',  ( -33.42925964089141644, -11.06161099612212695, -16.55003854064094426 ) ) ;
#6514 = AXIS2_PLACEMENT_3D ( 'NONE', #2012, #13575, #13717 ) ;
#6515 = DIRECTION ( 'NONE',  ( 0.000000000000000000, -0.000000000000000000, -1.000000000000000000 ) ) ;
#6516 = ORIENTED_EDGE ( 'NONE', *, *, #28292, .T. ) ;
#6517 = CARTESIAN_POINT ( 'NONE',  ( 26.81381729043378570, -6.366069288663354087, 43.19821070580849920 ) ) ;
#6518 = ADVANCED_FACE ( 'NONE', ( #23321 ), #28325, .F. ) ;
#6519 = DIRECTION ( 'NONE',  ( 0.000000000000000000, 0.000000000000000000, 1.000000000000000000 ) ) ;
#6520 = CARTESIAN_POINT ( 'NONE',  ( 0.6650193650332598683, -17.02944248263315785, 7.652108011868850035 ) ) ;
#6521 = EDGE_CURVE ( 'NONE', #18778, #438, #603, .T. ) ;
#6522 = DIRECTION ( 'NONE',  ( -0.000000000000000000, 1.132880637372608986E-16, -1.000000000000000000 ) ) ;
#6523 = DIRECTION ( 'NONE',  ( 0.000000000000000000, 0.000000000000000000, 1.000000000000000000 ) ) ;
#6524 = CARTESIAN_POINT ( 'NONE',  ( -8.975220329042338463, -14.47597657772618085, 5.774779864094944593 ) ) ;
#6525 = CARTESIAN_POINT ( 'NONE',  ( 14.87898187659696170, 13.36471393577513389, 5.652196082369963293 ) ) ;
#6526 = ORIENTED_EDGE ( 'NONE', *, *, #10961, .F. ) ;
#6527 = EDGE_CURVE ( 'NONE', #10056, #18778, #2094, .T. ) ;
#6528 = FACE_OUTER_BOUND ( 'NONE', #14522, .T. ) ;
#6529 = CARTESIAN_POINT ( 'NONE',  ( 32.31576317091161599, -17.59561277345965280, 34.80090346875809360 ) ) ;
#6530 = EDGE_CURVE ( 'NONE', #7224, #20725, #10204, .T. ) ;
#6531 = ORIENTED_EDGE ( 'NONE', *, *, #16033, .F. ) ;
#6532 = EDGE_LOOP ( 'NONE', ( #22804, #521, #30469, #26719 ) ) ;
#6533 = ADVANCED_FACE ( 'NONE', ( #17386 ), #21742, .T. ) ;
#6534 = LINE ( 'NONE', #22744, #12654 ) ;
#6535 = VECTOR ( 'NONE', #15957, 1000.000000000000000 ) ;
#6536 = CARTESIAN_POINT ( 'NONE',  ( -5.128149923613393391, 16.24357618101655021, 5.749228751562096562 ) ) ;
#6537 = ORIENTED_EDGE ( 'NONE', *, *, #4468, .T. ) ;
#6538 = CARTESIAN_POINT ( 'NONE',  ( 37.99999999999999289, 70.00000000000000000, -34.50000000000000000 ) ) ;
#6539 = CARTESIAN_POINT ( 'NONE',  ( 0.000000000000000000, 1.699320956058915452E-16, -1.500000000000001776 ) ) ;
#6540 = ORIENTED_EDGE ( 'NONE', *, *, #16064, .F. ) ;
#6541 = CARTESIAN_POINT ( 'NONE',  ( 0.000000000000000000, 0.000000000000000000, 21.50000000000000000 ) ) ;
#6542 = DIRECTION ( 'NONE',  ( 2.312964634635740689E-15, 1.000000000000000000, 0.000000000000000000 ) ) ;
#6543 = ORIENTED_EDGE ( 'NONE', *, *, #14321, .F. ) ;
#6544 = DIRECTION ( 'NONE',  ( -0.000000000000000000, 1.132880637372608986E-16, -1.000000000000000000 ) ) ;
#6545 = ADVANCED_FACE ( 'NONE', ( #7878 ), #533, .F. ) ;
#6546 = ORIENTED_EDGE ( 'NONE', *, *, #17599, .F. ) ;
#6547 = CARTESIAN_POINT ( 'NONE',  ( 22.95669091611932089, -27.54300778121948312, -1.500000000000000000 ) ) ;
#6548 = EDGE_CURVE ( 'NONE', #3169, #26376, #14885, .T. ) ;
#6549 = VERTEX_POINT ( 'NONE', #687 ) ;
#6550 = EDGE_CURVE ( 'NONE', #10235, #19317, #10055, .T. ) ;
#6551 = ORIENTED_EDGE ( 'NONE', *, *, #25767, .T. ) ;
#6552 = EDGE_CURVE ( 'NONE', #18859, #1513, #24234, .T. ) ;
#6553 = CYLINDRICAL_SURFACE ( 'NONE', #24099, 0.6002263538043630664 ) ;
#6554 = CARTESIAN_POINT ( 'NONE',  ( 0.1469846612282587339, -8.891930899535442023, -2.598723904613021496 ) ) ;
#6555 = ORIENTED_EDGE ( 'NONE', *, *, #2132, .T. ) ;
#6556 = B_SPLINE_CURVE_WITH_KNOTS ( 'NONE', 3,
 ( #18209, #8398, #1527, #22567, #25067, #10884, #27573, #13688, #20843, #20395, #3864, #6199, #13386, #9006, #18374, #17911, #6506, #27425 ),
 .UNSPECIFIED., .F., .F.,
 ( 4, 2, 2, 2, 2, 2, 2, 2, 4 ),
 ( 0.003174295595554300041, 0.003570702171545529768, 0.003967108747536759496, 0.004363515323527989223, 0.004759921899519219818, 0.005156328475510448678, 0.005552735051501679273, 0.005949141627492909000, 0.006345548203484138727 ),
 .UNSPECIFIED. ) ;
#6557 = AXIS2_PLACEMENT_3D ( 'NONE', #27701, #6327, #3995 ) ;
#6558 = CARTESIAN_POINT ( 'NONE',  ( 10.44969336715137409, -17.07413037334559647, 18.71435384576123440 ) ) ;
#6559 = CARTESIAN_POINT ( 'NONE',  ( -16.96556290498877573, 1.647560670993253540, 18.34798005863078885 ) ) ;
#6560 = EDGE_LOOP ( 'NONE', ( #6588, #1450, #25113, #17142, #21470, #5154, #22451, #5060, #2308 ) ) ;
#6561 = EDGE_CURVE ( 'NONE', #16378, #17362, #19714, .T. ) ;
#6562 = CARTESIAN_POINT ( 'NONE',  ( -16.81358047026920843, 2.650995224496061287, 19.45164628100866722 ) ) ;
#6563 = CARTESIAN_POINT ( 'NONE',  ( 18.25868057198135830, -8.206406842115287148, 7.632642797338977658 ) ) ;
#6564 = CARTESIAN_POINT ( 'NONE',  ( -13.95039892200172105, 9.845341970609696958, 7.098451512883313441 ) ) ;
#6565 = CARTESIAN_POINT ( 'NONE',  ( 3.971879806607519825, 16.57852306707251344, 18.34838970509067479 ) ) ;
#6566 = VERTEX_POINT ( 'NONE', #12873 ) ;
#6567 = VERTEX_POINT ( 'NONE', #26598 ) ;
#6568 = DIRECTION ( 'NONE',  ( 1.000000000000000000, 0.000000000000000000, 0.000000000000000000 ) ) ;
#6569 = CIRCLE ( 'NONE', #20501, 45.00000000000000711 ) ;
#6570 = CARTESIAN_POINT ( 'NONE',  ( -10.82521593960875528, 5.400395169024524655, 24.50000000000000000 ) ) ;
#6571 = CARTESIAN_POINT ( 'NONE',  ( -5.020628478053032140, 16.27454347535057622, 20.19668224736330941 ) ) ;
#6572 = CARTESIAN_POINT ( 'NONE',  ( -23.13350093726293366, 11.03024450687078506, 45.12903505574596608 ) ) ;
#6573 = CARTESIAN_POINT ( 'NONE',  ( -19.67362645597749449, 33.08334462853547819, 27.50000000000000000 ) ) ;
#6574 = CONTEXT_DEPENDENT_SHAPE_REPRESENTATION ( #26150, #9670 ) ;
#6575 = CARTESIAN_POINT ( 'NONE',  ( -5.971396161871753705, 19.08775596758252391, 7.652108011868850035 ) ) ;
#6576 = EDGE_CURVE ( 'NONE', #18, #8092, #7632, .T. ) ;
#6577 = ORIENTED_EDGE ( 'NONE', *, *, #23178, .T. ) ;
#6578 = EDGE_CURVE ( 'NONE', #26575, #29559, #4626, .T. ) ;
#6579 = AXIS2_PLACEMENT_3D ( 'NONE', #15050, #12732, #22230 ) ;
#6580 = CARTESIAN_POINT ( 'NONE',  ( -19.96205336850438528, 1.490391487655214453, 6.672349528511551497 ) ) ;
#6581 = CARTESIAN_POINT ( 'NONE',  ( 14.70507365826911972, 13.55638513645771503, 20.32200205377525393 ) ) ;
#6582 = CARTESIAN_POINT ( 'NONE',  ( 27.03074382657074182, -6.449748410230990991, 42.96778633356034049 ) ) ;
#6583 = VERTEX_POINT ( 'NONE', #15030 ) ;
#6584 = DIRECTION ( 'NONE',  ( 0.000000000000000000, 0.000000000000000000, -1.000000000000000000 ) ) ;
#6585 = ORIENTED_EDGE ( 'NONE', *, *, #10687, .T. ) ;
#6586 = CARTESIAN_POINT ( 'NONE',  ( 18.59976559251667183, -7.400385892474091953, 5.872146474157316831 ) ) ;
#6587 = DIRECTION ( 'NONE',  ( 0.000000000000000000, 0.000000000000000000, 1.000000000000000000 ) ) ;
#6588 = ORIENTED_EDGE ( 'NONE', *, *, #28852, .F. ) ;
#6589 = CARTESIAN_POINT ( 'NONE',  ( 49.99999999999998579, 50.00000000000000000, 62.49999999999999289 ) ) ;
#6590 = CARTESIAN_POINT ( 'NONE',  ( 49.99999999999999289, 70.00000000000001421, 53.15267136187731722 ) ) ;
#6591 = AXIS2_PLACEMENT_3D ( 'NONE', #25782, #4411, #9407 ) ;
#6592 = DIRECTION ( 'NONE',  ( -0.6707505147970090897, 0.7416830501633074890, 0.000000000000000000 ) ) ;
#6593 = CARTESIAN_POINT ( 'NONE',  ( 0.000000000000000000, 1.699320956058915452E-16, -1.500000000000001776 ) ) ;
#6594 = CARTESIAN_POINT ( 'NONE',  ( -32.19782014694307293, 14.25394737442115733, 35.54550565580015586 ) ) ;
#6595 = DIRECTION ( 'NONE',  ( 1.000000000000000000, 0.000000000000000000, 0.000000000000000000 ) ) ;
#6596 = DIRECTION ( 'NONE',  ( 1.000000000000000000, 0.000000000000000000, 0.000000000000000000 ) ) ;
#6597 = VERTEX_POINT ( 'NONE', #9901 ) ;
#6598 = DIRECTION ( 'NONE',  ( -1.000000000000000000, 0.000000000000000000, 0.000000000000000000 ) ) ;
#6599 = CARTESIAN_POINT ( 'NONE',  ( 1.687027447297431371, 8.840471615930075799, -1.500000000000000888 ) ) ;
#6600 = VERTEX_POINT ( 'NONE', #24546 ) ;
#6601 = DIRECTION ( 'NONE',  ( -0.000000000000000000, -0.000000000000000000, 1.000000000000000000 ) ) ;
#6602 = CARTESIAN_POINT ( 'NONE',  ( -15.13023987665972392, -7.854877310202117435, 18.34838970509067479 ) ) ;
#6603 = CARTESIAN_POINT ( 'NONE',  ( 19.64114023396309960, -37.13592150529014191, -1.500000000000000000 ) ) ;
#6604 = CARTESIAN_POINT ( 'NONE',  ( 40.89187623478217404, 5.790488632116406187, -19.50000000000000355 ) ) ;
#6605 = ORIENTED_EDGE ( 'NONE', *, *, #9706, .T. ) ;
#6606 = FACE_BOUND ( 'NONE', #6195, .T. ) ;
#6607 = VECTOR ( 'NONE', #1319, 1000.000000000000000 ) ;
#6608 = CONICAL_SURFACE ( 'NONE', #24017, 37.50000000000001421, 0.7853981633974500554 ) ;
#6609 = CARTESIAN_POINT ( 'NONE',  ( -10.11202017158466759, 41.14070756921185534, -1.500000000000000000 ) ) ;
#6610 = CARTESIAN_POINT ( 'NONE',  ( 12.56271066119290936, -40.24229205698606648, 34.56094169196020260 ) ) ;
#6612 = CIRCLE ( 'NONE', #2127, 27.70876437800068359 ) ;
#6611 = DIRECTION ( 'NONE',  ( -1.000000000000000000, 0.000000000000000000, 0.000000000000000000 ) ) ;
#6613 = ORIENTED_EDGE ( 'NONE', *, *, #21231, .F. ) ;
#6614 = CARTESIAN_POINT ( 'NONE',  ( -13.37849590498012908, 10.56201291617988147, 7.652108011868850923 ) ) ;
#6615 = ORIENTED_EDGE ( 'NONE', *, *, #17370, .F. ) ;
#6616 = EDGE_CURVE ( 'NONE', #23323, #14013, #24083, .T. ) ;
#6617 = CARTESIAN_POINT ( 'NONE',  ( -9.471281197126605989, -0.4564504349074081091, 21.50000000000000000 ) ) ;
#6618 = DIRECTION ( 'NONE',  ( -0.000000000000000000, -0.000000000000000000, 1.000000000000000000 ) ) ;
#6619 = ADVANCED_FACE ( 'NONE', ( #7414 ), #16922, .F. ) ;
#6620 = ORIENTED_EDGE ( 'NONE', *, *, #12282, .T. ) ;
#6621 = CARTESIAN_POINT ( 'NONE',  ( -21.56196259436895346, -35.42116262697312123, 29.49711835318369424 ) ) ;
#6622 = ORIENTED_EDGE ( 'NONE', *, *, #11194, .F. ) ;
#6623 = CARTESIAN_POINT ( 'NONE',  ( -31.29501345865439532, 26.27841684421964885, -6.500000000000000888 ) ) ;
#6624 = CARTESIAN_POINT ( 'NONE',  ( 35.41742430504415040, 80.00000000000000000, 50.49999999999998579 ) ) ;
#6625 = ORIENTED_EDGE ( 'NONE', *, *, #23630, .F. ) ;
#6626 = CYLINDRICAL_SURFACE ( 'NONE', #3353, 15.00000000000000000 ) ;
#6627 = CIRCLE ( 'NONE', #22071, 0.7500000000000002220 ) ;
#6628 = LINE ( 'NONE', #16143, #8897 ) ;
#6629 = CARTESIAN_POINT ( 'NONE',  ( 8.840471615930072247, -1.687027447297460236, -3.621320343559650379 ) ) ;
#6630 = VECTOR ( 'NONE', #14583, 1000.000000000000000 ) ;
#6631 = CARTESIAN_POINT ( 'NONE',  ( -4.163336342344337027E-14, -1.387778780781445676E-14, 1.500000000000000000 ) ) ;
#6632 = CARTESIAN_POINT ( 'NONE',  ( 9.471281197126602436, 0.4564504349074715028, 13.00000000000000178 ) ) ;
#6633 = CARTESIAN_POINT ( 'NONE',  ( 10.18506332983503349, -29.04537757311073420, 24.50000000000000000 ) ) ;
#6634 = CARTESIAN_POINT ( 'NONE',  ( 8.884323311075775109, 1.438332125858202692, 21.50000000000000000 ) ) ;
#6635 = DIRECTION ( 'NONE',  ( 0.000000000000000000, 0.000000000000000000, 1.000000000000000000 ) ) ;
#6636 = CARTESIAN_POINT ( 'NONE',  ( -18.40581374043504681, -7.824871006739526180, 18.84056766331481825 ) ) ;
#6637 = CARTESIAN_POINT ( 'NONE',  ( -18.11003155545035881, -8.529482236167146070, 20.34789198813115263 ) ) ;
#6638 = DIRECTION ( 'NONE',  ( -0.000000000000000000, 1.132880637372608986E-16, -1.000000000000000000 ) ) ;
#6639 = ORIENTED_EDGE ( 'NONE', *, *, #9960, .F. ) ;
#6640 = EDGE_LOOP ( 'NONE', ( #2948, #13993, #21064, #103 ) ) ;
#6641 = DIRECTION ( 'NONE',  ( -0.000000000000000000, -0.000000000000000000, 1.000000000000000000 ) ) ;
#6642 = CARTESIAN_POINT ( 'NONE',  ( -19.64114023396061981, 37.13592150528867109, -1.500000000000000000 ) ) ;
#6643 = CARTESIAN_POINT ( 'NONE',  ( -1.687027447297492211, -8.840471615930066918, 21.50000000000000000 ) ) ;
#6644 = ORIENTED_EDGE ( 'NONE', *, *, #11651, .F. ) ;
#6645 = DIRECTION ( 'NONE',  ( 0.000000000000000000, 0.000000000000000000, 1.000000000000000000 ) ) ;
#6646 = CARTESIAN_POINT ( 'NONE',  ( 17.94887244118349301, -8.863227448567842615, 19.00652017443069752 ) ) ;
#6647 = CARTESIAN_POINT ( 'NONE',  ( 4.263339901971998636, 16.49757000336419210, 5.670038381137163519 ) ) ;
#6648 = VECTOR ( 'NONE', #13893, 1000.000000000000000 ) ;
#6649 = ORIENTED_EDGE ( 'NONE', *, *, #15667, .T. ) ;
#6650 = AXIS2_PLACEMENT_3D ( 'NONE', #8153, #17822, #30122 ) ;
#6651 = CARTESIAN_POINT ( 'NONE',  ( -19.85654738780300121, 2.535877853918448555, 5.651989602109218858 ) ) ;
#6652 = CARTESIAN_POINT ( 'NONE',  ( -21.14806837890567692, -37.61929654846579041, -16.50000000000000000 ) ) ;
#6653 = DIRECTION ( 'NONE',  ( 0.000000000000000000, 0.000000000000000000, 1.000000000000000000 ) ) ;
#6654 = ORIENTED_EDGE ( 'NONE', *, *, #15509, .F. ) ;
#6655 = LINE ( 'NONE', #28952, #16332 ) ;
#6656 = CARTESIAN_POINT ( 'NONE',  ( -25.53015708495999547, 6.470147010658195086, 44.42018155122911338 ) ) ;
#6657 = CARTESIAN_POINT ( 'NONE',  ( -15.01328179936714413, 13.21424408877643941, 7.526993102356318133 ) ) ;
#6658 = VERTEX_POINT ( 'NONE', #24085 ) ;
#6659 = CARTESIAN_POINT ( 'NONE',  ( -8.499586724479453181, -2.959227181723774525, -3.621320343559650379 ) ) ;
#6660 = DIRECTION ( 'NONE',  ( -0.000000000000000000, -0.000000000000000000, -1.000000000000000000 ) ) ;
#6661 = CYLINDRICAL_SURFACE ( 'NONE', #19066, 15.00000000000000000 ) ;
#6662 = B_SPLINE_SURFACE_WITH_KNOTS ( 'NONE', 1, 3, ( 
 ( #22826, #5528, #22661, #29868, #13020, #25160, #29547, #13328, #8509, #8181, #27204, #8341, #5840, #1311, #15497, #10667, #17537, #27056, #10989, #25015, #1477, #10829, #30010, #15339, #20338, #12711, #27521, #12872, #10366, #24870, #24545, #6142, #22371, #1156, #20173, #8651, #17856, #27373, #5681, #5994, #3806, #18159 ),
 ( #15029, #3191, #844, #22208, #8033, #19880, #24697, #3340, #29695, #28284, #6750, #27974, #9410, #30155, #11445, #8955, #6603, #3969, #27665, #15968, #16119, #25488, #20931, #4414, #4111, #23276, #25638, #30308, #21082, #22972, #6294, #16265, #30602, #23577, #9246, #15806, #1629, #11140, #25326, #18471, #4254, #18766 ) ),
 .UNSPECIFIED., .F., .T., .F.,
 ( 2, 2 ),
 ( 4, 2, 2, 2, 2, 2, 2, 2, 2, 2, 2, 2, 2, 2, 2, 2, 2, 2, 2, 2, 4 ),
 ( 0.000000000000000000, 1.000000000000000000 ),
 ( 0.000000000000000000, 0.1963495408493620697, 0.3926990816987241395, 0.7853981633974482790, 1.178097245096172418, 1.570796326794896558, 1.963495408493620697, 2.356194490192344837, 2.748893571891068976, 2.945243112740430824, 3.141592653589793116, 3.337942194439155408, 3.534291735288517255, 3.926990816987241395, 4.319689898685965090, 4.712388980384689674, 5.105088062083414258, 5.497787143782137953, 5.890486225480861648, 6.086835766330223940, 6.283185307179586232 ),
 .UNSPECIFIED. ) ;
#6663 = CARTESIAN_POINT ( 'NONE',  ( 0.4421796641654209825, -17.03052986487778497, 7.595116371587256054 ) ) ;
#6664 = CARTESIAN_POINT ( 'NONE',  ( 0.000000000000000000, 0.000000000000000000, -87.50000000000000000 ) ) ;
#6665 = CARTESIAN_POINT ( 'NONE',  ( 26.36764545593177544, -31.31467416275353344, 1.500000000000000000 ) ) ;
#6666 = AXIS2_PLACEMENT_3D ( 'NONE', #19605, #19926, #26953 ) ;
#6667 = CARTESIAN_POINT ( 'NONE',  ( -17.06629068372215130, 0.6401188461407910646, 19.36813350477385143 ) ) ;
#6668 = CARTESIAN_POINT ( 'NONE',  ( 0.000000000000000000, -2.435693370351110282E-15, 21.50000000000000355 ) ) ;
#6669 = VERTEX_POINT ( 'NONE', #26748 ) ;
#6670 = AXIS2_PLACEMENT_3D ( 'NONE', #3141, #27928, #6404 ) ;
#6671 = CARTESIAN_POINT ( 'NONE',  ( 10.67336573878037420, -13.33112751634288706, 19.58863275299554019 ) ) ;
#6672 = CARTESIAN_POINT ( 'NONE',  ( 21.86019681245146629, -31.48592878035298170, 27.50000000000001776 ) ) ;
#6673 = ORIENTED_EDGE ( 'NONE', *, *, #18952, .T. ) ;
#6674 = VERTEX_POINT ( 'NONE', #12239 ) ;
#6675 = EDGE_CURVE ( 'NONE', #12022, #17226, #383, .T. ) ;
#6676 = CARTESIAN_POINT ( 'NONE',  ( -15.84912786217079450, 12.19893545703369142, 7.272192800924334399 ) ) ;
#6677 = ADVANCED_FACE ( 'NONE', ( #3039 ), #19416, .F. ) ;
#6678 = DIRECTION ( 'NONE',  ( -1.000000000000000000, 0.000000000000000000, 0.000000000000000000 ) ) ;
#6679 = ORIENTED_EDGE ( 'NONE', *, *, #14496, .T. ) ;
#6680 = CARTESIAN_POINT ( 'NONE',  ( -26.11179934312166750, 14.04991663536888957, 45.34931131770228063 ) ) ;
#6681 = FACE_OUTER_BOUND ( 'NONE', #9730, .T. ) ;
#6682 = EDGE_LOOP ( 'NONE', ( #13034, #27059, #30012, #3163 ) ) ;
#6683 = EDGE_CURVE ( 'NONE', #15816, #12560, #22827, .T. ) ;
#6684 = CARTESIAN_POINT ( 'NONE',  ( -15.51517975927889204, 12.62116967784147725, 18.37545668562167478 ) ) ;
#6685 = DIRECTION ( 'NONE',  ( 0.000000000000000000, 0.000000000000000000, -1.000000000000000000 ) ) ;
#6686 = EDGE_LOOP ( 'NONE', ( #4658, #30851 ) ) ;
#6687 = CARTESIAN_POINT ( 'NONE',  ( 0.8762659238204211221, 8.999114229549594057, -1.500000000000000888 ) ) ;
#6688 = VECTOR ( 'NONE', #28371, 1000.000000000000000 ) ;
#6689 = ORIENTED_EDGE ( 'NONE', *, *, #24489, .T. ) ;
#6690 = EDGE_CURVE ( 'NONE', #10914, #2256, #9123, .T. ) ;
#6691 = LINE ( 'NONE', #16203, #30842 ) ;
#6692 = VERTEX_POINT ( 'NONE', #25016 ) ;
#6693 = EDGE_CURVE ( 'NONE', #4980, #10762, #23554, .T. ) ;
#6694 = ORIENTED_EDGE ( 'NONE', *, *, #15464, .T. ) ;
#6695 = EDGE_CURVE ( 'NONE', #22584, #8392, #16637, .T. ) ;
#6696 = DIRECTION ( 'NONE',  ( -1.000000000000000000, 0.000000000000000000, 0.000000000000000000 ) ) ;
#6697 = DIRECTION ( 'NONE',  ( 0.000000000000000000, 0.000000000000000000, 1.000000000000000000 ) ) ;
#6698 = CARTESIAN_POINT ( 'NONE',  ( 1.665992581735233014, -16.99218467486976891, 18.84329447212443753 ) ) ;
#6699 = DIRECTION ( 'NONE',  ( -0.5406408174555976665, 0.8412535328311812055, 0.000000000000000000 ) ) ;
#6700 = EDGE_LOOP ( 'NONE', ( #10809, #11098, #11939, #30233 ) ) ;
#6701 = CARTESIAN_POINT ( 'NONE',  ( -19.85166970746586301, 2.573860339590182456, 18.34969686940296185 ) ) ;
#6702 = CARTESIAN_POINT ( 'NONE',  ( 3.912171961291947664, 8.637616862297855747, 1.500000000000001332 ) ) ;
#6703 = CARTESIAN_POINT ( 'NONE',  ( -13.42620032052776047, 10.50496109755573926, 20.34789198813115263 ) ) ;
#6704 = CARTESIAN_POINT ( 'NONE',  ( 4.454645749177147174, 19.51581340210660187, 18.82680253904184298 ) ) ;
#6705 = ORIENTED_EDGE ( 'NONE', *, *, #4438, .F. ) ;
#6706 = ORIENTED_EDGE ( 'NONE', *, *, #10099, .F. ) ;
#6707 = VECTOR ( 'NONE', #22221, 1000.000000000000000 ) ;
#6708 = PLANE ( 'NONE',  #8841 ) ;
#6709 = EDGE_CURVE ( 'NONE', #21157, #10630, #22054, .T. ) ;
#6710 = CARTESIAN_POINT ( 'NONE',  ( -1.000000000000008438, 13.00000000000001421, 43.10779406592839536 ) ) ;
#6711 = EDGE_CURVE ( 'NONE', #17300, #6047, #25560, .T. ) ;
#6712 = CARTESIAN_POINT ( 'NONE',  ( 8.778767752581492445, -41.45290410434266448, 20.58727206569324153 ) ) ;
#6713 = LINE ( 'NONE', #9210, #11369 ) ;
#6714 = EDGE_CURVE ( 'NONE', #12583, #23101, #8652, .T. ) ;
#6715 = LINE ( 'NONE', #1888, #20578 ) ;
#6716 = EDGE_CURVE ( 'NONE', #27888, #4214, #27831, .T. ) ;
#6717 = CARTESIAN_POINT ( 'NONE',  ( -30.97476472108959911, 20.16426083678214809, 27.50000000000000711 ) ) ;
#6718 = CARTESIAN_POINT ( 'NONE',  ( 34.70577939417261604, -10.49309206032036634, 34.49999999999999289 ) ) ;
#6719 = VERTEX_POINT ( 'NONE', #20026 ) ;
#6720 = EDGE_CURVE ( 'NONE', #19394, #13900, #2153, .T. ) ;
#6721 = CARTESIAN_POINT ( 'NONE',  ( -19.93785161568571951, 1.787211178945724788, 7.366751648393900176 ) ) ;
#6722 = CARTESIAN_POINT ( 'NONE',  ( -35.46011056729421540, 7.038057716383124607, 34.64849135038186745 ) ) ;
#6723 = CARTESIAN_POINT ( 'NONE',  ( 19.64177907938615064, -36.71644397333972876, 24.50000000000000000 ) ) ;
#6724 = ADVANCED_FACE ( 'NONE', ( #29870 ), #29548, .F. ) ;
#6725 = ORIENTED_EDGE ( 'NONE', *, *, #21544, .T. ) ;
#6726 = DIRECTION ( 'NONE',  ( -1.000000000000000000, 0.000000000000000000, 0.000000000000000000 ) ) ;
#6727 = ORIENTED_EDGE ( 'NONE', *, *, #29150, .F. ) ;
#6728 = EDGE_CURVE ( 'NONE', #7440, #11068, #15597, .T. ) ;
#6729 = CARTESIAN_POINT ( 'NONE',  ( 18.41347767057966678, -7.852385608265392669, 5.661398277488801867 ) ) ;
#6730 = CARTESIAN_POINT ( 'NONE',  ( -8.304834736901785419, 43.14465394274145638, -16.50000000000000355 ) ) ;
#6731 = ORIENTED_EDGE ( 'NONE', *, *, #27513, .F. ) ;
#6732 = CARTESIAN_POINT ( 'NONE',  ( 8.553213014649442059, -38.39187072122768285, 27.49999999999999645 ) ) ;
#6733 = AXIS2_PLACEMENT_3D ( 'NONE', #22142, #17000, #4999 ) ;
#6734 = CARTESIAN_POINT ( 'NONE',  ( 77.99999999999998579, -42.50000000000002132, 24.50000000000000000 ) ) ;
#6735 = CARTESIAN_POINT ( 'NONE',  ( -50.00000000000000000, 87.00000000000001421, 52.49999999999999289 ) ) ;
#6736 = LINE ( 'NONE', #20622, #15792 ) ;
#6737 = CARTESIAN_POINT ( 'NONE',  ( -6.044935790874366610, 19.08338196164711675, 20.34789198813115263 ) ) ;
#6738 = B_SPLINE_CURVE_WITH_KNOTS ( 'NONE', 3,
 ( #19846, #8008, #24671, #979, #10489, #22481, #29520, #8159, #8312, #5812, #15309, #1127 ),
 .UNSPECIFIED., .F., .F.,
 ( 4, 2, 2, 2, 2, 4 ),
 ( 2.975219550396606016E-07, 0.0009689891316535842632, 0.001937680741352128993, 0.002906372351050673722, 0.003390718155899950965, 0.003875063960749227775 ),
 .UNSPECIFIED. ) ;
#6739 = DIRECTION ( 'NONE',  ( -0.000000000000000000, 0.000000000000000000, 1.000000000000000000 ) ) ;
#6740 = CARTESIAN_POINT ( 'NONE',  ( 8.728722367416583694, -2.516121109503213216, 13.22130136205108819 ) ) ;
#6741 = ORIENTED_EDGE ( 'NONE', *, *, #22526, .T. ) ;
#6742 = EDGE_CURVE ( 'NONE', #14629, #11642, #22509, .T. ) ;
#6743 = EDGE_CURVE ( 'NONE', #5791, #19317, #23045, .T. ) ;
#6744 = LINE ( 'NONE', #18466, #25299 ) ;
#6745 = AXIS2_PLACEMENT_3D ( 'NONE', #8707, #16338, #6367 ) ;
#6746 = LINE ( 'NONE', #1764, #846 ) ;
#6747 = VERTEX_POINT ( 'NONE', #8342 ) ;
#6748 = CYLINDRICAL_SURFACE ( 'NONE', #1614, 9.482273699623480212 ) ;
#6749 = FACE_OUTER_BOUND ( 'NONE', #16940, .T. ) ;
#6750 = CARTESIAN_POINT ( 'NONE',  ( 39.00000000000000000, 5.563236990218597633, -1.500000000000000000 ) ) ;
#6751 = CARTESIAN_POINT ( 'NONE',  ( 5.374868878255610660, 44.10336124695606230, -19.50000000000000355 ) ) ;
#6752 = ORIENTED_EDGE ( 'NONE', *, *, #16434, .F. ) ;
#6753 = CARTESIAN_POINT ( 'NONE',  ( 0.09286997694516960222, -20.00015982525768266, 18.37250658438899364 ) ) ;
#6754 = CIRCLE ( 'NONE', #1796, 50.00000000000000000 ) ;
#6755 = CARTESIAN_POINT ( 'NONE',  ( -2.552544031601109875, 42.50000000001772094, -1.500000000000000000 ) ) ;
#6756 = CARTESIAN_POINT ( 'NONE',  ( 29.13062620811776782, -28.39040064518643547, 30.21738835640542220 ) ) ;
#6757 = CARTESIAN_POINT ( 'NONE',  ( 25.23756106473024019, 11.43858098102958287, -1.500000000000000000 ) ) ;
#6758 = VERTEX_POINT ( 'NONE', #15340 ) ;
#6759 = AXIS2_PLACEMENT_3D ( 'NONE', #21371, #9994, #2656 ) ;
#6760 = CARTESIAN_POINT ( 'NONE',  ( -12.56641067637617759, -40.32935944494947478, -1.500000000000000000 ) ) ;
#6761 = CARTESIAN_POINT ( 'NONE',  ( 0.000000000000000000, -2.775557561562891351E-14, 157.4999999999999716 ) ) ;
#6762 = ORIENTED_EDGE ( 'NONE', *, *, #14771, .F. ) ;
#6763 = CIRCLE ( 'NONE', #10257, 15.00000000000000000 ) ;
#6764 = DIRECTION ( 'NONE',  ( 0.000000000000000000, -1.000000000000000000, 0.000000000000000000 ) ) ;
#6765 = ORIENTED_EDGE ( 'NONE', *, *, #11376, .F. ) ;
#6766 = DIRECTION ( 'NONE',  ( -0.000000000000000000, -0.000000000000000000, -1.000000000000000000 ) ) ;
#6767 = CARTESIAN_POINT ( 'NONE',  ( 4.216636297896259045, 37.26217892624188011, 37.50000000000000000 ) ) ;
#6768 = DIRECTION ( 'NONE',  ( 1.000000000000000000, 0.000000000000000000, 0.000000000000000000 ) ) ;
#6769 = ORIENTED_EDGE ( 'NONE', *, *, #24779, .T. ) ;
#6770 = CARTESIAN_POINT ( 'NONE',  ( 18.71829317531095072, -7.044536951825313587, 6.788986777570698017 ) ) ;
#6771 = AXIS2_PLACEMENT_3D ( 'NONE', #7171, #12010, #25735 ) ;
#6772 = CARTESIAN_POINT ( 'NONE',  ( 8.795879380940563763, 2.270234684139707859, -1.500000000000001554 ) ) ;
#6773 = DIRECTION ( 'NONE',  ( 0.000000000000000000, 0.000000000000000000, -1.000000000000000000 ) ) ;
#6774 = LINE ( 'NONE', #17603, #29066 ) ;
#6775 = ORIENTED_EDGE ( 'NONE', *, *, #8004, .T. ) ;
#6776 = EDGE_CURVE ( 'NONE', #19006, #4914, #19706, .T. ) ;
#6777 = CARTESIAN_POINT ( 'NONE',  ( 0.000000000000000000, 0.000000000000000000, 21.50000000000000000 ) ) ;
#6778 = VECTOR ( 'NONE', #3170, 1000.000000000000227 ) ;
#6779 = CARTESIAN_POINT ( 'NONE',  ( 6.900000000000000355, 7.794228634059940042, 4.500000000000011546 ) ) ;
#6780 = FACE_OUTER_BOUND ( 'NONE', #2629, .T. ) ;
#6781 = CARTESIAN_POINT ( 'NONE',  ( -13.11527592942575282, -10.04126165406389326, 24.50000000000000000 ) ) ;
#6782 = CARTESIAN_POINT ( 'NONE',  ( 1.794035659141604899, 42.46622758119957552, 19.75017875872448059 ) ) ;
#6783 = DIRECTION ( 'NONE',  ( -1.000000000000000000, 0.000000000000000000, 0.000000000000000000 ) ) ;
#6784 = CARTESIAN_POINT ( 'NONE',  ( -18.32589276785171606, -8.054604467211156305, 20.12545155307891065 ) ) ;
#6785 = CARTESIAN_POINT ( 'NONE',  ( 32.28307784207223108, -8.475829241206289666, 37.38016955275583086 ) ) ;
#6786 = CIRCLE ( 'NONE', #10283, 6.000000000000005329 ) ;
#6787 = VERTEX_POINT ( 'NONE', #4716 ) ;
#6788 = ORIENTED_EDGE ( 'NONE', *, *, #22724, .T. ) ;
#6789 = FACE_OUTER_BOUND ( 'NONE', #820, .T. ) ;
#6790 = PRESENTATION_LAYER_ASSIGNMENT (  '', '', ( #24733 ) ) ;
#6791 = CARTESIAN_POINT ( 'NONE',  ( 4.336808689942017736E-16, 42.50000000000000000, -1.500000000000000000 ) ) ;
#6792 = LINE ( 'NONE', #4609, #1453 ) ;
#6793 = ORIENTED_EDGE ( 'NONE', *, *, #4185, .T. ) ;
#6794 = CARTESIAN_POINT ( 'NONE',  ( -6.045292009585545578, 15.95527889502104024, 20.24143955528809258 ) ) ;
#6795 = CARTESIAN_POINT ( 'NONE',  ( 4.476939094886643211, 16.43504713094788272, 7.557577766377196582 ) ) ;
#6796 = AXIS2_PLACEMENT_3D ( 'NONE', #21849, #29342, #17014 ) ;
#6797 = VERTEX_POINT ( 'NONE', #16267 ) ;
#6798 = CARTESIAN_POINT ( 'NONE',  ( -19.71314312682348557, 3.479754436677863438, 6.420335371522007506 ) ) ;
#6799 = AXIS2_PLACEMENT_3D ( 'NONE', #15837, #13669, #4138 ) ;
#6800 = CARTESIAN_POINT ( 'NONE',  ( 14.24237608451263348, 14.06627278277045079, 6.995624166085161910 ) ) ;
#6801 = VECTOR ( 'NONE', #27037, 1000.000000000000000 ) ;
#6802 = CARTESIAN_POINT ( 'NONE',  ( -9.792086282299422351, -42.77788222952042929, -16.50000000000000355 ) ) ;
#6803 = CARTESIAN_POINT ( 'NONE',  ( -38.62541652119597302, 5.911948292485620371, 32.11511063132802235 ) ) ;
#6804 = ORIENTED_EDGE ( 'NONE', *, *, #2144, .T. ) ;
#6805 = DIRECTION ( 'NONE',  ( 0.3598999890241668664, 0.9329908884337534403, 0.000000000000000000 ) ) ;
#6806 = DIRECTION ( 'NONE',  ( -1.000000000000000000, 0.000000000000000000, 0.000000000000000000 ) ) ;
#6807 = DIRECTION ( 'NONE',  ( -0.000000000000000000, 0.000000000000000000, 1.000000000000000000 ) ) ;
#6808 = ORIENTED_EDGE ( 'NONE', *, *, #14327, .T. ) ;
#6809 = CARTESIAN_POINT ( 'NONE',  ( 16.87360174012497538, 2.245128340606972639, 19.66962785902261857 ) ) ;
#6810 = CARTESIAN_POINT ( 'NONE',  ( -4.163336342344337027E-14, 1.387778780781445676E-14, 77.49999999999998579 ) ) ;
#6811 = CARTESIAN_POINT ( 'NONE',  ( -9.056208293496290196, 2.810445847081948667, 21.50000000000000000 ) ) ;
#6812 = CARTESIAN_POINT ( 'NONE',  ( -4.163336342344337027E-14, 1.387778780781445676E-14, 35.37867965644034740 ) ) ;
#6813 = VECTOR ( 'NONE', #23335, 1000.000000000000000 ) ;
#6814 = DIRECTION ( 'NONE',  ( 0.000000000000000000, -1.000000000000000000, 0.000000000000000000 ) ) ;
#6815 = CIRCLE ( 'NONE', #19772, 11.99999999999998934 ) ;
#6816 = DIRECTION ( 'NONE',  ( 0.000000000000000000, 0.000000000000000000, -1.000000000000000000 ) ) ;
#6817 = CARTESIAN_POINT ( 'NONE',  ( -19.93785161568571951, 1.787211178945723677, 20.06253562465620632 ) ) ;
#6818 = CARTESIAN_POINT ( 'NONE',  ( -13.00999358272542494, -0.8602714556717691030, 1.500000000000001332 ) ) ;
#6819 = VERTEX_POINT ( 'NONE', #19064 ) ;
#6820 = AXIS2_PLACEMENT_3D ( 'NONE', #7674, #2997, #12357 ) ;
#6821 = CARTESIAN_POINT ( 'NONE',  ( 11.94417982595701666, -16.06366807669217067, 19.47783254395485031 ) ) ;
#6822 = AXIS2_PLACEMENT_3D ( 'NONE', #24935, #13816, #4597 ) ;
#6823 = DIRECTION ( 'NONE',  ( 0.000000000000000000, 0.000000000000000000, -1.000000000000000000 ) ) ;
#6824 = VERTEX_POINT ( 'NONE', #21234 ) ;
#6825 = ORIENTED_EDGE ( 'NONE', *, *, #2163, .T. ) ;
#6826 = CARTESIAN_POINT ( 'NONE',  ( 5.296161872597624942, 19.28602264385379428, 20.34789198813115263 ) ) ;
#6827 = ORIENTED_EDGE ( 'NONE', *, *, #30346, .T. ) ;
#6828 = B_SPLINE_CURVE_WITH_KNOTS ( 'NONE', 3,
 ( #23719, #11892, #9539, #19054, #26223, #12816, #14988, #19519, #26542, #17494, #12515, #5643, #22319, #5170, #8139, #12668, #24816, #12355 ),
 .UNSPECIFIED., .F., .F.,
 ( 4, 2, 2, 2, 2, 2, 2, 2, 4 ),
 ( 0.003174295595554328664, 0.003570702171545568800, 0.003967108747536808935, 0.004363515323528048204, 0.004759921899519288339, 0.005156328475510528475, 0.005552735051501767743, 0.005949141627493007879, 0.006345548203484248015 ),
 .UNSPECIFIED. ) ;
#6829 = AXIS2_PLACEMENT_3D ( 'NONE', #24427, #19445, #26468 ) ;
#6830 = FACE_OUTER_BOUND ( 'NONE', #21336, .T. ) ;
#6831 = FILL_AREA_STYLE ('',( #5115 ) ) ;
#6832 = CIRCLE ( 'NONE', #27783, 0.7500000000000006661 ) ;
#6833 = ORIENTED_EDGE ( 'NONE', *, *, #28102, .F. ) ;
#6834 = FACE_OUTER_BOUND ( 'NONE', #23666, .T. ) ;
#6835 = AXIS2_PLACEMENT_3D ( 'NONE', #22917, #3750, #1565 ) ;
#6836 = DIRECTION ( 'NONE',  ( 0.000000000000000000, 1.000000000000000000, 1.156482317317869999E-16 ) ) ;
#6837 = VERTEX_POINT ( 'NONE', #13782 ) ;
#6838 = AXIS2_PLACEMENT_3D ( 'NONE', #10223, #15361, #869 ) ;
#6839 = ORIENTED_EDGE ( 'NONE', *, *, #24420, .T. ) ;
#6840 = FACE_OUTER_BOUND ( 'NONE', #18554, .T. ) ;
#6841 = VERTEX_POINT ( 'NONE', #7058 ) ;
#6842 = ORIENTED_EDGE ( 'NONE', *, *, #9430, .T. ) ;
#6843 = ADVANCED_FACE ( 'NONE', ( #4415 ), #18928, .F. ) ;
#6844 = CIRCLE ( 'NONE', #12863, 9.482273699623480212 ) ;
#6845 = PRODUCT_DEFINITION ( 'UNKNOWN', '', #8918, #774 ) ;
#6846 = CARTESIAN_POINT ( 'NONE',  ( 20.47140833542507821, -26.57182937991349903, -6.500000000000000888 ) ) ;
#6847 = CARTESIAN_POINT ( 'NONE',  ( -0.1984805017707983177, -17.02075843868200522, 19.60617949693493856 ) ) ;
#6848 = AXIS2_PLACEMENT_3D ( 'NONE', #6282, #18463, #1469 ) ;
#6849 = CIRCLE ( 'NONE', #19815, 20.00000000000000000 ) ;
#6850 = DIRECTION ( 'NONE',  ( 0.000000000000000000, -0.000000000000000000, 1.000000000000000000 ) ) ;
#6851 = DIRECTION ( 'NONE',  ( -1.243218491116710699E-14, 1.000000000000000000, 0.000000000000000000 ) ) ;
#6852 = CARTESIAN_POINT ( 'NONE',  ( 19.86222817340373226, 2.491431357970652183, 18.63641924841378028 ) ) ;
#6853 = VERTEX_POINT ( 'NONE', #25933 ) ;
#6854 = EDGE_CURVE ( 'NONE', #7845, #13900, #25639, .T. ) ;
#6855 = CARTESIAN_POINT ( 'NONE',  ( -19.75958569938476472, 3.205325445645400784, 18.63641924841378028 ) ) ;
#6856 = CARTESIAN_POINT ( 'NONE',  ( 11.43275458328725591, -37.45803590232208080, 34.49999999999998579 ) ) ;
#6857 = AXIS2_PLACEMENT_3D ( 'NONE', #16480, #19434, #9617 ) ;
#6858 = CARTESIAN_POINT ( 'NONE',  ( -15.80654879600846741, 12.28271411401622970, 7.366751648393900176 ) ) ;
#6859 = CYLINDRICAL_SURFACE ( 'NONE', #3863, 9.482273699623480212 ) ;
#6860 = ORIENTED_EDGE ( 'NONE', *, *, #15116, .T. ) ;
#6861 = ORIENTED_EDGE ( 'NONE', *, *, #16607, .F. ) ;
#6862 = AXIS2_PLACEMENT_3D ( 'NONE', #13803, #16444, #11467 ) ;
#6863 = CYLINDRICAL_SURFACE ( 'NONE', #26768, 21.71568325578263625 ) ;
#6864 = LINE ( 'NONE', #28700, #14621 ) ;
#6865 = FACE_OUTER_BOUND ( 'NONE', #30544, .T. ) ;
#6866 = DIRECTION ( 'NONE',  ( 1.000000000000000000, 0.000000000000000000, 0.000000000000000000 ) ) ;
#6867 = DIRECTION ( 'NONE',  ( 1.000000000000000000, 0.000000000000000000, 0.000000000000000000 ) ) ;
#6868 = CARTESIAN_POINT ( 'NONE',  ( -32.32764558496669594, 17.38770747897534719, 27.50000000000000000 ) ) ;
#6869 = EDGE_CURVE ( 'NONE', #9137, #26641, #23427, .T. ) ;
#6870 = DIRECTION ( 'NONE',  ( 1.000000000000000000, 0.000000000000000000, 0.000000000000000000 ) ) ;
#6871 = AXIS2_PLACEMENT_3D ( 'NONE', #4501, #30537, #11669 ) ;
#6872 = ORIENTED_EDGE ( 'NONE', *, *, #20439, .F. ) ;
#6873 = AXIS2_PLACEMENT_3D ( 'NONE', #18609, #27826, #11582 ) ;
#6874 = ADVANCED_BREP_SHAPE_REPRESENTATION ( '', ( #2508, #7396 ), #26315 ) ;
#6875 = CARTESIAN_POINT ( 'NONE',  ( -17.05861610865858324, 0.7402736376837879551, 7.098451512883313441 ) ) ;
#6876 = CARTESIAN_POINT ( 'NONE',  ( 14.79453494486351772, 13.45878767717418789, 20.34789198813115618 ) ) ;
#6877 = CARTESIAN_POINT ( 'NONE',  ( 19.81789086666766764, 2.695592600026628372, 18.47110296274024321 ) ) ;
#6878 = ORIENTED_EDGE ( 'NONE', *, *, #13585, .F. ) ;
#6879 = CARTESIAN_POINT ( 'NONE',  ( 29.99999999999925038, 1.387778780781445676E-14, 67.49999999999997158 ) ) ;
#6880 = EDGE_LOOP ( 'NONE', ( #2481, #17859, #18852 ) ) ;
#6881 = CARTESIAN_POINT ( 'NONE',  ( -4.776122516674677878E-15, -42.50000000000000000, 28.83974596215560737 ) ) ;
#6882 = AXIS2_PLACEMENT_3D ( 'NONE', #27040, #20008, #10185 ) ;
#6883 = CARTESIAN_POINT ( 'NONE',  ( -0.2599583092368172865, 44.07656244530785727, -16.50000000000000355 ) ) ;
#6884 = ORIENTED_EDGE ( 'NONE', *, *, #22415, .F. ) ;
#6885 = CARTESIAN_POINT ( 'NONE',  ( 18.66785090198818864, 33.79720267974621351, 27.50000000000000000 ) ) ;
#6886 = ADVANCED_FACE ( 'NONE', ( #16565 ), #14217, .F. ) ;
#6887 = LINE ( 'NONE', #11888, #23727 ) ;
#6888 = ADVANCED_FACE ( 'NONE', ( #23732 ), #26237, .F. ) ;
#6889 = DIRECTION ( 'NONE',  ( 0.000000000000000000, 0.000000000000000000, 1.000000000000000000 ) ) ;
#6890 = CARTESIAN_POINT ( 'NONE',  ( -18.45589647530846023, -7.705834498630351526, 6.781503518395066266 ) ) ;
#6891 = CARTESIAN_POINT ( 'NONE',  ( -6.185259412586026961, 19.03819474808297230, 20.32367522806703874 ) ) ;
#6892 = DIRECTION ( 'NONE',  ( 0.000000000000000000, 0.000000000000000000, 1.000000000000000000 ) ) ;
#6893 = LINE ( 'NONE', #26, #29262 ) ;
#6894 = EDGE_CURVE ( 'NONE', #21299, #6719, #9248, .T. ) ;
#6895 = CARTESIAN_POINT ( 'NONE',  ( -1.000000000000008438, 13.00000000000001421, 24.50000000000000000 ) ) ;
#6896 = ORIENTED_EDGE ( 'NONE', *, *, #29594, .T. ) ;
#6897 = ADVANCED_FACE ( 'NONE', ( #4566 ), #30309, .T. ) ;
#6898 = DIRECTION ( 'NONE',  ( -1.000000000000000000, 0.000000000000000000, 0.000000000000000000 ) ) ;
#6899 = CIRCLE ( 'NONE', #13378, 0.7500000000000006661 ) ;
#6900 = VECTOR ( 'NONE', #17424, 1000.000000000000000 ) ;
#6901 = LINE ( 'NONE', #22967, #20807 ) ;
#6902 = AXIS2_PLACEMENT_3D ( 'NONE', #3942, #16228, #11107 ) ;
#6903 = CYLINDRICAL_SURFACE ( 'NONE', #2829, 1.000000000000009548 ) ;
#6904 = EDGE_LOOP ( 'NONE', ( #8334, #5852, #22899, #21413 ) ) ;
#6905 = EDGE_CURVE ( 'NONE', #9950, #25953, #21083, .T. ) ;
#6906 = CARTESIAN_POINT ( 'NONE',  ( 1.438332125858173605, -8.884323311075778662, 21.50000000000000000 ) ) ;
#6907 = FACE_OUTER_BOUND ( 'NONE', #19114, .T. ) ;
#6909 = ADVANCED_FACE ( 'NONE', ( #9411 ), #13136, .T. ) ;
#6908 = LINE ( 'NONE', #7055, #27693 ) ;
#6910 = CARTESIAN_POINT ( 'NONE',  ( -14.58213539500865785, 7.758783772730382111, 24.50000000000000000 ) ) ;
#6911 = CARTESIAN_POINT ( 'NONE',  ( 25.19442432474404470, 35.44676296256560022, -19.50000000000000355 ) ) ;
#6912 = CIRCLE ( 'NONE', #3442, 3.000000000000002665 ) ;
#6913 = ORIENTED_EDGE ( 'NONE', *, *, #24096, .T. ) ;
#6914 = CARTESIAN_POINT ( 'NONE',  ( -4.608906612435655248, -7.730328572437724866, 1.500000000000001332 ) ) ;
#6915 = EDGE_CURVE ( 'NONE', #12408, #8486, #8625, .T. ) ;
#6916 = DIRECTION ( 'NONE',  ( 1.000000000000000000, 0.000000000000000000, 0.000000000000000000 ) ) ;
#6917 = CARTESIAN_POINT ( 'NONE',  ( 20.93653161406057350, -35.88774558615511978, 34.51026993352196115 ) ) ;
#6918 = FACE_OUTER_BOUND ( 'NONE', #5739, .T. ) ;
#6919 = VERTEX_POINT ( 'NONE', #25133 ) ;
#6920 = CARTESIAN_POINT ( 'NONE',  ( -14.01107592578417993, 9.765138712360668549, 6.783738457429056012 ) ) ;
#6921 = DIRECTION ( 'NONE',  ( 0.000000000000000000, 0.000000000000000000, 1.000000000000000000 ) ) ;
#6922 = DIRECTION ( 'NONE',  ( 1.000000000000000000, 0.000000000000000000, 0.000000000000000000 ) ) ;
#6923 = B_SPLINE_CURVE_WITH_KNOTS ( 'NONE', 3,
 ( #14990, #24502, #24657, #10313, #3147, #12670, #22164, #19829, #29352, #17496, #5645, #3292 ),
 .UNSPECIFIED., .F., .F.,
 ( 4, 2, 2, 2, 2, 4 ),
 ( 2.975219550396606016E-07, 0.0009689891316535838295, 0.001937680741352128125, 0.002906372351050672421, 0.003390718155899948363, 0.003875063960749225173 ),
 .UNSPECIFIED. ) ;
#6924 = ORIENTED_EDGE ( 'NONE', *, *, #16803, .F. ) ;
#6925 = EDGE_LOOP ( 'NONE', ( #30690, #28766, #20898, #18247, #21594 ) ) ;
#6926 = FACE_OUTER_BOUND ( 'NONE', #24397, .T. ) ;
#6927 = CIRCLE ( 'NONE', #8945, 15.00000000000000000 ) ;
#6928 = ORIENTED_EDGE ( 'NONE', *, *, #29680, .F. ) ;
#6929 = CARTESIAN_POINT ( 'NONE',  ( -0.2808233399669979313, -20.01605574108312169, 18.55820869691756769 ) ) ;
#6930 = EDGE_CURVE ( 'NONE', #8512, #26677, #26564, .T. ) ;
#6931 = ADVANCED_FACE ( 'NONE', ( #27486 ), #22632, .F. ) ;
#6932 = CARTESIAN_POINT ( 'NONE',  ( -7.685008110482990595, -15.25093183970990296, 6.447548852708279377 ) ) ;
#6933 = DIRECTION ( 'NONE',  ( 0.2972711322815261292, 0.9547931052914340189, 0.000000000000000000 ) ) ;
#6934 = VECTOR ( 'NONE', #5925, 1000.000000000000000 ) ;
#6935 = CARTESIAN_POINT ( 'NONE',  ( 1.792916928892102080, -16.98383425522534651, 19.47783254395485031 ) ) ;
#6936 = ORIENTED_EDGE ( 'NONE', *, *, #30002, .F. ) ;
#6937 = EDGE_CURVE ( 'NONE', #22820, #27449, #11119, .T. ) ;
#6938 = CARTESIAN_POINT ( 'NONE',  ( 18.70942253818554235, -7.068249826530434099, 6.392525840300342210 ) ) ;
#6939 = CARTESIAN_POINT ( 'NONE',  ( 16.74328841314637017, 3.194145055459935545, 7.652108011868850923 ) ) ;
#6940 = DIRECTION ( 'NONE',  ( -0.000000000000000000, -0.000000000000000000, 1.000000000000000000 ) ) ;
#6941 = DIRECTION ( 'NONE',  ( 0.000000000000000000, 0.000000000000000000, -1.000000000000000000 ) ) ;
#6942 = ORIENTED_EDGE ( 'NONE', *, *, #6494, .F. ) ;
#6943 = AXIS2_PLACEMENT_3D ( 'NONE', #13435, #8277, #5776 ) ;
#6944 = FACE_OUTER_BOUND ( 'NONE', #6395, .T. ) ;
#6945 =( BOUNDED_CURVE ( )  B_SPLINE_CURVE ( 3, ( #19581, #28792, #3356, #703 ),
 .UNSPECIFIED., .F., .T. ) 
 B_SPLINE_CURVE_WITH_KNOTS ( ( 4, 4 ),
 ( 3.552344893626886879, 3.884040399493172036 ),
 .UNSPECIFIED. ) 
 CURVE ( )  GEOMETRIC_REPRESENTATION_ITEM ( )  RATIONAL_B_SPLINE_CURVE ( ( 1.000000000000000000, 0.9908525036704132205, 0.9908525036704132205, 1.000000000000000000 ) ) 
 REPRESENTATION_ITEM ( '' )  );
#6946 = CARTESIAN_POINT ( 'NONE',  ( -12.74661400762298413, 11.28197093999160394, 19.66962785902261857 ) ) ;
#6947 = CARTESIAN_POINT ( 'NONE',  ( -0.7083562926194498788, 9.056472324687613096, 21.50000000000000000 ) ) ;
#6948 = CARTESIAN_POINT ( 'NONE',  ( -9.169883732660077058, -9.268939115642981008, 1.500000000000001332 ) ) ;
#6949 = CARTESIAN_POINT ( 'NONE',  ( -24.03057240117691862, -26.57182937991349903, -6.500000000000000888 ) ) ;
#6950 = CARTESIAN_POINT ( 'NONE',  ( -15.30782679199506191, -7.476958555467157375, 20.29090034784956131 ) ) ;
#6951 = CARTESIAN_POINT ( 'NONE',  ( 32.44949699048088121, -8.540025205420070264, 37.20290368958222160 ) ) ;
#6952 = EDGE_LOOP ( 'NONE', ( #1891, #15604, #15143, #13862 ) ) ;
#6953 = ORIENTED_EDGE ( 'NONE', *, *, #11284, .T. ) ;
#6954 = LINE ( 'NONE', #28476, #11466 ) ;
#6955 = DIRECTION ( 'NONE',  ( -0.000000000000000000, -0.000000000000000000, -1.000000000000000000 ) ) ;
#6956 = DIRECTION ( 'NONE',  ( -0.000000000000000000, 0.000000000000000000, 1.000000000000000000 ) ) ;
#6957 = FACE_OUTER_BOUND ( 'NONE', #24210, .T. ) ;
#6958 = VERTEX_POINT ( 'NONE', #24979 ) ;
#6959 = DIRECTION ( 'NONE',  ( 0.000000000000000000, 0.000000000000000000, 1.000000000000000000 ) ) ;
#6960 = AXIS2_PLACEMENT_3D ( 'NONE', #23440, #13793, #4576 ) ;
#6961 = CARTESIAN_POINT ( 'NONE',  ( 4.996079307276527715, 16.27198743970617301, 6.420335371522007506 ) ) ;
#6962 = EDGE_CURVE ( 'NONE', #24520, #3590, #17589, .T. ) ;
#6963 = ORIENTED_EDGE ( 'NONE', *, *, #27505, .F. ) ;
#6964 = DIRECTION ( 'NONE',  ( 1.000000000000000000, 0.000000000000000000, 0.000000000000000000 ) ) ;
#6965 = CARTESIAN_POINT ( 'NONE',  ( 11.92830948316210993, 12.20365889974009477, 7.441806358946449151 ) ) ;
#6966 = EDGE_CURVE ( 'NONE', #28599, #10212, #21554, .T. ) ;
#6967 = VECTOR ( 'NONE', #23775, 1000.000000000000000 ) ;
#6968 = DIRECTION ( 'NONE',  ( -1.000000000000000000, 0.000000000000000000, 0.000000000000000000 ) ) ;
#6969 = CARTESIAN_POINT ( 'NONE',  ( -17.79898064049163153, 37.82295783581751891, 29.26401803458472628 ) ) ;
#6970 = ORIENTED_EDGE ( 'NONE', *, *, #4666, .T. ) ;
#6971 = CARTESIAN_POINT ( 'NONE',  ( 27.86235613436987890, -14.72519157938688927, 43.48653168448677064 ) ) ;
#6972 = DIRECTION ( 'NONE',  ( 0.000000000000000000, 0.000000000000000000, 1.000000000000000000 ) ) ;
#6973 = CARTESIAN_POINT ( 'NONE',  ( -14.69500743155267841, 13.56684717634543702, 6.386539667786089502 ) ) ;
#6974 = VERTEX_POINT ( 'NONE', #11105 ) ;
#6975 = CARTESIAN_POINT ( 'NONE',  ( -15.57452153527462535, -6.867569271111572782, 6.530762810602277924 ) ) ;
#6976 = LINE ( 'NONE', #19440, #9864 ) ;
#6977 = CARTESIAN_POINT ( 'NONE',  ( 25.41307773079511634, -6.523700759042267983, 44.52046879171659555 ) ) ;
#6978 = CARTESIAN_POINT ( 'NONE',  ( 21.79579286733899579, -37.18345238509958506, -16.49999999999999645 ) ) ;
#6979 = CARTESIAN_POINT ( 'NONE',  ( 0.1201197967225750701, -20.01774464624827132, 7.632642797338977658 ) ) ;
#6980 = VECTOR ( 'NONE', #21201, 1000.000000000000000 ) ;
#6981 = CARTESIAN_POINT ( 'NONE',  ( 0.000000000000000000, 0.000000000000000000, -87.50000000000000000 ) ) ;
#6982 = PLANE ( 'NONE',  #25503 ) ;
#6983 = CARTESIAN_POINT ( 'NONE',  ( 1.687027447297431371, 8.840471615930075799, 1.500000000000001332 ) ) ;
#6984 = CARTESIAN_POINT ( 'NONE',  ( -50.00000000000000000, 0.000000000000000000, 196.3477631085023631 ) ) ;
#6985 = ORIENTED_EDGE ( 'NONE', *, *, #8447, .F. ) ;
#6986 = CARTESIAN_POINT ( 'NONE',  ( -6.501324370950584353, 15.79217903278762947, 6.521906765011497242 ) ) ;
#6987 = CYLINDRICAL_SURFACE ( 'NONE', #29027, 0.7500000000000006661 ) ;
#6988 = ORIENTED_EDGE ( 'NONE', *, *, #21940, .T. ) ;
#6989 = EDGE_LOOP ( 'NONE', ( #30751, #6872, #30474, #19852 ) ) ;
#6990 = CARTESIAN_POINT ( 'NONE',  ( 4.800123045415256584, 19.41580659536132458, 18.47531940416305929 ) ) ;
#6991 = ORIENTED_EDGE ( 'NONE', *, *, #6301, .T. ) ;
#6992 = CARTESIAN_POINT ( 'NONE',  ( 15.19061449783604623, 13.03728791304909507, 20.25336174263950184 ) ) ;
#6993 = CARTESIAN_POINT ( 'NONE',  ( -3.993622308618941741, -8.159193615868385763, 21.50000000000000000 ) ) ;
#6994 = EDGE_LOOP ( 'NONE', ( #29128, #11345, #20847, #5572 ) ) ;
#6995 = CARTESIAN_POINT ( 'NONE',  ( 18.48560952955219960, -7.681425967031921154, 18.39992786714538298 ) ) ;
#6996 = CARTESIAN_POINT ( 'NONE',  ( 16.59873159789848529, 3.986191100139168775, 18.73743063545763121 ) ) ;
#6997 = AXIS2_PLACEMENT_3D ( 'NONE', #14940, #20229, #29136 ) ;
#6998 = EDGE_CURVE ( 'NONE', #2547, #6824, #13296, .T. ) ;
#6999 = DIRECTION ( 'NONE',  ( -0.000000000000000000, -0.000000000000000000, 1.000000000000000000 ) ) ;
#7000 = ADVANCED_FACE ( 'NONE', ( #12985 ), #22476, .T. ) ;
#7001 = EDGE_LOOP ( 'NONE', ( #8009, #6417, #3907, #18478 ) ) ;
#7002 = ADVANCED_FACE ( 'NONE', ( #25294 ), #22943, .T. ) ;
#7003 = ORIENTED_EDGE ( 'NONE', *, *, #10346, .T. ) ;
#7004 = EDGE_LOOP ( 'NONE', ( #12119, #28440, #2198, #26956, #22573 ) ) ;
#7005 = ORIENTED_EDGE ( 'NONE', *, *, #21517, .F. ) ;
#7006 = DIRECTION ( 'NONE',  ( -0.000000000000000000, 1.000000000000000000, -0.000000000000000000 ) ) ;
#7007 = CARTESIAN_POINT ( 'NONE',  ( 0.000000000000000000, -7.794228634059938265, -4.500000000000013323 ) ) ;
#7008 = CARTESIAN_POINT ( 'NONE',  ( 1.568770080425524904, -16.99791492429842066, 7.280727868105637768 ) ) ;
#7009 = DIRECTION ( 'NONE',  ( -0.000000000000000000, -0.000000000000000000, -1.000000000000000000 ) ) ;
#7010 = CARTESIAN_POINT ( 'NONE',  ( 1.305293688432930699, -17.01213356654596964, 20.24143955528809613 ) ) ;
#7011 = PLANE ( 'NONE',  #27825 ) ;
#7012 = EDGE_LOOP ( 'NONE', ( #23521, #6526, #22022, #1173 ) ) ;
#7013 = AXIS2_PLACEMENT_3D ( 'NONE', #18144, #10976, #29852 ) ;
#7014 = CARTESIAN_POINT ( 'NONE',  ( -16.82311188420106163, 2.597149461308117413, 19.00652017443069752 ) ) ;
#7015 = CARTESIAN_POINT ( 'NONE',  ( 15.62938862465957079, -35.64705970074183483, 34.49999999999999289 ) ) ;
#7016 = VECTOR ( 'NONE', #11366, 1000.000000000000000 ) ;
#7017 = DIRECTION ( 'NONE',  ( 1.000000000000000000, 0.000000000000000000, 0.000000000000000000 ) ) ;
#7018 = ORIENTED_EDGE ( 'NONE', *, *, #8039, .F. ) ;
#7019 = VERTEX_POINT ( 'NONE', #15461 ) ;
#7020 = DIRECTION ( 'NONE',  ( -1.000000000000000000, 0.000000000000000000, 0.000000000000000000 ) ) ;
#7021 = CARTESIAN_POINT ( 'NONE',  ( -19.64114023396061981, 37.13592150528867109, -1.500000000000009992 ) ) ;
#7022 = CARTESIAN_POINT ( 'NONE',  ( 39.99999999999998579, 90.00000000000001421, 17.49999999999999645 ) ) ;
#7023 = CARTESIAN_POINT ( 'NONE',  ( -5.905415913170754649, 19.12693415355693105, 18.34969686940295830 ) ) ;
#7024 = B_SPLINE_CURVE_WITH_KNOTS ( 'NONE', 3,
 ( #13310, #15953, #11120, #20614, #5976, #29848, #15475, #4093, #27960, #1136, #15318, #8318, #24993, #8767, #25144, #13625, #1610, #15631 ),
 .UNSPECIFIED., .F., .F.,
 ( 4, 2, 2, 2, 2, 2, 2, 2, 4 ),
 ( 0.000000000000000000, 0.0003967869494442882099, 0.0007935738988885764197, 0.001190360848332864575, 0.001587147797777152839, 0.001983934747221441103, 0.002380721696665729151, 0.002777508646110017632, 0.003174295595554305679 ),
 .UNSPECIFIED. ) ;
#7025 = CARTESIAN_POINT ( 'NONE',  ( -11.21147646446735102, 30.29926891764210595, 1.500000000000000000 ) ) ;
#7026 = LINE ( 'NONE', #28241, #25863 ) ;
#7027 = VERTEX_POINT ( 'NONE', #17978 ) ;
#7028 = CARTESIAN_POINT ( 'NONE',  ( -19.95437879344081367, 1.590546279198207680, 7.098451512883313441 ) ) ;
#7029 = CARTESIAN_POINT ( 'NONE',  ( 14.45728346696244593, 13.82012126338015712, 18.54958172136248606 ) ) ;
#7030 = CARTESIAN_POINT ( 'NONE',  ( 0.9621688436939443978, 9.033033306777458193, 21.50000000000000000 ) ) ;
#7031 = ORIENTED_EDGE ( 'NONE', *, *, #21011, .F. ) ;
#7032 = CARTESIAN_POINT ( 'NONE',  ( 49.99999999999998579, -50.00000000000000000, -92.50000000000000000 ) ) ;
#7033 = EDGE_LOOP ( 'NONE', ( #9419, #5578 ) ) ;
#7034 = CARTESIAN_POINT ( 'NONE',  ( 13.00999358272542850, -0.8602714556717643291, 1.500000000000001332 ) ) ;
#7035 = ADVANCED_FACE ( 'NONE', ( #10637 ), #30553, .T. ) ;
#7036 = AXIS2_PLACEMENT_3D ( 'NONE', #20472, #6440, #8626 ) ;
#7037 = CARTESIAN_POINT ( 'NONE',  ( 28.34828976096172681, -29.18752572968383419, -1.500000000000000000 ) ) ;
#7038 = VERTEX_POINT ( 'NONE', #20598 ) ;
#7039 = CARTESIAN_POINT ( 'NONE',  ( 33.69370807471729989, -13.92103290742843491, 27.50000000000000355 ) ) ;
#7040 = LINE ( 'NONE', #28566, #2313 ) ;
#7041 = DIRECTION ( 'NONE',  ( 0.000000000000000000, 0.000000000000000000, 1.000000000000000000 ) ) ;
#7042 = DIRECTION ( 'NONE',  ( -0.000000000000000000, -0.000000000000000000, 1.000000000000000000 ) ) ;
#7043 = CARTESIAN_POINT ( 'NONE',  ( -6.493275194760120606, 15.79517802630851797, 19.14333282897057842 ) ) ;
#7044 = CARTESIAN_POINT ( 'NONE',  ( -37.16608720827707657, -51.86186943028246787, 57.49999999999999289 ) ) ;
#7045 = CYLINDRICAL_SURFACE ( 'NONE', #18847, 1.000000000000008438 ) ;
#7046 = EDGE_LOOP ( 'NONE', ( #8082, #1320, #16805, #8146 ) ) ;
#7047 = AXIS2_PLACEMENT_3D ( 'NONE', #21147, #6816, #11656 ) ;
#7048 = DIRECTION ( 'NONE',  ( -1.000000000000000000, 0.000000000000000000, 0.000000000000000000 ) ) ;
#7049 = B_SPLINE_CURVE_WITH_KNOTS ( 'NONE', 3,
 ( #26222, #4860, #14374, #16872, #2527, #9691 ),
 .UNSPECIFIED., .F., .F.,
 ( 4, 2, 4 ),
 ( 0.001794032523744105035, 0.007046146517947431132, 0.01388807892444383733 ),
 .UNSPECIFIED. ) ;
#7050 = CARTESIAN_POINT ( 'NONE',  ( -25.19442432475839055, 35.44676296258369064, -19.50000000000000355 ) ) ;
#7051 = CARTESIAN_POINT ( 'NONE',  ( 24.03057240117691862, 26.57182937991349903, -1.500000000000001332 ) ) ;
#7052 = ORIENTED_EDGE ( 'NONE', *, *, #16994, .T. ) ;
#7053 = DIRECTION ( 'NONE',  ( 1.000000000000000000, 0.000000000000000000, 0.000000000000000000 ) ) ;
#7054 = DIRECTION ( 'NONE',  ( 0.000000000000000000, 0.000000000000000000, -1.000000000000000000 ) ) ;
#7055 = CARTESIAN_POINT ( 'NONE',  ( -3.858906612435654804, -7.730328572437724866, -3.621320343559650379 ) ) ;
#7056 = CARTESIAN_POINT ( 'NONE',  ( -8.884323311075783991, -1.438332125858144295, -1.500000000000001776 ) ) ;
#7057 = EDGE_CURVE ( 'NONE', #24048, #24781, #5156, .T. ) ;
#7058 = CARTESIAN_POINT ( 'NONE',  ( -23.20393738267338790, 0.000000000000000000, 1.500000000000000000 ) ) ;
#7059 = ORIENTED_EDGE ( 'NONE', *, *, #4057, .T. ) ;
#7060 = CARTESIAN_POINT ( 'NONE',  ( -15.26435939152463384, 8.070345032481604619, -0.6213203435596476032 ) ) ;
#7061 = CARTESIAN_POINT ( 'NONE',  ( 46.99999999999998579, 87.00000000000001421, 52.49999999999999289 ) ) ;
#7062 = EDGE_CURVE ( 'NONE', #26243, #466, #658, .T. ) ;
#7063 = CARTESIAN_POINT ( 'NONE',  ( 37.08686162832535871, 13.21332193651624110, 31.68138836149219628 ) ) ;
#7064 = DIRECTION ( 'NONE',  ( -0.000000000000000000, -0.000000000000000000, 1.000000000000000000 ) ) ;
#7065 = VERTEX_POINT ( 'NONE', #27637 ) ;
#7066 = CARTESIAN_POINT ( 'NONE',  ( 0.000000000000000000, 1.699320956058915452E-16, -1.500000000000001776 ) ) ;
#7067 = ORIENTED_EDGE ( 'NONE', *, *, #9731, .T. ) ;
#7068 = ADVANCED_FACE ( 'NONE', ( #1445 ), #6261, .F. ) ;
#7069 = CARTESIAN_POINT ( 'NONE',  ( -11.21147646446735102, -30.29926891764210595, 1.500000000000000000 ) ) ;
#7070 = CARTESIAN_POINT ( 'NONE',  ( 12.35846533491531041, 11.73919094685904696, 7.652108011868850923 ) ) ;
#7071 = ORIENTED_EDGE ( 'NONE', *, *, #20062, .T. ) ;
#7072 = ADVANCED_FACE ( 'NONE', ( #10958 ), #15302, .F. ) ;
#7073 = ORIENTED_EDGE ( 'NONE', *, *, #15862, .T. ) ;
#7074 = CARTESIAN_POINT ( 'NONE',  ( 2.959227181723801170, -8.499586724479446076, 1.500000000000001332 ) ) ;
#7075 = EDGE_CURVE ( 'NONE', #12516, #28935, #3617, .T. ) ;
#7076 = VECTOR ( 'NONE', #30306, 1000.000000000000000 ) ;
#7077 = ORIENTED_EDGE ( 'NONE', *, *, #11266, .T. ) ;
#7078 = ORIENTED_EDGE ( 'NONE', *, *, #17433, .T. ) ;
#7079 = CARTESIAN_POINT ( 'NONE',  ( -0.1401636875787321268, -17.02258069761206372, 19.77662771831109367 ) ) ;
#7080 = EDGE_CURVE ( 'NONE', #10893, #19850, #29568, .T. ) ;
#7081 = CARTESIAN_POINT ( 'NONE',  ( -9.908187358984022808, -17.39367339311967342, 7.366751648393900176 ) ) ;
#7082 = CIRCLE ( 'NONE', #13019, 0.7500000000000006661 ) ;
#7083 = DIRECTION ( 'NONE',  ( 1.000000000000000000, 0.000000000000000000, 0.000000000000000000 ) ) ;
#7084 = EDGE_CURVE ( 'NONE', #9428, #27809, #28090, .T. ) ;
#7085 = CARTESIAN_POINT ( 'NONE',  ( 1.153863525602932150, -19.98436899483067819, 18.73743063545763121 ) ) ;
#7086 = EDGE_LOOP ( 'NONE', ( #5244, #3291, #30213, #8621 ) ) ;
#7087 = LINE ( 'NONE', #19092, #17815 ) ;
#7088 = EDGE_CURVE ( 'NONE', #18831, #26574, #6715, .T. ) ;
#7089 = LINE ( 'NONE', #7714, #22333 ) ;
#7090 = CARTESIAN_POINT ( 'NONE',  ( 11.67039530559478777, 12.46804495696167336, 19.14333282897057842 ) ) ;
#7091 = DIRECTION ( 'NONE',  ( 1.000000000000000000, 0.000000000000000000, 0.000000000000000000 ) ) ;
#7092 = ORIENTED_EDGE ( 'NONE', *, *, #28945, .T. ) ;
#7093 = LINE ( 'NONE', #4906, #9399 ) ;
#7094 = CARTESIAN_POINT ( 'NONE',  ( -15.01497154418444602, -8.089954645606729500, 5.704143890883081269 ) ) ;
#7095 = DIRECTION ( 'NONE',  ( -1.000000000000000000, 0.000000000000000000, 0.000000000000000000 ) ) ;
#7096 = AXIS2_PLACEMENT_3D ( 'NONE', #14892, #24401, #3045 ) ;
#7097 = CARTESIAN_POINT ( 'NONE',  ( -19.90131041440201187, 1.988107338454515149, 5.779535427900759359 ) ) ;
#7098 = CARTESIAN_POINT ( 'NONE',  ( -18.09892777451933910, -8.511549950051179536, 18.34726407865099418 ) ) ;
#7099 = VECTOR ( 'NONE', #1512, 1000.000000000000114 ) ;
#7100 = DIRECTION ( 'NONE',  ( 0.7557495743542582689, -0.6548607339452851006, 0.000000000000000000 ) ) ;
#7101 = FACE_OUTER_BOUND ( 'NONE', #7291, .T. ) ;
#7102 = ORIENTED_EDGE ( 'NONE', *, *, #18495, .F. ) ;
#7103 = VERTEX_POINT ( 'NONE', #16226 ) ;
#7104 = DIRECTION ( 'NONE',  ( 0.000000000000000000, -0.000000000000000000, -1.000000000000000000 ) ) ;
#7105 = CARTESIAN_POINT ( 'NONE',  ( -5.105024945675580739, -42.22604126506273303, -1.500000000000000000 ) ) ;
#7106 = EDGE_CURVE ( 'NONE', #6203, #699, #17114, .T. ) ;
#7107 = CARTESIAN_POINT ( 'NONE',  ( -1.073881485057447405, -0.9711784013058452070, 1.500000000000000000 ) ) ;
#7108 = EDGE_CURVE ( 'NONE', #5078, #23472, #13643, .T. ) ;
#7109 = CARTESIAN_POINT ( 'NONE',  ( -50.00000000000000000, 87.00000000000001421, 22.49999999999999289 ) ) ;
#7110 = ORIENTED_EDGE ( 'NONE', *, *, #26877, .T. ) ;
#7111 = DIRECTION ( 'NONE',  ( 1.000000000000000000, 0.000000000000000000, 0.000000000000000000 ) ) ;
#7112 = CARTESIAN_POINT ( 'NONE',  ( 15.40995608898784397, -7.231564984717127054, 19.00652017443069752 ) ) ;
#7113 = EDGE_CURVE ( 'NONE', #13970, #2231, #24075, .T. ) ;
#7114 = CARTESIAN_POINT ( 'NONE',  ( 5.409330662328856398, 19.27307614344555375, 5.657991946698900598 ) ) ;
#7115 = ORIENTED_EDGE ( 'NONE', *, *, #19265, .F. ) ;
#7116 = CARTESIAN_POINT ( 'NONE',  ( 5.730668117466260369, 19.18033075515274888, 20.25336174263950184 ) ) ;
#7117 = EDGE_CURVE ( 'NONE', #27891, #12561, #1669, .T. ) ;
#7118 = LINE ( 'NONE', #245, #7269 ) ;
#7119 = DIRECTION ( 'NONE',  ( -1.000000000000000000, 0.000000000000000000, 0.000000000000000000 ) ) ;
#7120 = CARTESIAN_POINT ( 'NONE',  ( -23.38069191132970204, 29.32513219524850001, 37.49999999996538236 ) ) ;
#7121 = ORIENTED_EDGE ( 'NONE', *, *, #9417, .F. ) ;
#7122 = LINE ( 'NONE', #28643, #22313 ) ;
#7123 = VECTOR ( 'NONE', #8244, 1000.000000000000000 ) ;
#7124 = EDGE_CURVE ( 'NONE', #27347, #13900, #23234, .T. ) ;
#7125 = AXIS2_PLACEMENT_3D ( 'NONE', #20307, #1283, #5964 ) ;
#7126 = LINE ( 'NONE', #11795, #9071 ) ;
#7127 = CARTESIAN_POINT ( 'NONE',  ( -23.96732207938974213, -33.98584080153308662, -1.500000000000000000 ) ) ;
#7128 = VERTEX_POINT ( 'NONE', #13895 ) ;
#7129 = SHAPE_REPRESENTATION ( 'Front & Rear Ported Pressure', ( #7396 ), #910 ) ;
#7130 = CARTESIAN_POINT ( 'NONE',  ( -15.57976790534003086, -6.855017190910956515, 6.641371103590088865 ) ) ;
#7131 = PLANE ( 'NONE',  #28789 ) ;
#7132 = CARTESIAN_POINT ( 'NONE',  ( -23.07950435457351190, 11.50806656539842798, 49.21048435262080289 ) ) ;
#7133 = CARTESIAN_POINT ( 'NONE',  ( 0.3158150563615996775, -20.01532941283344513, 5.651989602109218858 ) ) ;
#7134 = B_SPLINE_CURVE_WITH_KNOTS ( 'NONE', 3,
 ( #4903, #14421, #11615, #14093 ),
 .UNSPECIFIED., .F., .F.,
 ( 4, 4 ),
 ( 3.022186913359086288E-07, 0.007932103869840195776 ),
 .UNSPECIFIED. ) ;
#7135 = CARTESIAN_POINT ( 'NONE',  ( 66.99999999999998579, -50.00000000000000000, 59.49999999999999289 ) ) ;
#7136 = LINE ( 'NONE', #23642, #26997 ) ;
#7137 = CARTESIAN_POINT ( 'NONE',  ( -17.04815991962219357, 0.8662532504481892381, 19.97651184436794125 ) ) ;
#7138 = DIRECTION ( 'NONE',  ( 0.000000000000000000, 0.000000000000000000, 1.000000000000000000 ) ) ;
#7139 = VERTEX_POINT ( 'NONE', #15940 ) ;
#7140 = EDGE_CURVE ( 'NONE', #1105, #16393, #25583, .T. ) ;
#7141 = ADVANCED_FACE ( 'NONE', ( #20742 ), #11705, .T. ) ;
#7142 = CARTESIAN_POINT ( 'NONE',  ( 11.23845335764779563, -16.56542118924666340, 20.33971507717571114 ) ) ;
#7143 = FACE_OUTER_BOUND ( 'NONE', #688, .T. ) ;
#7144 = ORIENTED_EDGE ( 'NONE', *, *, #23562, .F. ) ;
#7145 = ORIENTED_EDGE ( 'NONE', *, *, #9213, .F. ) ;
#7146 = AXIS2_PLACEMENT_3D ( 'NONE', #25096, #30235, #5919 ) ;
#7147 = CARTESIAN_POINT ( 'NONE',  ( 4.434078574240014170, 19.50234843602376955, 18.84486140012300126 ) ) ;
#7148 = DIRECTION ( 'NONE',  ( 0.000000000000000000, 0.000000000000000000, -1.000000000000000000 ) ) ;
#7149 = ORIENTED_EDGE ( 'NONE', *, *, #27118, .T. ) ;
#7150 = DIRECTION ( 'NONE',  ( -1.000000000000000000, 0.000000000000000000, 0.000000000000000000 ) ) ;
#7151 = CARTESIAN_POINT ( 'NONE',  ( -10.52692833102915770, -17.02631732661572883, 7.652108011868850035 ) ) ;
#7152 = ORIENTED_EDGE ( 'NONE', *, *, #9031, .T. ) ;
#7153 = CARTESIAN_POINT ( 'NONE',  ( 18.70304204834580020, -7.134633872344113392, 18.92976555901915603 ) ) ;
#7154 = CARTESIAN_POINT ( 'NONE',  ( 19.59419491516168321, 4.095680178559272022, 19.79423548914561692 ) ) ;
#7155 = CARTESIAN_POINT ( 'NONE',  ( -26.12047388987420149, 6.311255530320346807, 48.12792051007069460 ) ) ;
#7156 = ORIENTED_EDGE ( 'NONE', *, *, #5428, .T. ) ;
#7157 = CARTESIAN_POINT ( 'NONE',  ( 15.47543066139447987, -7.098048983848884497, 19.96344307082653202 ) ) ;
#7158 = ORIENTED_EDGE ( 'NONE', *, *, #770, .F. ) ;
#7159 = AXIS2_PLACEMENT_3D ( 'NONE', #26183, #23382, #14023 ) ;
#7160 = ORIENTED_EDGE ( 'NONE', *, *, #7282, .F. ) ;
#7161 = VECTOR ( 'NONE', #21944, 1000.000000000000227 ) ;
#7162 = AXIS2_PLACEMENT_3D ( 'NONE', #17864, #18323, #22668 ) ;
#7163 = CARTESIAN_POINT ( 'NONE',  ( 0.000000000000000000, 0.000000000000000000, 34.49999999999999289 ) ) ;
#7164 = CARTESIAN_POINT ( 'NONE',  ( 0.09252763182292866873, -8.674330214978059672, -2.975619346028175904 ) ) ;
#7165 = CARTESIAN_POINT ( 'NONE',  ( 0.9820204223201481897, -19.99380624802878970, 7.441806358946449151 ) ) ;
#7166 = CARTESIAN_POINT ( 'NONE',  ( -14.80112376877043445, -8.505769479261473975, 19.96568007040468373 ) ) ;
#7167 = CARTESIAN_POINT ( 'NONE',  ( -23.36055057548231062, 12.54866584153426601, 48.48250221505454505 ) ) ;
#7168 = CARTESIAN_POINT ( 'NONE',  ( 16.74864137134695596, 3.161078882829539971, 18.34777357837152323 ) ) ;
#7169 = ORIENTED_EDGE ( 'NONE', *, *, #19874, .F. ) ;
#7170 = CARTESIAN_POINT ( 'NONE',  ( -8.197313248159920462, 3.914781618004780306, 13.22130136205108819 ) ) ;
#7171 = CARTESIAN_POINT ( 'NONE',  ( -14.58213539500865785, 7.758783772730382111, 24.50000000000000000 ) ) ;
#7172 = FACE_OUTER_BOUND ( 'NONE', #27412, .T. ) ;
#7173 = EDGE_LOOP ( 'NONE', ( #5593, #28664, #26099, #21695 ) ) ;
#7174 = ORIENTED_EDGE ( 'NONE', *, *, #27712, .T. ) ;
#7175 = CARTESIAN_POINT ( 'NONE',  ( 0.000000000000000000, 42.50000000000000000, 24.50000000000000000 ) ) ;
#7176 = CARTESIAN_POINT ( 'NONE',  ( 20.47140923013457936, -25.96617498784419098, -16.50001200000000168 ) ) ;
#7177 = FACE_OUTER_BOUND ( 'NONE', #18355, .T. ) ;
#7178 = PRODUCT_DEFINITION_SHAPE ( 'NONE', 'NONE',  #30860 ) ;
#7179 = DIRECTION ( 'NONE',  ( 0.000000000000000000, -1.000000000000000000, 0.000000000000000000 ) ) ;
#7180 = CARTESIAN_POINT ( 'NONE',  ( 17.84153987719590972, -14.83584055149750114, -1.500000000000000000 ) ) ;
#7181 = CARTESIAN_POINT ( 'NONE',  ( -22.64188265567332436, -30.81688647342193121, 27.50000000000000711 ) ) ;
#7182 = AXIS2_PLACEMENT_3D ( 'NONE', #10131, #24478, #3122 ) ;
#7183 = CARTESIAN_POINT ( 'NONE',  ( -5.719992972340618209, 19.16498258860014658, 7.626647697317578967 ) ) ;
#7184 = ORIENTED_EDGE ( 'NONE', *, *, #11481, .F. ) ;
#7185 = CARTESIAN_POINT ( 'NONE',  ( -2.048514414209405832, -39.45186992530642556, 34.50000000000000711 ) ) ;
#7186 = CARTESIAN_POINT ( 'NONE',  ( -17.59389297287863840, -9.510918850537244396, 19.08830981656263859 ) ) ;
#7187 = DIRECTION ( 'NONE',  ( 1.000000000000000000, 0.000000000000000000, 0.000000000000000000 ) ) ;
#7188 = ORIENTED_EDGE ( 'NONE', *, *, #7969, .F. ) ;
#7189 = FACE_OUTER_BOUND ( 'NONE', #18774, .T. ) ;
#7190 = ORIENTED_EDGE ( 'NONE', *, *, #28306, .F. ) ;
#7191 = CARTESIAN_POINT ( 'NONE',  ( 16.11353791281288395, -5.634185590772410990, 7.280727868105637768 ) ) ;
#7192 = DIRECTION ( 'NONE',  ( 1.000000000000000000, 0.000000000000000000, 0.000000000000000000 ) ) ;
#7193 = ORIENTED_EDGE ( 'NONE', *, *, #20037, .F. ) ;
#7194 = CARTESIAN_POINT ( 'NONE',  ( 3.101722653984818834, 39.35894504374194014, 27.49999999999999645 ) ) ;
#7195 = APPLICATION_CONTEXT ( 'automotive_design' ) ;
#7196 = DIRECTION ( 'NONE',  ( -0.000000000000000000, -0.000000000000000000, 1.000000000000000000 ) ) ;
#7197 = CARTESIAN_POINT ( 'NONE',  ( -18.04156136322729864, -8.631457789788587576, 5.652196082369963293 ) ) ;
#7198 = CIRCLE ( 'NONE', #16158, 0.7500000000000006661 ) ;
#7199 = CARTESIAN_POINT ( 'NONE',  ( 4.510281037539698445E-13, -4.926614671774132148E-13, 79.49999999999998579 ) ) ;
#7200 = CARTESIAN_POINT ( 'NONE',  ( 4.510281037539698445E-13, -4.926614671774132148E-13, 62.49999999999999289 ) ) ;
#7201 = ORIENTED_EDGE ( 'NONE', *, *, #21993, .T. ) ;
#7202 = CARTESIAN_POINT ( 'NONE',  ( 15.76152542347981900, -6.481515897568145057, 5.651492010659114662 ) ) ;
#7203 = CARTESIAN_POINT ( 'NONE',  ( 12.56641067637628240, -40.32935944494942504, -1.500000000000000000 ) ) ;
#7204 = CARTESIAN_POINT ( 'NONE',  ( 0.000000000000000000, -2.322405306613848348E-14, 117.5000000000000000 ) ) ;
#7205 = ORIENTED_EDGE ( 'NONE', *, *, #27671, .T. ) ;
#7206 = CARTESIAN_POINT ( 'NONE',  ( 8.099999999999999645, 0.000000000000000000, 0.000000000000000000 ) ) ;
#7207 = CARTESIAN_POINT ( 'NONE',  ( -17.61017686385352121, -9.517781650307574282, 19.58863275299554019 ) ) ;
#7208 = DIRECTION ( 'NONE',  ( 0.9898214418809327952, -0.1423148382732850048, 0.000000000000000000 ) ) ;
#7209 = CYLINDRICAL_SURFACE ( 'NONE', #7312, 0.7500000000000011102 ) ;
#7210 = CARTESIAN_POINT ( 'NONE',  ( -33.56615453960540663, 10.45399542313511354, 35.60128781019762556 ) ) ;
#7211 = VERTEX_POINT ( 'NONE', #16533 ) ;
#7212 =( NAMED_UNIT ( * ) PLANE_ANGLE_UNIT ( ) SI_UNIT ( $, .RADIAN. ) );
#7213 = CARTESIAN_POINT ( 'NONE',  ( 25.41822862649771508, 27.59854655694143588, 37.49999999990964028 ) ) ;
#7214 = CARTESIAN_POINT ( 'NONE',  ( -11.40980092660686829, 6.310027164379044429, 1.500000000000001332 ) ) ;
#7215 = ORIENTED_EDGE ( 'NONE', *, *, #6108, .F. ) ;
#7216 = CARTESIAN_POINT ( 'NONE',  ( -26.44644203219470668, 9.801837641955994940, -1.500000000000000000 ) ) ;
#7217 = ORIENTED_EDGE ( 'NONE', *, *, #130, .T. ) ;
#7218 = CARTESIAN_POINT ( 'NONE',  ( -15.34307810681595186, 12.82926163924265950, 20.34789198813115263 ) ) ;
#7219 = CARTESIAN_POINT ( 'NONE',  ( 0.000000000000000000, 0.000000000000000000, 1.500000000000001332 ) ) ;
#7220 = ORIENTED_EDGE ( 'NONE', *, *, #28234, .T. ) ;
#7221 = AXIS2_PLACEMENT_3D ( 'NONE', #28946, #12883, #10378 ) ;
#7222 = EDGE_LOOP ( 'NONE', ( #2950, #29909 ) ) ;
#7223 = CARTESIAN_POINT ( 'NONE',  ( 0.000000000000000000, 0.000000000000000000, -87.50000000000000000 ) ) ;
#7224 = VERTEX_POINT ( 'NONE', #3 ) ;
#7225 = ORIENTED_EDGE ( 'NONE', *, *, #1936, .T. ) ;
#7226 = CARTESIAN_POINT ( 'NONE',  ( -0.6606983433884117130, -20.00701505202155062, 19.45164628100866722 ) ) ;
#7227 = CARTESIAN_POINT ( 'NONE',  ( -8.006961111548653420, -15.06991809617584899, 7.441806358946449151 ) ) ;
#7228 = CARTESIAN_POINT ( 'NONE',  ( 0.000000000000000000, 1.699320956058915452E-16, -1.500000000000001776 ) ) ;
#7229 = CARTESIAN_POINT ( 'NONE',  ( 30.75232512042845556, -9.966982604840845639, -1.500000000000000000 ) ) ;
#7230 = ORIENTED_EDGE ( 'NONE', *, *, #4646, .F. ) ;
#7231 = EDGE_CURVE ( 'NONE', #15032, #5400, #23690, .T. ) ;
#7232 = DIRECTION ( 'NONE',  ( 1.000000000000000000, 0.000000000000000000, 0.000000000000000000 ) ) ;
#7233 = CARTESIAN_POINT ( 'NONE',  ( 23.11204207310333203, 35.56592875157961231, -11.49994540239372043 ) ) ;
#7234 = CARTESIAN_POINT ( 'NONE',  ( 11.65818676052302294, 12.48028922388247253, 19.25672174529527325 ) ) ;
#7235 = FACE_OUTER_BOUND ( 'NONE', #5911, .T. ) ;
#7236 = ORIENTED_EDGE ( 'NONE', *, *, #15125, .F. ) ;
#7237 = PRODUCT_RELATED_PRODUCT_CATEGORY ( 'part', '', ( #4681 ) ) ;
#7238 = CIRCLE ( 'NONE', #1816, 0.7500000000000007772 ) ;
#7239 = FACE_OUTER_BOUND ( 'NONE', #3456, .T. ) ;
#7240 = CARTESIAN_POINT ( 'NONE',  ( -15.09693789817080578, -7.923486267757679613, 5.661398277488802755 ) ) ;
#7241 = CARTESIAN_POINT ( 'NONE',  ( 12.24063095261064404, 4.490763173670002217, 24.50000000000000000 ) ) ;
#7242 = CIRCLE ( 'NONE', #256, 20.00000000000000000 ) ;
#7243 = CARTESIAN_POINT ( 'NONE',  ( -37.16608720827707657, 65.00000000000000000, 57.49999999999999289 ) ) ;
#7244 = CARTESIAN_POINT ( 'NONE',  ( 19.78395057425408154, 2.934310293824245353, 7.626647697317575414 ) ) ;
#7245 = EDGE_CURVE ( 'NONE', #3543, #29877, #21049, .T. ) ;
#7246 = DIRECTION ( 'NONE',  ( 0.7416830501633145944, 0.6707505147970012072, -0.000000000000000000 ) ) ;
#7247 = DIRECTION ( 'NONE',  ( 0.000000000000000000, 0.000000000000000000, 1.000000000000000000 ) ) ;
#7248 = ORIENTED_EDGE ( 'NONE', *, *, #18369, .T. ) ;
#7249 = ORIENTED_EDGE ( 'NONE', *, *, #12056, .T. ) ;
#7250 = DIRECTION ( 'NONE',  ( -0.000000000000000000, -0.000000000000000000, -1.000000000000000000 ) ) ;
#7251 = CARTESIAN_POINT ( 'NONE',  ( -8.321991900972895095, -14.88664253267596571, 5.653604225791663218 ) ) ;
#7252 = DIRECTION ( 'NONE',  ( 0.6707505147970010961, -0.7416830501633147055, 0.000000000000000000 ) ) ;
#7253 = FACE_OUTER_BOUND ( 'NONE', #5138, .T. ) ;
#7254 = EDGE_LOOP ( 'NONE', ( #24570, #28698, #5501, #22453 ) ) ;
#7255 = CONTEXT_DEPENDENT_SHAPE_REPRESENTATION ( #58, #21622 ) ;
#7256 = CARTESIAN_POINT ( 'NONE',  ( 18.05043922081454610, -8.654756627348808351, 20.05479082170252525 ) ) ;
#7257 = EDGE_CURVE ( 'NONE', #15581, #52, #15103, .T. ) ;
#7258 = CIRCLE ( 'NONE', #24685, 11.46182693247435935 ) ;
#7259 = CARTESIAN_POINT ( 'NONE',  ( 5.818449564404023278, 19.15386117387415510, 5.796888747622817029 ) ) ;
#7260 = EDGE_CURVE ( 'NONE', #9004, #29934, #11139, .T. ) ;
#7261 = EDGE_LOOP ( 'NONE', ( #23466, #16193, #19574, #21807 ) ) ;
#7262 = LINE ( 'NONE', #19270, #7315 ) ;
#7263 = CARTESIAN_POINT ( 'NONE',  ( 11.86828576611216235, 12.26598719735377863, 7.366751648393900176 ) ) ;
#7264 = B_SPLINE_CURVE_WITH_KNOTS ( 'NONE', 3,
 ( #5652, #5802, #5334, #10021, #1121, #14686, #10634, #21867, #17031, #3154, #12983, #20146, #19529, #15147, #24508, #14843, #17656, #5495 ),
 .UNSPECIFIED., .F., .F.,
 ( 4, 2, 2, 2, 2, 2, 2, 2, 4 ),
 ( 0.003174295595554332567, 0.003570702171545570534, 0.003967108747536808935, 0.004363515323528046469, 0.004759921899519284870, 0.005156328475510523271, 0.005552735051501760805, 0.005949141627492998338, 0.006345548203484236739 ),
 .UNSPECIFIED. ) ;
#7265 = CARTESIAN_POINT ( 'NONE',  ( -10.29532059365457108, -42.63824274976927597, -16.49999999999999645 ) ) ;
#7266 = CARTESIAN_POINT ( 'NONE',  ( -37.98255541114690459, 9.730631687238020078, 31.92508531691350981 ) ) ;
#7267 = ORIENTED_EDGE ( 'NONE', *, *, #26959, .F. ) ;
#7268 = CARTESIAN_POINT ( 'NONE',  ( 0.000000000000000000, 1.699320956058915452E-16, -1.500000000000001776 ) ) ;
#7269 = VECTOR ( 'NONE', #14444, 1000.000000000000000 ) ;
#7270 = CARTESIAN_POINT ( 'NONE',  ( 6.630478080506912342, 6.778663211761485563, 13.00000000000000178 ) ) ;
#7271 = CIRCLE ( 'NONE', #22689, 0.7500000000000004441 ) ;
#7272 = FACE_OUTER_BOUND ( 'NONE', #15628, .T. ) ;
#7273 = ORIENTED_EDGE ( 'NONE', *, *, #25991, .T. ) ;
#7274 = CARTESIAN_POINT ( 'NONE',  ( -15.42813811594282036, -7.209250886987519813, 5.862424720655265098 ) ) ;
#7275 = CARTESIAN_POINT ( 'NONE',  ( -12.86767874445213877, -1.850092897552710225, 24.50000000000000000 ) ) ;
#7276 = AXIS2_PLACEMENT_3D ( 'NONE', #12882, #24708, #20497 ) ;
#7277 = EDGE_CURVE ( 'NONE', #23361, #21731, #16384, .T. ) ;
#7278 = DIRECTION ( 'NONE',  ( -0.000000000000000000, -0.000000000000000000, -1.000000000000000000 ) ) ;
#7279 = EDGE_CURVE ( 'NONE', #17105, #13217, #15621, .T. ) ;
#7280 = DIRECTION ( 'NONE',  ( 0.000000000000000000, -1.132880637372608986E-16, 1.000000000000000000 ) ) ;
#7281 = CIRCLE ( 'NONE', #24709, 15.00000000000003553 ) ;
#7282 = EDGE_CURVE ( 'NONE', #9215, #23733, #21584, .T. ) ;
#7283 = DIRECTION ( 'NONE',  ( 0.000000000000000000, -1.132880637372608986E-16, 1.000000000000000000 ) ) ;
#7284 = CARTESIAN_POINT ( 'NONE',  ( 1.000000000000008438, 19.97498435543819184, 1.500000000000001332 ) ) ;
#7285 = CARTESIAN_POINT ( 'NONE',  ( -19.96188467872886463, 1.492656647078444809, 19.47783254395485031 ) ) ;
#7286 = ORIENTED_EDGE ( 'NONE', *, *, #6854, .T. ) ;
#7287 = EDGE_CURVE ( 'NONE', #6669, #203, #18102, .T. ) ;
#7288 = CARTESIAN_POINT ( 'NONE',  ( 11.92709382895865566, -16.07640909887372516, 19.58863275299554019 ) ) ;
#7289 = DIRECTION ( 'NONE',  ( 0.000000000000000000, 0.000000000000000000, -1.000000000000000000 ) ) ;
#7290 = ORIENTED_EDGE ( 'NONE', *, *, #6157, .F. ) ;
#7291 = EDGE_LOOP ( 'NONE', ( #19300, #5972, #16929, #4728, #29965, #15753, #7700 ) ) ;
#7292 = EDGE_CURVE ( 'NONE', #17125, #1255, #15622, .T. ) ;
#7293 = AXIS2_PLACEMENT_3D ( 'NONE', #29152, #7785, #17298 ) ;
#7294 = CARTESIAN_POINT ( 'NONE',  ( -49.67292458505995256, 69.99754304297013618, 55.05739345352110803 ) ) ;
#7295 = EDGE_CURVE ( 'NONE', #25948, #8229, #22072, .T. ) ;
#7296 = CARTESIAN_POINT ( 'NONE',  ( -12.73895949420588458, 48.35079126656098225, -47.06516019132716622 ) ) ;
#7297 = B_SPLINE_CURVE_WITH_KNOTS ( 'NONE', 3,
 ( #6575, #1599, #7183, #26053, #16852, #24158, #2191, #2340, #16387, #14507, #26368, #26203, #26517, #21195, #153, #9674, #9369, #19183 ),
 .UNSPECIFIED., .F., .F.,
 ( 4, 2, 2, 2, 2, 2, 2, 2, 4 ),
 ( 0.003174295595554313485, 0.003570702171545544080, 0.003967108747536775108, 0.004363515323528005703, 0.004759921899519236298, 0.005156328475510467760, 0.005552735051501698355, 0.005949141627492928949, 0.006345548203484159544 ),
 .UNSPECIFIED. ) ;
#7298 = CIRCLE ( 'NONE', #9341, 0.6002263538043630664 ) ;
#7299 = FACE_OUTER_BOUND ( 'NONE', #10670, .T. ) ;
#7300 = VERTEX_POINT ( 'NONE', #305 ) ;
#7301 = AXIS2_PLACEMENT_3D ( 'NONE', #4343, #9039, #6232 ) ;
#7302 = DIRECTION ( 'NONE',  ( 1.000000000000000000, 0.000000000000000000, 0.000000000000000000 ) ) ;
#7303 = DIRECTION ( 'NONE',  ( 1.000000000000000000, 1.776356839400250465E-15, 0.000000000000000000 ) ) ;
#7304 = VERTEX_POINT ( 'NONE', #12018 ) ;
#7305 = CARTESIAN_POINT ( 'NONE',  ( 18.44211820063743446, -7.784504718833766823, 18.37415474056476938 ) ) ;
#7306 = DIRECTION ( 'NONE',  ( -0.7416830501633076000, -0.6707505147970089787, 0.000000000000000000 ) ) ;
#7307 = VECTOR ( 'NONE', #17064, 1000.000000000000000 ) ;
#7308 = FACE_OUTER_BOUND ( 'NONE', #1251, .T. ) ;
#7309 =( BOUNDED_SURFACE ( )  B_SPLINE_SURFACE ( 3, 2, ( 
 ( #15183, #25168, #29703 ),
 ( #22667, #17392, #26914 ),
 ( #8515, #8347, #27527 ),
 ( #3347, #3812, #13335 ),
 ( #17543, #22832, #19719 ),
 ( #12879, #5535, #15035 ),
 ( #27062, #24550, #10374 ),
 ( #24705, #22378, #10522 ),
 ( #2070, #20642, #20936 ),
 ( #18620, #20494, #25643 ),
 ( #9103, #6610, #25938 ),
 ( #4259, #4570, #16125 ),
 ( #4420, #27980, #28291 ),
 ( #6300, #13787, #14073 ),
 ( #18772, #27672, #30607 ),
 ( #6465, #25333, #23284 ),
 ( #13494, #6917, #8794 ),
 ( #16427, #15813, #15973 ),
 ( #28132, #30460, #30314 ),
 ( #3974, #1926, #11451 ),
 ( #6756, #16271, #25794 ),
 ( #13935, #23432, #22978 ),
 ( #11145, #11593, #11293 ),
 ( #8961, #13648, #21087 ),
 ( #1483, #1634, #9253 ),
 ( #10995, #30161, #30015 ),
 ( #8656, #18320, #18164 ),
 ( #27836, #25493, #4118 ),
 ( #20789, #23130, #1775 ),
 ( #18476, #19215, #21552 ),
 ( #29049, #14394, #23735 ),
 ( #12369, #26709, #30770 ),
 ( #21238, #18933, #7536 ),
 ( #2847, #9868, #23901 ),
 ( #19069, #5188, #9416 ),
 ( #24194, #14690, #2692 ),
 ( #28438, #16727, #14548 ),
 ( #2544, #21405, #12203 ),
 ( #7063, #26239, #21871 ),
 ( #12060, #47, #19383 ),
 ( #28588, #9557, #28901 ),
 ( #26561, #505, #11914 ),
 ( #7690, #17037, #11744 ),
 ( #2387, #344, #28744 ),
 ( #7382, #4878, #10025 ),
 ( #21703, #19534, #14222 ),
 ( #16571, #26088, #17189 ),
 ( #5338, #23582, #7213 ),
 ( #188, #9705, #4720 ),
 ( #2225, #16890, #26409 ),
 ( #5035, #24046, #19678 ),
 ( #1285, #12836, #10640 ),
 ( #15150, #3620, #29366 ),
 ( #8307, #17507, #8005 ),
 ( #27027, #20150, #24837 ),
 ( #26876, #22338, #1125 ),
 ( #14849, #5655, #10171 ),
 ( #24669, #3473, #19997 ),
 ( #976, #29668, #17824 ),
 ( #3307, #29200, #10486 ) ),
 .UNSPECIFIED., .F., .F., .T. ) 
 B_SPLINE_SURFACE_WITH_KNOTS ( ( 4, 2, 2, 2, 2, 2, 2, 2, 2, 2, 2, 2, 2, 2, 2, 2, 2, 2, 2, 2, 2, 2, 2, 2, 2, 2, 2, 2, 2, 4 ),
 ( 3, 3 ),
 ( 0.09646856835573283662, 0.09948321111685021201, 0.1009905324974089136, 0.1024978538779676013, 0.1085271394002023659, 0.1100344607807610675, 0.1115417821613197552, 0.1145564249224371445, 0.1175710676835545199, 0.1205857104446719091, 0.1266149959669066738, 0.1326442814891414523, 0.1356589242502588277, 0.1386735670113762309, 0.1447028525336109817, 0.1477174952947283570, 0.1492248166752870309, 0.1507321380558457324, 0.1567614235780805110, 0.1597760663391978864, 0.1627907091003152895, 0.1688199946225500403, 0.1703273160031087419, 0.1718346373836674157, 0.1748492801447847911, 0.1808785656670195696, 0.1823858870475782434, 0.1838932084281369450, 0.1869078511892543482, 0.1929371367114890989 ),
 ( 0.000000000000000000, 1.000000000000000000 ),
 .UNSPECIFIED. ) 
 GEOMETRIC_REPRESENTATION_ITEM ( )  RATIONAL_B_SPLINE_SURFACE ( (
 ( 1.000000000000000000, 0.8675417673879289859, 1.000000000000000000),
 ( 1.000000000000000000, 0.8667209715531846159, 1.000000000000000000),
 ( 1.000000000000000000, 0.8662263239862698638, 1.000000000000000000),
 ( 1.000000000000000000, 0.8659995305180094860, 1.000000000000000000),
 ( 1.000000000000000000, 0.8660104782249490318, 1.000000000000000000),
 ( 1.000000000000000000, 0.8662041757988804269, 1.000000000000000000),
 ( 1.000000000000000000, 0.8663863992244035250, 1.000000000000000000),
 ( 1.000000000000000000, 0.8677117148204597230, 1.000000000000000000),
 ( 1.000000000000000000, 0.8700966207775098216, 1.000000000000000000),
 ( 1.000000000000000000, 0.8745420513867560031, 1.000000000000000000),
 ( 1.000000000000000000, 0.8755007923160716965, 1.000000000000000000),
 ( 1.000000000000000000, 0.8775326389012688688, 1.000000000000000000),
 ( 1.000000000000000000, 0.8786077117299072592, 1.000000000000000000),
 ( 1.000000000000000000, 0.8819935310329167777, 1.000000000000000000),
 ( 1.000000000000000000, 0.8844646895995935676, 1.000000000000000000),
 ( 1.000000000000000000, 0.8897514236679686661, 1.000000000000000000),
 ( 1.000000000000000000, 0.8925717272467494912, 1.000000000000000000),
 ( 1.000000000000000000, 0.8984586818434432409, 1.000000000000000000),
 ( 1.000000000000000000, 0.9014857458774653276, 1.000000000000000000),
 ( 1.000000000000000000, 0.9106811941533423660, 1.000000000000000000),
 ( 1.000000000000000000, 0.9169643886478042738, 1.000000000000000000),
 ( 1.000000000000000000, 0.9291626511573400915, 1.000000000000000000),
 ( 1.000000000000000000, 0.9349057736410160135, 1.000000000000000000),
 ( 1.000000000000000000, 0.9425642407771720466, 1.000000000000000000),
 ( 1.000000000000000000, 0.9449584557358955417, 1.000000000000000000),
 ( 1.000000000000000000, 0.9493596902480637700, 1.000000000000000000),
 ( 1.000000000000000000, 0.9513682277052729619, 1.000000000000000000),
 ( 1.000000000000000000, 0.9566191346130005213, 1.000000000000000000),
 ( 1.000000000000000000, 0.9591281150650757814, 1.000000000000000000),
 ( 1.000000000000000000, 0.9612060428348171426, 1.000000000000000000),
 ( 1.000000000000000000, 0.9616180368580454774, 1.000000000000000000),
 ( 1.000000000000000000, 0.9617930603854571991, 1.000000000000000000),
 ( 1.000000000000000000, 0.9617771003161980081, 1.000000000000000000),
 ( 1.000000000000000000, 0.9615975401732786976, 1.000000000000000000),
 ( 1.000000000000000000, 0.9614342877366656159, 1.000000000000000000),
 ( 1.000000000000000000, 0.9602599180209367979, 1.000000000000000000),
 ( 1.000000000000000000, 0.9581730223097011390, 1.000000000000000000),
 ( 1.000000000000000000, 0.9535175983937561606, 1.000000000000000000),
 ( 1.000000000000000000, 0.9517118983112912156, 1.000000000000000000),
 ( 1.000000000000000000, 0.9476286036465969564, 1.000000000000000000),
 ( 1.000000000000000000, 0.9453763728113453446, 1.000000000000000000),
 ( 1.000000000000000000, 0.9381189311205525572, 1.000000000000000000),
 ( 1.000000000000000000, 0.9326041533762798874, 1.000000000000000000),
 ( 1.000000000000000000, 0.9252136989611822182, 1.000000000000000000),
 ( 1.000000000000000000, 0.9237107470788312735, 1.000000000000000000),
 ( 1.000000000000000000, 0.9206640173840989760, 1.000000000000000000),
 ( 1.000000000000000000, 0.9191158710780323871, 1.000000000000000000),
 ( 1.000000000000000000, 0.9144587407289394010, 1.000000000000000000),
 ( 1.000000000000000000, 0.9113459265957564170, 1.000000000000000000),
 ( 1.000000000000000000, 0.9021094256030967040, 1.000000000000000000),
 ( 1.000000000000000000, 0.8960840667680185501, 1.000000000000000000),
 ( 1.000000000000000000, 0.8891528055769346572, 1.000000000000000000),
 ( 1.000000000000000000, 0.8877968478283493337, 1.000000000000000000),
 ( 1.000000000000000000, 0.8851579642536796522, 1.000000000000000000),
 ( 1.000000000000000000, 0.8838757127171860128, 1.000000000000000000),
 ( 1.000000000000000000, 0.8802090789781089608, 1.000000000000000000),
 ( 1.000000000000000000, 0.8779855326665648718, 1.000000000000000000),
 ( 1.000000000000000000, 0.8720740473562953454, 1.000000000000000000),
 ( 1.000000000000000000, 0.8691432809519210601, 1.000000000000000000),
 ( 1.000000000000000000, 0.8675023601337629175, 1.000000000000000000) ) ) 
 REPRESENTATION_ITEM ( '' )  SURFACE ( )  );
#7310 = EDGE_LOOP ( 'NONE', ( #30547, #8233, #22839, #4533 ) ) ;
#7311 = DIRECTION ( 'NONE',  ( 1.000000000000000000, 0.000000000000000000, 0.000000000000000000 ) ) ;
#7312 = AXIS2_PLACEMENT_3D ( 'NONE', #24190, #26235, #12364 ) ;
#7313 = VERTEX_POINT ( 'NONE', #9828 ) ;
#7314 = EDGE_CURVE ( 'NONE', #30491, #1882, #27179, .T. ) ;
#7315 = VECTOR ( 'NONE', #18820, 1000.000000000000000 ) ;
#7316 = ORIENTED_EDGE ( 'NONE', *, *, #2026, .F. ) ;
#7317 = AXIS2_PLACEMENT_3D ( 'NONE', #19749, #9941, #21938 ) ;
#7318 = ADVANCED_FACE ( 'NONE', ( #5298 ), #5143, .F. ) ;
#7319 = ADVANCED_FACE ( 'NONE', ( #19635 ), #14654, .F. ) ;
#7320 = CIRCLE ( 'NONE', #13779, 0.7500000000000006661 ) ;
#7321 = DIRECTION ( 'NONE',  ( -1.000000000000000000, 0.000000000000000000, 0.000000000000000000 ) ) ;
#7322 = CARTESIAN_POINT ( 'NONE',  ( -12.85282321250444681, 11.16584596974482935, 19.96783386855779341 ) ) ;
#7323 = CIRCLE ( 'NONE', #840, 0.7500000000000006661 ) ;
#7324 = EDGE_CURVE ( 'NONE', #20845, #11886, #21081, .T. ) ;
#7325 = CARTESIAN_POINT ( 'NONE',  ( 6.630478080506909677, 6.778663211761489116, 1.500000000000001332 ) ) ;
#7326 = CARTESIAN_POINT ( 'NONE',  ( 0.000000000000000000, 0.000000000000000000, 1.500000000000001332 ) ) ;
#7327 = CARTESIAN_POINT ( 'NONE',  ( 49.99999999999998579, 70.00000000000000000, 12.49999999999999112 ) ) ;
#7328 = FACE_BOUND ( 'NONE', #2554, .T. ) ;
#7329 = VERTEX_POINT ( 'NONE', #7180 ) ;
#7330 = CARTESIAN_POINT ( 'NONE',  ( -16.85109579167143323, 2.433552959544810435, 18.71435384576123440 ) ) ;
#7331 = CARTESIAN_POINT ( 'NONE',  ( -11.40980092660686829, 6.310027164379044429, 24.50000000000000000 ) ) ;
#7332 = CIRCLE ( 'NONE', #349, 3.559164065751841743 ) ;
#7333 = FACE_OUTER_BOUND ( 'NONE', #19003, .T. ) ;
#7334 = VERTEX_POINT ( 'NONE', #26200 ) ;
#7335 = ORIENTED_EDGE ( 'NONE', *, *, #19531, .F. ) ;
#7336 = CARTESIAN_POINT ( 'NONE',  ( 0.000000000000000000, 0.000000000000000000, 1.500000000000000000 ) ) ;
#7337 = PLANE ( 'NONE',  #17111 ) ;
#7338 = PLANE ( 'NONE',  #24308 ) ;
#7339 = CARTESIAN_POINT ( 'NONE',  ( 18.53505294460180508, -7.514422089582846631, 18.47531940416306995 ) ) ;
#7340 = DIRECTION ( 'NONE',  ( 0.000000000000000000, 0.000000000000000000, 1.000000000000000000 ) ) ;
#7341 = CIRCLE ( 'NONE', #2860, 0.7500000000000006661 ) ;
#7342 = CARTESIAN_POINT ( 'NONE',  ( -36.00052790658070023, 0.5797355074648735673, 27.50000000000000711 ) ) ;
#7343 = CIRCLE ( 'NONE', #24760, 7.500000000000000000 ) ;
#7344 = CARTESIAN_POINT ( 'NONE',  ( -19.18576292979354392, -22.55620591602727742, 24.50000000000000000 ) ) ;
#7345 = EDGE_LOOP ( 'NONE', ( #8673, #18697, #10268, #3041 ) ) ;
#7346 = CIRCLE ( 'NONE', #11341, 3.000000000000002665 ) ;
#7347 = DIRECTION ( 'NONE',  ( 0.000000000000000000, 0.000000000000000000, -1.000000000000000000 ) ) ;
#7348 = CARTESIAN_POINT ( 'NONE',  ( -17.64259547893122360, -9.420269215336071866, 18.84486140012300126 ) ) ;
#7349 = DIRECTION ( 'NONE',  ( 0.000000000000000000, 0.000000000000000000, 1.000000000000000000 ) ) ;
#7350 = ORIENTED_EDGE ( 'NONE', *, *, #30029, .F. ) ;
#7351 = CARTESIAN_POINT ( 'NONE',  ( 15.41319392345653938, 12.77323265862689183, 6.018569869498933578 ) ) ;
#7352 = ORIENTED_EDGE ( 'NONE', *, *, #2529, .T. ) ;
#7353 = VECTOR ( 'NONE', #25663, 1000.000000000000000 ) ;
#7354 = ADVANCED_FACE ( 'NONE', ( #4831 ), #7793, .T. ) ;
#7355 = CARTESIAN_POINT ( 'NONE',  ( 0.000000000000000000, 0.000000000000000000, -52.50000000000000000 ) ) ;
#7356 = AXIS2_PLACEMENT_3D ( 'NONE', #16372, #9351, #14026 ) ;
#7357 = EDGE_CURVE ( 'NONE', #12085, #18281, #21830, .T. ) ;
#7358 = CARTESIAN_POINT ( 'NONE',  ( 16.65321191614105345, 3.713086717969341866, 20.24143955528808902 ) ) ;
#7359 = DIRECTION ( 'NONE',  ( 1.000000000000000000, 0.000000000000000000, 0.000000000000000000 ) ) ;
#7360 = ORIENTED_EDGE ( 'NONE', *, *, #13042, .T. ) ;
#7361 = AXIS2_PLACEMENT_3D ( 'NONE', #10774, #23064, #6243 ) ;
#7362 = CARTESIAN_POINT ( 'NONE',  ( 3.898220458062934046, 16.59828442330441689, 5.661398277488802755 ) ) ;
#7363 = CARTESIAN_POINT ( 'NONE',  ( -8.072557715923444732, 14.41080185948837311, 24.50000000000000000 ) ) ;
#7364 = DIRECTION ( 'NONE',  ( -0.000000000000000000, 1.132880637372608986E-16, -1.000000000000000000 ) ) ;
#7365 = CIRCLE ( 'NONE', #28776, 9.084132297865673777 ) ;
#7366 = LINE ( 'NONE', #16407, #11347 ) ;
#7367 = CARTESIAN_POINT ( 'NONE',  ( 34.99999999999933920, 4.286263797015655244E-15, 85.49999999999998579 ) ) ;
#7368 = ORIENTED_EDGE ( 'NONE', *, *, #29806, .F. ) ;
#7369 = CARTESIAN_POINT ( 'NONE',  ( -10.11202017158235833, -41.14070756921188377, -1.500000000000000000 ) ) ;
#7370 = DIRECTION ( 'NONE',  ( 0.000000000000000000, 1.000000000000000000, 0.000000000000000000 ) ) ;
#7371 = ORIENTED_EDGE ( 'NONE', *, *, #23631, .F. ) ;
#7372 = CARTESIAN_POINT ( 'NONE',  ( 9.999999999999959144, 1.510243460696181139E-14, 24.50000000000000000 ) ) ;
#7373 = CARTESIAN_POINT ( 'NONE',  ( -14.70315170625142365, -8.688231105434649493, 19.36813350477385143 ) ) ;
#7374 = VECTOR ( 'NONE', #27537, 1000.000000000000000 ) ;
#7375 = CARTESIAN_POINT ( 'NONE',  ( -33.78553900464347493, 24.40792682089791654, -16.50000000000000000 ) ) ;
#7376 = DIRECTION ( 'NONE',  ( -0.000000000000000000, 0.000000000000000000, 1.000000000000000000 ) ) ;
#7377 = CIRCLE ( 'NONE', #24804, 2.898871837527151385 ) ;
#7378 = CARTESIAN_POINT ( 'NONE',  ( -31.18700685316050780, 26.11823559932051353, -1.500000000000000000 ) ) ;
#7379 = VECTOR ( 'NONE', #13092, 1000.000000000000114 ) ;
#7380 = EDGE_LOOP ( 'NONE', ( #24925, #16760 ) ) ;
#7381 = CARTESIAN_POINT ( 'NONE',  ( -1.000000000000008438, 13.00000000000001421, 1.500000000000001332 ) ) ;
#7382 = CARTESIAN_POINT ( 'NONE',  ( 30.84961167908536339, 26.01027997894835764, 30.46573359564818162 ) ) ;
#7383 = CARTESIAN_POINT ( 'NONE',  ( -6.742350454026557749, 18.82948505227174962, 6.037995405461185072 ) ) ;
#7384 = EDGE_LOOP ( 'NONE', ( #19751, #23047, #3480, #3741 ) ) ;
#7385 = DIRECTION ( 'NONE',  ( 0.000000000000000000, 1.000000000000000000, 0.000000000000000000 ) ) ;
#7386 = ORIENTED_EDGE ( 'NONE', *, *, #10728, .F. ) ;
#7387 = CARTESIAN_POINT ( 'NONE',  ( 30.53339558441486190, -7.800891647352842462, 39.24389099736750097 ) ) ;
#7388 = CARTESIAN_POINT ( 'NONE',  ( 26.83043119477639138, -8.695877139419035728, 1.500000000000000000 ) ) ;
#7389 = CIRCLE ( 'NONE', #18832, 0.7500000000000006661 ) ;
#7390 = ORIENTED_EDGE ( 'NONE', *, *, #19318, .T. ) ;
#7391 = VERTEX_POINT ( 'NONE', #15733 ) ;
#7392 = CARTESIAN_POINT ( 'NONE',  ( 50.00000000000000000, 6.123233995736766085E-15, -87.50000000000000000 ) ) ;
#7393 = ORIENTED_EDGE ( 'NONE', *, *, #26959, .T. ) ;
#7394 = ORIENTED_EDGE ( 'NONE', *, *, #23095, .F. ) ;
#7395 = CARTESIAN_POINT ( 'NONE',  ( -0.6129396130214324057, -20.00853051056088461, 19.66989035740801839 ) ) ;
#7396 = AXIS2_PLACEMENT_3D ( 'NONE', #9486, #28514, #21014 ) ;
#7397 = CARTESIAN_POINT ( 'NONE',  ( -8.089106849613333594, -15.02215080929124547, 7.500147780736496017 ) ) ;
#7398 = CARTESIAN_POINT ( 'NONE',  ( 0.000000000000000000, 1.699320956058915452E-16, -1.500000000000001776 ) ) ;
#7399 = CARTESIAN_POINT ( 'NONE',  ( 1.009606305713754315, -17.02204649693582184, 18.37415474056476938 ) ) ;
#7400 = AXIS2_PLACEMENT_3D ( 'NONE', #23962, #2609, #263 ) ;
#7401 = ORIENTED_EDGE ( 'NONE', *, *, #13724, .T. ) ;
#7402 = CARTESIAN_POINT ( 'NONE',  ( -14.58213539500865785, 7.758783772730382111, 1.500000000000000000 ) ) ;
#7403 = CARTESIAN_POINT ( 'NONE',  ( -23.16720440049831709, -10.90834004837188154, 45.15082199682045427 ) ) ;
#7404 = CARTESIAN_POINT ( 'NONE',  ( 14.89413573707702021, 13.37445272932973417, 18.34798005862662507 ) ) ;
#7405 = DIRECTION ( 'NONE',  ( -1.000000000000000000, 0.000000000000000000, 0.000000000000000000 ) ) ;
#7406 = ORIENTED_EDGE ( 'NONE', *, *, #11303, .F. ) ;
#7407 = B_SPLINE_CURVE_WITH_KNOTS ( 'NONE', 3,
 ( #20924, #8500, #9089, #20481, #16109, #13321, #20332, #10982, #15489, #20772, #30001, #6284, #15797, #27364, #4102, #1620, #25317, #25629, #18302, #6451 ),
 .UNSPECIFIED., .F., .F.,
 ( 4, 2, 2, 2, 2, 2, 2, 2, 2, 4 ),
 ( 0.000000000000000000, 0.06250000000000054123, 0.1250000000000009714, 0.1875000000000014155, 0.2187500000000014433, 0.2500000000000014433, 0.3125000000000011102, 0.3750000000000007216, 0.4375000000000003886, 0.5000000000000000000 ),
 .UNSPECIFIED. ) ;
#7408 = CARTESIAN_POINT ( 'NONE',  ( -2.209227181723746103, 8.499586724479465616, -3.621320343559650379 ) ) ;
#7409 = CARTESIAN_POINT ( 'NONE',  ( -14.70423443302406419, -8.686234331489293581, 6.782048567692550378 ) ) ;
#7410 = CARTESIAN_POINT ( 'NONE',  ( -5.974095823819629558, 15.97878383974769534, 5.749491821935610147 ) ) ;
#7411 = DIRECTION ( 'NONE',  ( 0.000000000000000000, 0.000000000000000000, 1.000000000000000000 ) ) ;
#7412 = CARTESIAN_POINT ( 'NONE',  ( 28.79137815760242702, -9.331429872129930914, 1.500000000000000000 ) ) ;
#7413 = DIRECTION ( 'NONE',  ( 0.000000000000000000, 1.000000000000000000, 0.000000000000000000 ) ) ;
#7414 = FACE_OUTER_BOUND ( 'NONE', #5171, .T. ) ;
#7415 = ORIENTED_EDGE ( 'NONE', *, *, #30363, .T. ) ;
#7416 = ORIENTED_EDGE ( 'NONE', *, *, #17785, .T. ) ;
#7417 = CARTESIAN_POINT ( 'NONE',  ( 40.89187623478217404, 5.790488632116406187, -19.50000000000000355 ) ) ;
#7418 = ORIENTED_EDGE ( 'NONE', *, *, #9001, .F. ) ;
#7419 = DIRECTION ( 'NONE',  ( 0.000000000000000000, 1.000000000000000000, 0.000000000000000000 ) ) ;
#7420 = CARTESIAN_POINT ( 'NONE',  ( 11.11118388262826784, -16.62953976291649028, 18.34798005863226678 ) ) ;
#7421 = ORIENTED_EDGE ( 'NONE', *, *, #27687, .F. ) ;
#7422 = APPLICATION_PROTOCOL_DEFINITION ( 'draft international standard', 'automotive_design', 1998, #26509 ) ;
#7423 = CARTESIAN_POINT ( 'NONE',  ( 15.81416692036122207, -6.360574302898111654, 18.34798005863078885 ) ) ;
#7424 = AXIS2_PLACEMENT_3D ( 'NONE', #12978, #22469, #12092 ) ;
#7425 = VECTOR ( 'NONE', #23088, 1000.000000000000000 ) ;
#7426 = DIRECTION ( 'NONE',  ( 0.000000000000000000, 0.000000000000000000, -1.000000000000000000 ) ) ;
#7427 = ORIENTED_EDGE ( 'NONE', *, *, #7891, .T. ) ;
#7428 = CARTESIAN_POINT ( 'NONE',  ( 5.627515464934154998, 19.21053377385552707, 20.29090034784956131 ) ) ;
#7429 = DIRECTION ( 'NONE',  ( -1.000000000000000000, 0.000000000000000000, 0.000000000000000000 ) ) ;
#7430 = AXIS2_PLACEMENT_3D ( 'NONE', #12288, #22093, #5110 ) ;
#7431 = DIRECTION ( 'NONE',  ( -1.000000000000000000, 0.000000000000000000, 0.000000000000000000 ) ) ;
#7432 = CARTESIAN_POINT ( 'NONE',  ( -32.89458440824127194, 18.04996087680839167, 37.50000000007908341 ) ) ;
#7433 = ORIENTED_EDGE ( 'NONE', *, *, #7231, .F. ) ;
#7434 = CARTESIAN_POINT ( 'NONE',  ( 9.056472324687607767, 0.7083562926195451359, -1.500000000000001776 ) ) ;
#7435 = EDGE_CURVE ( 'NONE', #3590, #6841, #4158, .T. ) ;
#7436 = ADVANCED_FACE ( 'NONE', ( #29481 ), #20104, .F. ) ;
#7437 = CARTESIAN_POINT ( 'NONE',  ( 25.10445388623454477, 25.60065097860747585, 1.500000000000000000 ) ) ;
#7438 = AXIS2_PLACEMENT_3D ( 'NONE', #6914, #13932, #11449 ) ;
#7439 = CARTESIAN_POINT ( 'NONE',  ( 1.038391619697657475, 44.07656847656198806, -16.49999999999999645 ) ) ;
#7440 = VERTEX_POINT ( 'NONE', #25251 ) ;
#7441 = CARTESIAN_POINT ( 'NONE',  ( -15.54251014615009296, -6.943938207015639463, 7.080843742048788414 ) ) ;
#7442 = CARTESIAN_POINT ( 'NONE',  ( -50.00000000000000000, -70.00000000000000000, -92.50000000000000000 ) ) ;
#7443 = PRODUCT_DEFINITION_SHAPE ( 'NONE', 'NONE',  #30868 ) ;
#7444 = CARTESIAN_POINT ( 'NONE',  ( 0.1277494853664074559, -20.01772078232906793, 5.670038381137163519 ) ) ;
#7445 = CARTESIAN_POINT ( 'NONE',  ( 6.812559277181973627, -5.881244434206257310, 1.500000000000001332 ) ) ;
#7446 = EDGE_CURVE ( 'NONE', #17807, #21378, #3899, .T. ) ;
#7447 = DIRECTION ( 'NONE',  ( -1.000000000000000000, 0.000000000000000000, 0.000000000000000000 ) ) ;
#7448 = CARTESIAN_POINT ( 'NONE',  ( 37.79101548699587454, -10.50083399009356988, 14.39349168688145575 ) ) ;
#7449 = FACE_OUTER_BOUND ( 'NONE', #18607, .T. ) ;
#7450 = ORIENTED_EDGE ( 'NONE', *, *, #27898, .F. ) ;
#7451 = CARTESIAN_POINT ( 'NONE',  ( 12.37236664230077743, -12.04390635323149716, 1.500000000000000000 ) ) ;
#7452 = B_SPLINE_CURVE_WITH_KNOTS ( 'NONE', 3,
 ( #16489, #26006, #1989, #12229, #19405, #6978, #4486, #28923, #4634, #14134, #30380, #11513, #20996, #17056, #2870, #25546, #12394, #4169, #13699, #24071, #13995, #23493, #2135, #14714, #11652, #21143, #21728 ),
 .UNSPECIFIED., .F., .F.,
 ( 4, 2, 1, 1, 2, 2, 2, 2, 1, 1, 1, 2, 2, 2, 2, 4 ),
 ( 0.9060794618157798075, 0.9075469702249081561, 0.9090144786340366156, 0.9119494954522934238, 0.9178195290888072622, 0.9295595963618348279, 0.9530397309078899593, 0.9545072393170184188, 0.9559747477261468784, 0.9589097645444037976, 0.9647797981809175250, 0.9677148149991744441, 0.9706498318174312523, 0.9765198654539450906, 0.9882599327269725453, 1.000000000000000000 ),
 .UNSPECIFIED. ) ;
#7453 = VECTOR ( 'NONE', #11108, 1000.000000000000000 ) ;
#7454 = CARTESIAN_POINT ( 'NONE',  ( -50.00000000000000000, -50.00000000000000000, 62.49999999999999289 ) ) ;
#7455 = VERTEX_POINT ( 'NONE', #5763 ) ;
#7456 = VERTEX_POINT ( 'NONE', #27604 ) ;
#7457 = DIRECTION ( 'NONE',  ( -0.6707505147970090897, -0.7416830501633074890, 0.000000000000000000 ) ) ;
#7458 = CYLINDRICAL_SURFACE ( 'NONE', #15895, 0.7500000000000003331 ) ;
#7459 = ORIENTED_EDGE ( 'NONE', *, *, #24027, .T. ) ;
#7460 = AXIS2_PLACEMENT_3D ( 'NONE', #6272, #15784, #25306 ) ;
#7461 = EDGE_CURVE ( 'NONE', #7103, #6285, #24628, .T. ) ;
#7462 = DIRECTION ( 'NONE',  ( 0.000000000000000000, 0.000000000000000000, 1.000000000000000000 ) ) ;
#7463 = ADVANCED_FACE ( 'NONE', ( #15113, #13259 ), #10920, .F. ) ;
#7464 = CARTESIAN_POINT ( 'NONE',  ( -65.00000000000000000, -36.86186943028246787, 57.49999999999999289 ) ) ;
#7465 = VERTEX_POINT ( 'NONE', #13424 ) ;
#7466 = EDGE_CURVE ( 'NONE', #14242, #18086, #12631, .T. ) ;
#7467 = CARTESIAN_POINT ( 'NONE',  ( 18.38343463818524981, -7.922482876633608839, 18.34838970509067479 ) ) ;
#7468 = CARTESIAN_POINT ( 'NONE',  ( 19.76051936388921604, 3.198927888044590162, 18.34798005862662507 ) ) ;
#7469 = DIRECTION ( 'NONE',  ( -1.000000000000000000, 0.000000000000000000, 0.000000000000000000 ) ) ;
#7470 = VERTEX_POINT ( 'NONE', #29944 ) ;
#7471 = FACE_OUTER_BOUND ( 'NONE', #3799, .T. ) ;
#7472 = ORIENTED_EDGE ( 'NONE', *, *, #22914, .T. ) ;
#7473 = EDGE_CURVE ( 'NONE', #11838, #17742, #16598, .T. ) ;
#7474 = CIRCLE ( 'NONE', #26395, 20.00000000000000000 ) ;
#7475 = ORIENTED_EDGE ( 'NONE', *, *, #24487, .F. ) ;
#7476 = ADVANCED_FACE ( 'NONE', ( #22444 ), #8581, .F. ) ;
#7477 = CARTESIAN_POINT ( 'NONE',  ( 38.96677131950519879, -1.867903411460851926, 32.22156839220826896 ) ) ;
#7478 = CARTESIAN_POINT ( 'NONE',  ( -12.72741959552008595, 11.30275801665550794, 19.56050940960062690 ) ) ;
#7479 = AXIS2_PLACEMENT_3D ( 'NONE', #10559, #29736, #11176 ) ;
#7480 = EDGE_CURVE ( 'NONE', #9580, #12801, #932, .T. ) ;
#7481 = CARTESIAN_POINT ( 'NONE',  ( -7.747355498299749677, -15.21644541356979907, 18.92976555901915603 ) ) ;
#7482 = EDGE_CURVE ( 'NONE', #23974, #14320, #10448, .T. ) ;
#7483 = LINE ( 'NONE', #2019, #23981 ) ;
#7484 = CARTESIAN_POINT ( 'NONE',  ( 8.999114229549594057, -0.1262659238204522361, 21.50000000000000000 ) ) ;
#7485 = CARTESIAN_POINT ( 'NONE',  ( 4.045242219987651211, 16.55840560649980731, 18.34798005863078885 ) ) ;
#7486 = VERTEX_POINT ( 'NONE', #5923 ) ;
#7487 = CARTESIAN_POINT ( 'NONE',  ( 9.676137610658594568, -14.02562811695957024, 5.670038381137163519 ) ) ;
#7488 = DIRECTION ( 'NONE',  ( -1.000000000000000000, 0.000000000000000000, 0.000000000000000000 ) ) ;
#7489 = CARTESIAN_POINT ( 'NONE',  ( 1.438332125858173605, -8.884323311075778662, 1.500000000000001332 ) ) ;
#7490 = ORIENTED_EDGE ( 'NONE', *, *, #18921, .T. ) ;
#7491 = ORIENTED_EDGE ( 'NONE', *, *, #28842, .F. ) ;
#7492 = DIRECTION ( 'NONE',  ( -1.000000000000000000, 0.000000000000000000, 0.000000000000000000 ) ) ;
#7493 = DIRECTION ( 'NONE',  ( 0.000000000000000000, 0.000000000000000000, -1.000000000000000000 ) ) ;
#7494 = CARTESIAN_POINT ( 'NONE',  ( -5.325396069054047388, 16.18574704710537659, 7.632642797338977658 ) ) ;
#7495 = CARTESIAN_POINT ( 'NONE',  ( -15.37836256574693827, -7.321964740028795049, 7.526951045817044772 ) ) ;
#7496 = CIRCLE ( 'NONE', #5489, 0.9999999999999983347 ) ;
#7497 = EDGE_CURVE ( 'NONE', #22829, #23519, #14578, .T. ) ;
#7498 = CARTESIAN_POINT ( 'NONE',  ( -3.395021109945006721, -30.50000000000000711, 1.500000000000001332 ) ) ;
#7499 = ORIENTED_EDGE ( 'NONE', *, *, #27687, .T. ) ;
#7500 = EDGE_CURVE ( 'NONE', #16268, #11562, #27035, .T. ) ;
#7501 = VERTEX_POINT ( 'NONE', #12951 ) ;
#7502 = CARTESIAN_POINT ( 'NONE',  ( -23.21352257770656990, 10.78826658734919519, 49.40206402021039622 ) ) ;
#7503 = CARTESIAN_POINT ( 'NONE',  ( -4.163336342344337027E-14, 1.387778780781445676E-14, 24.50000000000000000 ) ) ;
#7504 = ADVANCED_FACE ( 'NONE', ( #13105 ), #1088, .F. ) ;
#7505 = CARTESIAN_POINT ( 'NONE',  ( 25.10445388623454477, -25.60065097860747585, -1.500000000000000000 ) ) ;
#7506 = ORIENTED_EDGE ( 'NONE', *, *, #27881, .F. ) ;
#7507 = CARTESIAN_POINT ( 'NONE',  ( 15.12016594919360557, 13.11846484362264320, 7.595116371587256054 ) ) ;
#7508 = ORIENTED_EDGE ( 'NONE', *, *, #6167, .T. ) ;
#7509 = CARTESIAN_POINT ( 'NONE',  ( 18.38084888341871093, -7.928499866610141389, 7.652108011868850035 ) ) ;
#7510 = EDGE_CURVE ( 'NONE', #20399, #4649, #22597, .T. ) ;
#7511 = CARTESIAN_POINT ( 'NONE',  ( 20.47140833542507821, 26.57182937991349903, -6.500000000000000888 ) ) ;
#7512 = DIRECTION ( 'NONE',  ( -1.000000000000000000, 0.000000000000000000, 0.000000000000000000 ) ) ;
#7513 = ORIENTED_EDGE ( 'NONE', *, *, #13608, .F. ) ;
#7514 = EDGE_CURVE ( 'NONE', #10711, #7128, #24521, .T. ) ;
#7515 = CARTESIAN_POINT ( 'NONE',  ( -70.00000000000000000, -70.00000000000000000, -92.50000000000000000 ) ) ;
#7516 = CYLINDRICAL_SURFACE ( 'NONE', #25610, 11.99999999999998934 ) ;
#7517 = DIRECTION ( 'NONE',  ( 0.000000000000000000, 0.7709617516270895754, 0.6368814469962912339 ) ) ;
#7518 = DIRECTION ( 'NONE',  ( 0.000000000000000000, 0.000000000000000000, 1.000000000000000000 ) ) ;
#7519 = AXIS2_PLACEMENT_3D ( 'NONE', #4161, #20396, #27885 ) ;
#7520 = PLANE ( 'NONE',  #3940 ) ;
#7521 = PLANE ( 'NONE',  #15807 ) ;
#7522 = CARTESIAN_POINT ( 'NONE',  ( 33.42925964089140933, 11.06161099612213405, 39.78814634291935448 ) ) ;
#7523 = ORIENTED_EDGE ( 'NONE', *, *, #376, .F. ) ;
#7524 = CARTESIAN_POINT ( 'NONE',  ( 15.40017468080368168, -7.251222802968046999, 6.910395520694542881 ) ) ;
#7525 = LINE ( 'NONE', #5174, #17247 ) ;
#7526 = CARTESIAN_POINT ( 'NONE',  ( -5.374868878254082105, 44.10336124695542992, -19.50000000000000355 ) ) ;
#7527 = FACE_OUTER_BOUND ( 'NONE', #28761, .T. ) ;
#7528 = ORIENTED_EDGE ( 'NONE', *, *, #14712, .F. ) ;
#7529 = DIRECTION ( 'NONE',  ( 0.9898214418809326842, 0.1423148382732852268, -0.000000000000000000 ) ) ;
#7530 = DIRECTION ( 'NONE',  ( -0.000000000000000000, 1.132880637372608986E-16, -1.000000000000000000 ) ) ;
#7531 = EDGE_CURVE ( 'NONE', #24159, #2072, #27100, .T. ) ;
#7532 = DIRECTION ( 'NONE',  ( -1.000000000000000000, 0.000000000000000000, -0.000000000000000000 ) ) ;
#7533 = EDGE_CURVE ( 'NONE', #28104, #2857, #4756, .T. ) ;
#7534 = CARTESIAN_POINT ( 'NONE',  ( 2.552544030762014415, -42.50000000000000000, -1.500000000000000000 ) ) ;
#7535 = CARTESIAN_POINT ( 'NONE',  ( -4.163336342344337027E-14, -1.387778780781445676E-14, 1.500000000000000000 ) ) ;
#7536 = CARTESIAN_POINT ( 'NONE',  ( 37.50184436008131428, 0.5407290483799589431, 37.50000000002315659 ) ) ;
#7537 = DIRECTION ( 'NONE',  ( 0.000000000000000000, -1.000000000000000000, 0.000000000000000000 ) ) ;
#7538 = VERTEX_POINT ( 'NONE', #12102 ) ;
#7539 = VECTOR ( 'NONE', #13091, 1000.000000000000000 ) ;
#7540 = DIRECTION ( 'NONE',  ( 1.000000000000000000, 0.000000000000000000, -0.000000000000000000 ) ) ;
#7541 = EDGE_LOOP ( 'NONE', ( #2850, #30169, #15330, #2182 ) ) ;
#7542 = DIRECTION ( 'NONE',  ( -0.000000000000000000, -0.000000000000000000, 1.000000000000000000 ) ) ;
#7543 = DIRECTION ( 'NONE',  ( 1.000000000000000000, 0.000000000000000000, 0.000000000000000000 ) ) ;
#7544 = EDGE_LOOP ( 'NONE', ( #23228, #1360, #23628, #15707 ) ) ;
#7545 = ORIENTED_EDGE ( 'NONE', *, *, #20976, .T. ) ;
#7546 = FACE_BOUND ( 'NONE', #11922, .T. ) ;
#7547 = ORIENTED_EDGE ( 'NONE', *, *, #4231, .F. ) ;
#7548 = ORIENTED_EDGE ( 'NONE', *, *, #12678, .T. ) ;
#7549 = DIRECTION ( 'NONE',  ( -0.5406408174555974444, -0.8412535328311813165, -0.000000000000000000 ) ) ;
#7550 = CARTESIAN_POINT ( 'NONE',  ( -23.21352257770656990, 10.78826658734919519, 49.40206402021039622 ) ) ;
#7551 = CARTESIAN_POINT ( 'NONE',  ( -70.00000000000000000, -50.00000000000000000, -92.50000000000000000 ) ) ;
#7552 = DIRECTION ( 'NONE',  ( 1.000000000000000000, 0.000000000000000000, 0.000000000000000000 ) ) ;
#7553 = CARTESIAN_POINT ( 'NONE',  ( 1.411528516173252923, -17.00651183856732018, 20.13759033520874908 ) ) ;
#7554 = VERTEX_POINT ( 'NONE', #15905 ) ;
#7555 = CARTESIAN_POINT ( 'NONE',  ( 26.11179934312166395, 14.04991663536889490, 45.34931131770220247 ) ) ;
#7556 = DIRECTION ( 'NONE',  ( -0.000000000000000000, -0.000000000000000000, 1.000000000000000000 ) ) ;
#7557 = CARTESIAN_POINT ( 'NONE',  ( 14.84329864647545349, 13.43104200419766592, 18.34838970509067479 ) ) ;
#7558 = CARTESIAN_POINT ( 'NONE',  ( -1.897971151300065476E-14, 90.00000000000001421, 22.49999999999999289 ) ) ;
#7559 = EDGE_LOOP ( 'NONE', ( #26576, #13695, #24618, #2013 ) ) ;
#7560 = CIRCLE ( 'NONE', #10050, 2.898871837527149609 ) ;
#7561 = DIRECTION ( 'NONE',  ( 0.000000000000000000, 0.000000000000000000, 1.000000000000000000 ) ) ;
#7562 = CARTESIAN_POINT ( 'NONE',  ( -14.71031647956046839, -8.675071222119054681, 6.447548852708279377 ) ) ;
#7563 = CARTESIAN_POINT ( 'NONE',  ( -6.936828876846345082, 18.77725343618824994, 6.672349528511551497 ) ) ;
#7564 = DIRECTION ( 'NONE',  ( 0.000000000000000000, -0.000000000000000000, 1.000000000000000000 ) ) ;
#7565 = CARTESIAN_POINT ( 'NONE',  ( 0.01885174614965954773, 0.8831628876357842106, 9.000000000000003553 ) ) ;
#7566 = CARTESIAN_POINT ( 'NONE',  ( 25.47847050916410439, -26.57182937991349903, -6.499999999999999112 ) ) ;
#7567 = DIRECTION ( 'NONE',  ( -0.000000000000000000, -0.000000000000000000, -1.000000000000000000 ) ) ;
#7568 = EDGE_CURVE ( 'NONE', #24166, #1662, #30079, .T. ) ;
#7569 = ORIENTED_EDGE ( 'NONE', *, *, #18561, .T. ) ;
#7570 = EDGE_LOOP ( 'NONE', ( #21258, #11374, #24118, #10423 ) ) ;
#7571 = CARTESIAN_POINT ( 'NONE',  ( -4.390207617113899730, 7.856594496258241023, 1.500000000000001332 ) ) ;
#7572 = ADVANCED_FACE ( 'NONE', ( #6957 ), #19260, .F. ) ;
#7573 = DIRECTION ( 'NONE',  ( -1.000000000000000000, 0.000000000000000000, 0.000000000000000000 ) ) ;
#7574 = CARTESIAN_POINT ( 'NONE',  ( -12.85282321250444681, 11.16584596974482757, 7.272049892295485485 ) ) ;
#7576 = CARTESIAN_POINT ( 'NONE',  ( 0.2758680007048933680, -17.03033689273112827, 5.774779864094944593 ) ) ;
#7575 = AXIS2_PLACEMENT_3D ( 'NONE', #16796, #4946, #13853 ) ;
#7577 = ORIENTED_EDGE ( 'NONE', *, *, #1377, .F. ) ;
#7578 = PRODUCT_CONTEXT ( 'NONE', #3601, 'mechanical' ) ;
#7579 = DIRECTION ( 'NONE',  ( 1.000000000000000000, 0.000000000000000000, 0.000000000000000000 ) ) ;
#7580 = PLANE ( 'NONE',  #15680 ) ;
#7581 = VERTEX_POINT ( 'NONE', #28481 ) ;
#7582 = CARTESIAN_POINT ( 'NONE',  ( 34.70577939417254498, 10.49309206032065944, 34.49999999999999289 ) ) ;
#7583 = CIRCLE ( 'NONE', #27514, 0.7500000000000006661 ) ;
#7584 = DIRECTION ( 'NONE',  ( 0.000000000000000000, 0.000000000000000000, -1.000000000000000000 ) ) ;
#7585 = B_SPLINE_CURVE_WITH_KNOTS ( 'NONE', 3,
 ( #22927, #24810, #24964, #13588, #20133, #27620 ),
 .UNSPECIFIED., .F., .F.,
 ( 4, 2, 4 ),
 ( 1.408367944312347353, 1.570796326794896558, 1.733224709277445319 ),
 .UNSPECIFIED. ) ;
#7586 = CARTESIAN_POINT ( 'NONE',  ( -37.98447197189175739, -9.661085588429401128, 34.97777146685444905 ) ) ;
#7587 = ORIENTED_EDGE ( 'NONE', *, *, #6905, .T. ) ;
#7588 = CARTESIAN_POINT ( 'NONE',  ( 24.03448224033878944, 8.660042335149841009, 45.23564988763769179 ) ) ;
#7589 = DIRECTION ( 'NONE',  ( 0.000000000000000000, 1.132880637372608986E-16, -1.000000000000000000 ) ) ;
#7590 = CARTESIAN_POINT ( 'NONE',  ( 4.770489558936219510E-15, -42.50000000000000000, -1.500000000000000000 ) ) ;
#7591 = VERTEX_POINT ( 'NONE', #23048 ) ;
#7592 = CARTESIAN_POINT ( 'NONE',  ( 6.899999999999999467, 9.000000000000000000, 0.000000000000000000 ) ) ;
#7593 = CARTESIAN_POINT ( 'NONE',  ( 16.69721919944051791, -13.88429941593332551, 1.500000000000000000 ) ) ;
#7594 = CARTESIAN_POINT ( 'NONE',  ( -0.2093543646724261298, -17.02041581256300873, 6.420335371522007506 ) ) ;
#7595 = CARTESIAN_POINT ( 'NONE',  ( 9.056208293496307959, -2.810445847081891824, 1.500000000000001332 ) ) ;
#7596 = CARTESIAN_POINT ( 'NONE',  ( 22.49999999999992184, 1.663324310589599759E-14, 62.49999999999999289 ) ) ;
#7597 = CARTESIAN_POINT ( 'NONE',  ( 37.89827105978137922, -10.03094553435206926, 13.95238484874844787 ) ) ;
#7598 = CARTESIAN_POINT ( 'NONE',  ( 0.000000000000000000, 0.000000000000000000, 1.500000000000001332 ) ) ;
#7599 = ORIENTED_EDGE ( 'NONE', *, *, #13371, .F. ) ;
#7600 = FACE_BOUND ( 'NONE', #7839, .T. ) ;
#7601 = CARTESIAN_POINT ( 'NONE',  ( 4.437794406404241165, 19.50150518896415974, 7.161525567826892313 ) ) ;
#7602 = ORIENTED_EDGE ( 'NONE', *, *, #26210, .T. ) ;
#7603 = EDGE_LOOP ( 'NONE', ( #28178, #18681, #11755, #5936 ) ) ;
#7604 = B_SPLINE_CURVE_WITH_KNOTS ( 'NONE', 3,
 ( #25086, #27901, #13246, #22582, #10586, #1075, #25403, #17926, #27742, #24932, #25550, #4175, #20101, #20552, #22734, #27438, #6524, #18073, #6058, #4030 ),
 .UNSPECIFIED., .F., .F.,
 ( 4, 2, 2, 2, 2, 2, 2, 2, 2, 4 ),
 ( 0.000000000000000000, 0.06250000000000072164, 0.1250000000000014433, 0.1875000000000021649, 0.2187500000000021094, 0.2500000000000020539, 0.3125000000000015543, 0.3750000000000010547, 0.4375000000000005551, 0.5000000000000000000 ),
 .UNSPECIFIED. ) ;
#7605 = LINE ( 'NONE', #17432, #14636 ) ;
#7606 = DIRECTION ( 'NONE',  ( 0.000000000000000000, 1.000000000000000000, 0.000000000000000000 ) ) ;
#7607 = VERTEX_POINT ( 'NONE', #28332 ) ;
#7608 = CARTESIAN_POINT ( 'NONE',  ( 12.43151381881690476, 11.65737597917811996, 18.35377592296120497 ) ) ;
#7609 = AXIS2_PLACEMENT_3D ( 'NONE', #4721, #21553, #21239 ) ;
#7610 = VECTOR ( 'NONE', #10942, 1000.000000000000000 ) ;
#7611 = CARTESIAN_POINT ( 'NONE',  ( -9.002647793593395065, -14.45788447640154395, 5.796888747622817029 ) ) ;
#7612 = ORIENTED_EDGE ( 'NONE', *, *, #19112, .T. ) ;
#7613 = CIRCLE ( 'NONE', #15579, 1.000000000000007772 ) ;
#7614 = CARTESIAN_POINT ( 'NONE',  ( 15.81416324982725818, -6.360572704771151997, 18.34798005862662507 ) ) ;
#7615 = CARTESIAN_POINT ( 'NONE',  ( 19.72311808385370213, 3.421819763545495441, 18.37415474056476938 ) ) ;
#7616 = CARTESIAN_POINT ( 'NONE',  ( 40.22758167353954661, -5.871156286330812435, -16.50000000000000711 ) ) ;
#7617 = ORIENTED_EDGE ( 'NONE', *, *, #25695, .F. ) ;
#7618 = CARTESIAN_POINT ( 'NONE',  ( 15.70571165148985315, -6.606148062277499733, 20.32222155561919053 ) ) ;
#7619 = ORIENTED_EDGE ( 'NONE', *, *, #8476, .F. ) ;
#7620 = ORIENTED_EDGE ( 'NONE', *, *, #11084, .F. ) ;
#7621 = DIRECTION ( 'NONE',  ( 0.000000000000000000, -1.132880637372608986E-16, 1.000000000000000000 ) ) ;
#7622 = CARTESIAN_POINT ( 'NONE',  ( -5.974095823819627782, 15.97878383974769179, 18.44527579819791185 ) ) ;
#7623 = CARTESIAN_POINT ( 'NONE',  ( -13.30548897721377699, 10.64932510079500538, 20.34789198813115263 ) ) ;
#7624 = CIRCLE ( 'NONE', #4547, 9.482273699623480212 ) ;
#7625 = CARTESIAN_POINT ( 'NONE',  ( -9.646222981487634129, -17.54010295177085155, 19.25672174529527325 ) ) ;
#7626 = CARTESIAN_POINT ( 'NONE',  ( -33.37350925571147542, 22.02919766087737941, 30.87635845694642711 ) ) ;
#7627 = CIRCLE ( 'NONE', #18099, 9.482273699623480212 ) ;
#7628 = PLANE ( 'NONE',  #4541 ) ;
#7629 = FACE_OUTER_BOUND ( 'NONE', #24715, .T. ) ;
#7630 = ORIENTED_EDGE ( 'NONE', *, *, #26922, .T. ) ;
#7631 = PRODUCT_DEFINITION ( 'UNKNOWN', '', #17893, #3913 ) ;
#7632 = CIRCLE ( 'NONE', #3653, 7.500000000000000000 ) ;
#7633 = CARTESIAN_POINT ( 'NONE',  ( 9.135582339684649611, -14.36547911245298259, 7.176035686813569292 ) ) ;
#7634 = CARTESIAN_POINT ( 'NONE',  ( -27.98709118423092690, 29.59858197539721658, 13.20579471836786745 ) ) ;
#7635 = CARTESIAN_POINT ( 'NONE',  ( 9.439370189418465174, -14.17768557490432002, 5.774779864094943704 ) ) ;
#7636 = EDGE_CURVE ( 'NONE', #16019, #25635, #16723, .T. ) ;
#7637 = ORIENTED_EDGE ( 'NONE', *, *, #1997, .T. ) ;
#7638 = VERTEX_POINT ( 'NONE', #4918 ) ;
#7639 = CARTESIAN_POINT ( 'NONE',  ( 32.19782014694307293, 14.25394737442116444, 35.54550565580007770 ) ) ;
#7640 = CARTESIAN_POINT ( 'NONE',  ( 28.34828976096171971, -29.18752572968383419, -1.500000000000000000 ) ) ;
#7641 = ADVANCED_FACE ( 'NONE', ( #26447 ), #5077, .F. ) ;
#7642 = CARTESIAN_POINT ( 'NONE',  ( 18.67144399175157687, -7.167977615171057693, 19.85730954408919757 ) ) ;
#7643 = DIRECTION ( 'NONE',  ( 1.000000000000000000, 0.000000000000000000, -0.000000000000000000 ) ) ;
#7644 = DIRECTION ( 'NONE',  ( -1.000000000000000000, 0.000000000000000000, 0.000000000000000000 ) ) ;
#7645 = CARTESIAN_POINT ( 'NONE',  ( -32.08353429858341599, -26.68014822793582752, -14.83332872282386816 ) ) ;
#7646 = EDGE_CURVE ( 'NONE', #26649, #24670, #21285, .T. ) ;
#7647 = ADVANCED_FACE ( 'NONE', ( #30807 ), #20566, .F. ) ;
#7648 = VERTEX_POINT ( 'NONE', #30088 ) ;
#7649 = CIRCLE ( 'NONE', #5669, 0.7500000000000006661 ) ;
#7650 = CARTESIAN_POINT ( 'NONE',  ( -21.55879915780394285, -31.64813929209768517, 34.49999999999999289 ) ) ;
#7651 = ADVANCED_FACE ( 'NONE', ( #7253 ), #8723, .T. ) ;
#7652 = CARTESIAN_POINT ( 'NONE',  ( 0.000000000000000000, 1.699320956058915452E-16, -1.500000000000001776 ) ) ;
#7653 = CARTESIAN_POINT ( 'NONE',  ( 9.634323311075775109, 1.438332125858202692, 21.50000000000000000 ) ) ;
#7654 = ORIENTED_EDGE ( 'NONE', *, *, #30373, .T. ) ;
#7655 = EDGE_CURVE ( 'NONE', #20169, #11001, #6388, .T. ) ;
#7656 = CARTESIAN_POINT ( 'NONE',  ( 3.196529495465388226, 8.413215745755008967, 21.50000000000000000 ) ) ;
#7657 = CIRCLE ( 'NONE', #15619, 15.00000000000000000 ) ;
#7658 = ORIENTED_EDGE ( 'NONE', *, *, #25429, .T. ) ;
#7659 = CARTESIAN_POINT ( 'NONE',  ( 6.900000000000000355, 0.000000000000000000, 9.000000000000000000 ) ) ;
#7660 = VECTOR ( 'NONE', #18726, 1000.000000000000000 ) ;
#7661 = CARTESIAN_POINT ( 'NONE',  ( -33.57242512142387625, 24.08458161877161885, -13.16663720014219408 ) ) ;
#7662 = FACE_OUTER_BOUND ( 'NONE', #27843, .T. ) ;
#7663 = ORIENTED_EDGE ( 'NONE', *, *, #30002, .T. ) ;
#7664 = CARTESIAN_POINT ( 'NONE',  ( 48.00277007997793532, 69.90319682561420223, 58.53084797575039744 ) ) ;
#7665 = DIRECTION ( 'NONE',  ( -0.000000000000000000, 0.000000000000000000, 1.000000000000000000 ) ) ;
#7666 = LINE ( 'NONE', #14672, #8856 ) ;
#7667 = DIRECTION ( 'NONE',  ( 1.000000000000000000, 0.000000000000000000, 0.000000000000000000 ) ) ;
#7668 = DIRECTION ( 'NONE',  ( 0.1423148382732889461, 0.9898214418809321291, 0.000000000000000000 ) ) ;
#7669 = CARTESIAN_POINT ( 'NONE',  ( 10.58066667298599661, -16.99307187112385265, 20.12545155307891065 ) ) ;
#7670 = CARTESIAN_POINT ( 'NONE',  ( 32.19782014694307293, 14.25394737442116444, 39.78814634291936159 ) ) ;
#7671 = EDGE_CURVE ( 'NONE', #27143, #30053, #30239, .T. ) ;
#7672 = ORIENTED_EDGE ( 'NONE', *, *, #11194, .T. ) ;
#7673 = EDGE_CURVE ( 'NONE', #26525, #22829, #21445, .T. ) ;
#7674 = CARTESIAN_POINT ( 'NONE',  ( 0.000000000000000000, -2.435693370351110282E-15, 21.50000000000000355 ) ) ;
#7675 = EDGE_CURVE ( 'NONE', #29550, #19640, #29554, .T. ) ;
#7676 = CARTESIAN_POINT ( 'NONE',  ( 39.99999999999998579, 90.00000000000001421, 52.49999999999999289 ) ) ;
#7677 = CARTESIAN_POINT ( 'NONE',  ( 23.96732207938043402, -33.98584080152387088, -1.500000000000000000 ) ) ;
#7678 = LINE ( 'NONE', #21225, #16785 ) ;
#7679 = ADVANCED_FACE ( 'NONE', ( #20034 ), #12719, .F. ) ;
#7680 = ORIENTED_EDGE ( 'NONE', *, *, #8636, .T. ) ;
#7681 = CIRCLE ( 'NONE', #25110, 7.500000000000013323 ) ;
#7682 = CARTESIAN_POINT ( 'NONE',  ( 27.98837345756654926, -29.59714202224856194, 13.23495098233264500 ) ) ;
#7683 = CARTESIAN_POINT ( 'NONE',  ( -45.56537993551197019, 69.19660983124860820, 60.81053982466166730 ) ) ;
#7684 = ADVANCED_FACE ( 'NONE', ( #19889 ), #852, .F. ) ;
#7685 = FACE_OUTER_BOUND ( 'NONE', #8037, .T. ) ;
#7686 = CARTESIAN_POINT ( 'NONE',  ( 127.5000000000000000, 0.000000000000000000, 0.000000000000000000 ) ) ;
#7687 = CARTESIAN_POINT ( 'NONE',  ( 12.56641067637329812, 40.32935944495179115, -1.500000000000000000 ) ) ;
#7688 = EDGE_CURVE ( 'NONE', #26441, #20574, #18128, .T. ) ;
#7689 = CARTESIAN_POINT ( 'NONE',  ( -13.00999358272542494, -0.8602714556717691030, 24.50000000000000000 ) ) ;
#7690 = CARTESIAN_POINT ( 'NONE',  ( 33.03869540315597675, 22.74296903121848956, 30.80490156986919814 ) ) ;
#7691 = EDGE_CURVE ( 'NONE', #28435, #24290, #21909, .T. ) ;
#7693 = CARTESIAN_POINT ( 'NONE',  ( 7.341751895053238108, -5.349779314757616255, 13.22130136205108819 ) ) ;
#7692 = B_SPLINE_CURVE_WITH_KNOTS ( 'NONE', 3,
 ( #1890, #3943, #6428, #25749, #30125, #23401, #30430, #27800, #15943, #8927, #25457, #11417 ),
 .UNSPECIFIED., .F., .F.,
 ( 4, 2, 2, 2, 2, 4 ),
 ( 2.975096543230397156E-07, 0.0009689891193463220660, 0.001937680729038321250, 0.002906372338730320217, 0.003390718143576314497, 0.003875063948422308776 ),
 .UNSPECIFIED. ) ;
#7694 = VERTEX_POINT ( 'NONE', #15184 ) ;
#7695 = CARTESIAN_POINT ( 'NONE',  ( 8.840471615930072247, -1.687027447297460236, 21.50000000000000000 ) ) ;
#7696 = ORIENTED_EDGE ( 'NONE', *, *, #13398, .F. ) ;
#7697 = CARTESIAN_POINT ( 'NONE',  ( 2.168404344971008868E-16, 42.50000000000000711, -1.500000000000000000 ) ) ;
#7698 = FACE_OUTER_BOUND ( 'NONE', #26120, .T. ) ;
#7699 = ORIENTED_EDGE ( 'NONE', *, *, #18925, .T. ) ;
#7700 = ORIENTED_EDGE ( 'NONE', *, *, #26912, .F. ) ;
#7701 = CARTESIAN_POINT ( 'NONE',  ( 12.24063095261064404, 4.490763173670002217, 1.500000000000001332 ) ) ;
#7702 = VERTEX_POINT ( 'NONE', #22058 ) ;
#7703 = ORIENTED_EDGE ( 'NONE', *, *, #13800, .F. ) ;
#7704 = ORIENTED_EDGE ( 'NONE', *, *, #28663, .T. ) ;
#7705 = DIRECTION ( 'NONE',  ( 0.2817325568414296710, 0.9594929736144973687, -0.000000000000000000 ) ) ;
#7706 = AXIS2_PLACEMENT_3D ( 'NONE', #11030, #13381, #15696 ) ;
#7707 = EDGE_CURVE ( 'NONE', #27411, #26330, #700, .T. ) ;
#7708 = CARTESIAN_POINT ( 'NONE',  ( -34.17816363167221994, 12.44541626675085588, 34.50000000000000711 ) ) ;
#7709 = DIRECTION ( 'NONE',  ( 1.000000000000000000, 0.000000000000000000, -0.000000000000000000 ) ) ;
#7710 = EDGE_CURVE ( 'NONE', #23836, #5438, #14730, .T. ) ;
#7711 = CARTESIAN_POINT ( 'NONE',  ( 4.299378382534714937, 16.48726736029805195, 18.37259980046034613 ) ) ;
#7712 = CARTESIAN_POINT ( 'NONE',  ( -32.28307784207223108, 8.475829241206282560, 37.38016955275591613 ) ) ;
#7713 = VERTEX_POINT ( 'NONE', #15036 ) ;
#7714 = CARTESIAN_POINT ( 'NONE',  ( 50.00000000000000000, 6.123233995736766085E-15, 196.3477631085023631 ) ) ;
#7715 = PLANE ( 'NONE',  #24045 ) ;
#7716 = CARTESIAN_POINT ( 'NONE',  ( 1.230359340266124146, -17.01462811240320150, 5.749491821935610147 ) ) ;
#7717 = CARTESIAN_POINT ( 'NONE',  ( 9.056472324687607767, 0.7083562926195454690, 13.22130136205108819 ) ) ;
#7718 = EDGE_CURVE ( 'NONE', #7224, #16079, #21751, .T. ) ;
#7719 = ORIENTED_EDGE ( 'NONE', *, *, #11645, .T. ) ;
#7720 = LINE ( 'NONE', #7408, #3857 ) ;
#7721 = CARTESIAN_POINT ( 'NONE',  ( -17.63988435498683671, -9.462624493092876676, 6.233981582756856987 ) ) ;
#7722 = CARTESIAN_POINT ( 'NONE',  ( -6.065925884476026653, 15.94726461227263847, 5.810767894563978686 ) ) ;
#7723 = CYLINDRICAL_SURFACE ( 'NONE', #23731, 3.559164065751841743 ) ;
#7724 = CARTESIAN_POINT ( 'NONE',  ( -18.24419300814588851, -8.237927942618480159, 18.44501272782439827 ) ) ;
#7725 = DIRECTION ( 'NONE',  ( 1.000000000000000000, 0.000000000000000000, 0.000000000000000000 ) ) ;
#7726 = ORIENTED_EDGE ( 'NONE', *, *, #27673, .F. ) ;
#7727 = VERTEX_POINT ( 'NONE', #2895 ) ;
#7728 = SURFACE_STYLE_USAGE ( .BOTH. , #14586 ) ;
#7729 = AXIS2_PLACEMENT_3D ( 'NONE', #19426, #19893, #22383 ) ;
#7730 = CARTESIAN_POINT ( 'NONE',  ( 20.65888525914559892, 38.75220717792412728, -19.50000000000000355 ) ) ;
#7731 = FACE_OUTER_BOUND ( 'NONE', #5293, .T. ) ;
#7732 = CARTESIAN_POINT ( 'NONE',  ( 9.454746441592959627, -0.7220001660362819207, 21.50000000000000000 ) ) ;
#7733 = ORIENTED_EDGE ( 'NONE', *, *, #22939, .T. ) ;
#7734 = APPLICATION_PROTOCOL_DEFINITION ( 'draft international standard', 'automotive_design', 1998, #5010 ) ;
#7735 = CARTESIAN_POINT ( 'NONE',  ( -2.094186647214675734, 9.248129367672088819, 1.500000000000001332 ) ) ;
#7736 = PLANE ( 'NONE',  #19161 ) ;
#7737 = ORIENTED_EDGE ( 'NONE', *, *, #17620, .T. ) ;
#7738 = CARTESIAN_POINT ( 'NONE',  ( -23.62400240902268322, -9.724154461249517212, 45.23564988763774863 ) ) ;
#7739 = CARTESIAN_POINT ( 'NONE',  ( 19.74328841314634886, 3.194145055459934213, 20.34789198813115263 ) ) ;
#7740 = CARTESIAN_POINT ( 'NONE',  ( -8.546423435383418976, -14.74799740001549786, 18.34798005863078885 ) ) ;
#7741 = CARTESIAN_POINT ( 'NONE',  ( -28.19317390287710623, -29.49677466076099819, 34.53603776002483272 ) ) ;
#7742 = ORIENTED_EDGE ( 'NONE', *, *, #14489, .F. ) ;
#7743 = CARTESIAN_POINT ( 'NONE',  ( 11.77411685406913477, -16.16721897189998103, 6.037995405461183296 ) ) ;
#7744 = EDGE_CURVE ( 'NONE', #6719, #10258, #21528, .T. ) ;
#7745 = CARTESIAN_POINT ( 'NONE',  ( 13.27321688587731607, 41.66719137602760981, -16.50000000000000000 ) ) ;
#7746 = CARTESIAN_POINT ( 'NONE',  ( 11.23874228076938664, -11.06161525231356713, -0.6213203435596476032 ) ) ;
#7747 = EDGE_LOOP ( 'NONE', ( #11188, #21880, #13512, #15472 ) ) ;
#7748 = CARTESIAN_POINT ( 'NONE',  ( -18.15569024355515282, -8.431866758338669499, 5.670038381137163519 ) ) ;
#7749 = VECTOR ( 'NONE', #3127, 1000.000000000000000 ) ;
#7750 = FACE_OUTER_BOUND ( 'NONE', #3071, .T. ) ;
#7751 = CARTESIAN_POINT ( 'NONE',  ( 0.4458717728788724188, -17.03078575579515430, 5.701226463332907279 ) ) ;
#7752 = CARTESIAN_POINT ( 'NONE',  ( -10.00000000000004263, 1.387778780781445676E-14, 24.50000000000000000 ) ) ;
#7753 = PLANE ( 'NONE',  #2853 ) ;
#7754 = FACE_OUTER_BOUND ( 'NONE', #2542, .T. ) ;
#7755 = CARTESIAN_POINT ( 'NONE',  ( 10.47960520055065992, -7.757439966934453146, 24.50000000000000000 ) ) ;
#7756 = EDGE_LOOP ( 'NONE', ( #22981, #27321, #12995, #20912 ) ) ;
#7757 = DIRECTION ( 'NONE',  ( 1.000000000000000000, 0.000000000000000000, 0.000000000000000000 ) ) ;
#7758 = LINE ( 'NONE', #24737, #18061 ) ;
#7759 = ORIENTED_EDGE ( 'NONE', *, *, #23066, .F. ) ;
#7760 = ORIENTED_EDGE ( 'NONE', *, *, #8775, .F. ) ;
#7761 = DIRECTION ( 'NONE',  ( 1.000000000000000000, 0.000000000000000000, 0.000000000000000000 ) ) ;
#7762 = FACE_OUTER_BOUND ( 'NONE', #22571, .T. ) ;
#7763 = EDGE_LOOP ( 'NONE', ( #29336, #358, #5133, #5933 ) ) ;
#7764 = CARTESIAN_POINT ( 'NONE',  ( 15.45595318746689273, 12.72131790141721375, 18.80699882434806369 ) ) ;
#7765 = AXIS2_PLACEMENT_3D ( 'NONE', #2840, #30762, #2219 ) ;
#7766 = CARTESIAN_POINT ( 'NONE',  ( -9.081360402260859388, -14.40588898056578060, 5.862424720655265098 ) ) ;
#7767 = ORIENTED_EDGE ( 'NONE', *, *, #22560, .F. ) ;
#7768 = CARTESIAN_POINT ( 'NONE',  ( -19.73500371898429862, 3.353449004226453312, 7.176035686813569292 ) ) ;
#7769 = CARTESIAN_POINT ( 'NONE',  ( 18.12921809165263198, -8.446683920555065228, 5.775318986477952166 ) ) ;
#7770 = CONICAL_SURFACE ( 'NONE', #15224, 9.000000000000000000, 1.047197551196600296 ) ;
#7771 = DIRECTION ( 'NONE',  ( 1.000000000000000000, 0.000000000000000000, -0.000000000000000000 ) ) ;
#7772 = ORIENTED_EDGE ( 'NONE', *, *, #23123, .F. ) ;
#7773 = VERTEX_POINT ( 'NONE', #5536 ) ;
#7774 = CARTESIAN_POINT ( 'NONE',  ( 19.67838142173201987, 33.09896098428890809, 27.50000000000000000 ) ) ;
#7775 = VERTEX_POINT ( 'NONE', #7732 ) ;
#7776 = CARTESIAN_POINT ( 'NONE',  ( 36.86322900007326808, 13.93456307833209706, 31.62480519666989309 ) ) ;
#7777 = CARTESIAN_POINT ( 'NONE',  ( -6.803558837019167527, 18.82611028990652713, 18.82680253904184298 ) ) ;
#7778 = CARTESIAN_POINT ( 'NONE',  ( -15.20706373417739599, 13.01805446572691594, 20.32842677360128292 ) ) ;
#7779 = DIRECTION ( 'NONE',  ( 0.000000000000000000, 0.000000000000000000, 1.000000000000000000 ) ) ;
#7780 = CIRCLE ( 'NONE', #23213, 4.999999999999997335 ) ;
#7781 = CARTESIAN_POINT ( 'NONE',  ( -36.50611713474064146, -15.17355836286742843, 31.53147891484856657 ) ) ;
#7782 = CARTESIAN_POINT ( 'NONE',  ( -24.03057240117691862, 26.57182937991348481, 24.50000000000000000 ) ) ;
#7783 = DIRECTION ( 'NONE',  ( -0.9898214418809327952, -0.1423148382732853101, 0.000000000000000000 ) ) ;
#7784 = VERTEX_POINT ( 'NONE', #24551 ) ;
#7785 = DIRECTION ( 'NONE',  ( 0.000000000000000000, -1.000000000000000000, 0.000000000000000000 ) ) ;
#7786 = AXIS2_PLACEMENT_3D ( 'NONE', #16437, #25951, #11924 ) ;
#7787 = CARTESIAN_POINT ( 'NONE',  ( 9.436006877828926775, -14.17980878077545981, 7.526951045817043884 ) ) ;
#7788 = ORIENTED_EDGE ( 'NONE', *, *, #27181, .T. ) ;
#7789 = ORIENTED_EDGE ( 'NONE', *, *, #14737, .F. ) ;
#7790 = CARTESIAN_POINT ( 'NONE',  ( -4.668110441710642711, -19.44758969394387194, 1.500000000000001332 ) ) ;
#7791 = CARTESIAN_POINT ( 'NONE',  ( 10.88769261259305310, -16.77715788799338625, 7.626647697317580743 ) ) ;
#7792 = CARTESIAN_POINT ( 'NONE',  ( 16.16296542101254730, 5.939519782021115191, -0.6213203435596476032 ) ) ;
#7793 = CYLINDRICAL_SURFACE ( 'NONE', #22586, 27.70876437800068359 ) ;
#7794 = AXIS2_PLACEMENT_3D ( 'NONE', #10081, #12124, #21778 ) ;
#7795 = DIRECTION ( 'NONE',  ( -1.000000000000000000, 0.000000000000000000, -0.000000000000000000 ) ) ;
#7796 = COLOUR_RGB ( '',0.7921568627450980005, 0.8196078431372548767, 0.9333333333333333481 ) ;
#7797 = CARTESIAN_POINT ( 'NONE',  ( 6.070111251556830290, 19.05682731086507076, 7.267242832833948896 ) ) ;
#7798 = EDGE_LOOP ( 'NONE', ( #24417, #15438, #28209, #12885, #25934, #21826, #11351, #2610, #29123, #8073 ) ) ;
#7799 = CARTESIAN_POINT ( 'NONE',  ( -6.606788361478927563, -38.83273613297759397, 34.49999999999999289 ) ) ;
#7800 = CARTESIAN_POINT ( 'NONE',  ( -35.97269501643903311, 1.773469557544170572, 34.75180443448076062 ) ) ;
#7801 = EDGE_CURVE ( 'NONE', #22741, #17807, #4178, .T. ) ;
#7802 = CARTESIAN_POINT ( 'NONE',  ( 16.79425489945617400, 2.861376016183142745, 7.595116371587256054 ) ) ;
#7803 = ORIENTED_EDGE ( 'NONE', *, *, #5583, .T. ) ;
#7804 = AXIS2_PLACEMENT_3D ( 'NONE', #14616, #567, #22246 ) ;
#7805 = CARTESIAN_POINT ( 'NONE',  ( 15.37106698384762993, 12.82394120857653874, 7.359006845440219102 ) ) ;
#7806 = ORIENTED_EDGE ( 'NONE', *, *, #11146, .F. ) ;
#7807 = DIRECTION ( 'NONE',  ( -0.000000000000000000, -0.000000000000000000, -1.000000000000000000 ) ) ;
#7808 = CIRCLE ( 'NONE', #5833, 1.000000000000008438 ) ;
#7809 = CARTESIAN_POINT ( 'NONE',  ( -7.028330626922778990, 10.93629592680536788, 1.500000000000001332 ) ) ;
#7810 = AXIS2_PLACEMENT_3D ( 'NONE', #16304, #20105, #6635 ) ;
#7811 = DIRECTION ( 'NONE',  ( -0.000000000000000000, -0.000000000000000000, -1.000000000000000000 ) ) ;
#7812 = ORIENTED_EDGE ( 'NONE', *, *, #28636, .F. ) ;
#7813 = EDGE_CURVE ( 'NONE', #10221, #23441, #12565, .T. ) ;
#7814 = CARTESIAN_POINT ( 'NONE',  ( 24.03057240117690441, -26.57182937991349903, 26.54355021145563143 ) ) ;
#7815 = EDGE_CURVE ( 'NONE', #28813, #9106, #22094, .T. ) ;
#7816 = DIRECTION ( 'NONE',  ( 0.000000000000000000, 0.000000000000000000, -1.000000000000000000 ) ) ;
#7817 = CARTESIAN_POINT ( 'NONE',  ( -9.824744466605366711, -8.513189541288717521, 24.50000000000000000 ) ) ;
#7818 = CARTESIAN_POINT ( 'NONE',  ( 33.17909676736307034, 15.33239136497788913, 34.49999999999997868 ) ) ;
#7819 = AXIS2_PLACEMENT_3D ( 'NONE', #16301, #18958, #24078 ) ;
#7820 = CARTESIAN_POINT ( 'NONE',  ( -13.89991139849285773, 7.447222512978775022, 1.500000000000001332 ) ) ;
#7821 = DIRECTION ( 'NONE',  ( 0.000000000000000000, 0.000000000000000000, 1.000000000000000000 ) ) ;
#7822 = FACE_OUTER_BOUND ( 'NONE', #11714, .T. ) ;
#7823 = ORIENTED_EDGE ( 'NONE', *, *, #7673, .T. ) ;
#7824 = DIRECTION ( 'NONE',  ( 0.000000000000000000, 0.000000000000000000, 1.000000000000000000 ) ) ;
#7825 = AXIS2_PLACEMENT_3D ( 'NONE', #22961, #3959, #18460 ) ;
#7826 = CARTESIAN_POINT ( 'NONE',  ( -13.77701868333377178, 10.07013474916661266, 20.13759033520874908 ) ) ;
#7827 = DIRECTION ( 'NONE',  ( 0.000000000000000000, -0.000000000000000000, -1.000000000000000000 ) ) ;
#7828 = ORIENTED_EDGE ( 'NONE', *, *, #26922, .F. ) ;
#7830 = ADVANCED_FACE ( 'NONE', ( #16126, #13177 ), #6150, .T. ) ;
#7829 = VECTOR ( 'NONE', #8528, 1000.000000000000000 ) ;
#7831 = CARTESIAN_POINT ( 'NONE',  ( 32.40545545705547426, -23.64849546015198811, 17.96741959276885581 ) ) ;
#7832 = CARTESIAN_POINT ( 'NONE',  ( -42.15079822434952916, 66.40050670621626239, 62.28253961994978738 ) ) ;
#7833 = CARTESIAN_POINT ( 'NONE',  ( 35.78163722268750746, -27.43648963448195133, -11.49999999999999645 ) ) ;
#7834 = AXIS2_PLACEMENT_3D ( 'NONE', #26047, #9667, #26510 ) ;
#7835 = CARTESIAN_POINT ( 'NONE',  ( -13.22505861668184046, -42.10773672057003125, -19.50000000000000355 ) ) ;
#7836 = CARTESIAN_POINT ( 'NONE',  ( 7.724883619896791842, 5.687793815610376669, 21.50000000000000000 ) ) ;
#7837 = AXIS2_PLACEMENT_3D ( 'NONE', #11186, #22716, #27884 ) ;
#7838 = CYLINDRICAL_SURFACE ( 'NONE', #17022, 1.999999999999998224 ) ;
#7839 = EDGE_LOOP ( 'NONE', ( #18769, #882 ) ) ;
#7840 = VECTOR ( 'NONE', #23564, 1000.000000000000000 ) ;
#7841 = CARTESIAN_POINT ( 'NONE',  ( 33.03787114092997257, -23.27353420009123042, -4.833239141675072403 ) ) ;
#7842 = CIRCLE ( 'NONE', #14799, 10.00000000000003197 ) ;
#7843 = CARTESIAN_POINT ( 'NONE',  ( 1.836970198721029589E-15, -14.99999999999997158, -70.00000000000000000 ) ) ;
#7844 = CARTESIAN_POINT ( 'NONE',  ( -18.04365185506139113, -8.627086862512678422, 20.34789198813115263 ) ) ;
#7845 = VERTEX_POINT ( 'NONE', #15657 ) ;
#7846 = EDGE_CURVE ( 'NONE', #1564, #26699, #18165, .T. ) ;
#7847 = ORIENTED_EDGE ( 'NONE', *, *, #10125, .F. ) ;
#7848 = AXIS2_PLACEMENT_3D ( 'NONE', #26689, #12813, #22311 ) ;
#7849 = EDGE_CURVE ( 'NONE', #24302, #9342, #24016, .T. ) ;
#7850 = DIRECTION ( 'NONE',  ( -0.000000000000000000, 0.000000000000000000, 1.000000000000000000 ) ) ;
#7851 = VERTEX_POINT ( 'NONE', #27674 ) ;
#7852 = ORIENTED_EDGE ( 'NONE', *, *, #2103, .T. ) ;
#7853 = CARTESIAN_POINT ( 'NONE',  ( -50.00000000000000000, 0.000000000000000000, 12.49999999999998401 ) ) ;
#7854 = CIRCLE ( 'NONE', #8354, 15.00000000000000000 ) ;
#7855 = ADVANCED_FACE ( 'NONE', ( #20346, #27981, #25494 ), #25170, .T. ) ;
#7856 = CARTESIAN_POINT ( 'NONE',  ( -23.07950435457351190, 11.50806656539842798, 49.21048435262080289 ) ) ;
#7857 = EDGE_CURVE ( 'NONE', #4888, #13891, #13495, .T. ) ;
#7858 = CARTESIAN_POINT ( 'NONE',  ( -4.163336342344337027E-14, 1.387778780781445676E-14, 62.49999999999999289 ) ) ;
#7859 = AXIS2_PLACEMENT_3D ( 'NONE', #29998, #27966, #15637 ) ;
#7860 = CARTESIAN_POINT ( 'NONE',  ( -37.95344354766306338, 9.779784673403119299, 13.60598863365600053 ) ) ;
#7861 = FACE_OUTER_BOUND ( 'NONE', #24700, .T. ) ;
#7862 = VERTEX_POINT ( 'NONE', #13649 ) ;
#7863 = EDGE_CURVE ( 'NONE', #2852, #11596, #11147, .T. ) ;
#7864 = DIRECTION ( 'NONE',  ( -0.000000000000000000, 1.000000000000000000, -0.000000000000000000 ) ) ;
#7865 = CARTESIAN_POINT ( 'NONE',  ( -32.50000000000000000, 0.000000000000000000, -52.50000000000000000 ) ) ;
#7866 = DIRECTION ( 'NONE',  ( 0.000000000000000000, -1.132880637372608986E-16, 1.000000000000000000 ) ) ;
#7867 = VECTOR ( 'NONE', #21453, 1000.000000000000114 ) ;
#7868 = EDGE_CURVE ( 'NONE', #12720, #21119, #16627, .T. ) ;
#7869 = ORIENTED_EDGE ( 'NONE', *, *, #21854, .T. ) ;
#7870 = B_SPLINE_CURVE_WITH_KNOTS ( 'NONE', 3,
 ( #27952, #1739, #30729, #23547, #7029, #20752, #30433, #13615, #9377, #1894, #25754, #4384, #19040, #18733, #28247, #6581, #6876, #16391 ),
 .UNSPECIFIED., .F., .F.,
 ( 4, 2, 2, 2, 2, 2, 2, 2, 4 ),
 ( 0.000000000000000000, 0.0003967869494442868004, 0.0007935738988885736008, 0.001190360848332860455, 0.001587147797777147202, 0.001983934747221434165, 0.002380721696665720911, 0.002777508646110007657, 0.003174295595554294403 ),
 .UNSPECIFIED. ) ;
#7871 = VECTOR ( 'NONE', #30378, 1000.000000000000000 ) ;
#7872 = AXIS2_PLACEMENT_3D ( 'NONE', #13814, #16302, #16753 ) ;
#7873 = CARTESIAN_POINT ( 'NONE',  ( 0.000000000000000000, 0.000000000000000000, -87.50000000000000000 ) ) ;
#7874 = CARTESIAN_POINT ( 'NONE',  ( -5.694318326875604797, 16.07090250511087604, 5.661398277488801867 ) ) ;
#7875 = EDGE_CURVE ( 'NONE', #24589, #25420, #28582, .T. ) ;
#7876 = DIRECTION ( 'NONE',  ( -0.000000000000000000, -0.000000000000000000, -1.000000000000000000 ) ) ;
#7877 = CARTESIAN_POINT ( 'NONE',  ( -18.32390295431236282, -8.059524160852181041, 18.55820869691756769 ) ) ;
#7878 = FACE_OUTER_BOUND ( 'NONE', #15539, .T. ) ;
#7879 = CIRCLE ( 'NONE', #25798, 0.7500000000000006661 ) ;
#7880 = ORIENTED_EDGE ( 'NONE', *, *, #25501, .F. ) ;
#7881 = ORIENTED_EDGE ( 'NONE', *, *, #8042, .F. ) ;
#7882 = CIRCLE ( 'NONE', #13362, 0.7500000000000006661 ) ;
#7883 = DIRECTION ( 'NONE',  ( 0.000000000000000000, 0.000000000000000000, 1.000000000000000000 ) ) ;
#7884 = CARTESIAN_POINT ( 'NONE',  ( 2.687479363073301819, 44.39187623479102740, -19.50000000000000355 ) ) ;
#7885 = FACE_OUTER_BOUND ( 'NONE', #25076, .T. ) ;
#7886 = DIRECTION ( 'NONE',  ( 0.000000000000000000, 0.000000000000000000, -1.000000000000000000 ) ) ;
#7887 = EDGE_LOOP ( 'NONE', ( #5363, #4056 ) ) ;
#7888 = APPLICATION_PROTOCOL_DEFINITION ( 'draft international standard', 'automotive_design', 1998, #26935 ) ;
#7889 = CARTESIAN_POINT ( 'NONE',  ( -4.163336342344337027E-14, 1.387778780781445676E-14, 37.50000000000000000 ) ) ;
#7890 = LINE ( 'NONE', #543, #24136 ) ;
#7891 = EDGE_CURVE ( 'NONE', #30269, #27691, #11160, .T. ) ;
#7892 = CIRCLE ( 'NONE', #5900, 1.000000000000007772 ) ;
#7893 = ORIENTED_EDGE ( 'NONE', *, *, #8454, .F. ) ;
#7894 = CARTESIAN_POINT ( 'NONE',  ( -10.00000000000004263, 1.387778780781445676E-14, 24.50000000000000000 ) ) ;
#7895 = EDGE_CURVE ( 'NONE', #27782, #4693, #11294, .T. ) ;
#7896 = B_SPLINE_SURFACE_WITH_KNOTS ( 'NONE', 3, 1, ( 
 ( #22780, #18434 ),
 ( #27627, #27475 ),
 ( #6563, #25124 ),
 ( #25444, #15931 ),
 ( #20448, #24970 ),
 ( #8606, #5953 ),
 ( #25591, #1273 ),
 ( #27324, #15451 ),
 ( #13596, #23074 ),
 ( #11237, #8910 ),
 ( #6251, #30264 ),
 ( #3608, #11402 ),
 ( #29656, #1722 ),
 ( #20732, #30113 ),
 ( #16075, #15761 ),
 ( #3929, #3766 ),
 ( #22932, #13285 ),
 ( #13129, #22623 ),
 ( #1435, #11094 ),
 ( #10781, #27785 ),
 ( #20588, #20296 ),
 ( #8293, #29822 ),
 ( #4211, #8744 ),
 ( #6096, #23224 ),
 ( #10950, #15606 ),
 ( #8464, #1878 ),
 ( #17809, #18264 ),
 ( #17966, #13887 ),
 ( #14492, #4982 ),
 ( #23534, #9201 ),
 ( #28539, #23993 ) ),
 .UNSPECIFIED., .F., .F., .F.,
 ( 4, 3, 3, 3, 3, 3, 3, 3, 3, 3, 4 ),
 ( 2, 2 ),
 ( 0.000000000000000000, 0.05425176834609633791, 0.1085332949128352958, 0.1623767749169382768, 0.2157504826133063158, 0.2688657508888171455, 0.3218907763505476360, 0.3749548578363336993, 0.4282048033836242107, 0.4818374082110501444, 0.4999999999131659045 ),
 ( 0.000000000000000000, 1.000000000000000000 ),
 .UNSPECIFIED. ) ;
#7897 = CIRCLE ( 'NONE', #25320, 0.7500000000000006661 ) ;
#7898 = FACE_OUTER_BOUND ( 'NONE', #18543, .T. ) ;
#7899 = AXIS2_PLACEMENT_3D ( 'NONE', #24312, #2963, #17609 ) ;
#7900 = CARTESIAN_POINT ( 'NONE',  ( -7.671651850954195773, -15.25824679864874511, 19.28454053338349183 ) ) ;
#7901 = CARTESIAN_POINT ( 'NONE',  ( -38.35800364550046027, -7.710258930485773377, 35.01326192470217080 ) ) ;
#7902 = ORIENTED_EDGE ( 'NONE', *, *, #4599, .T. ) ;
#7903 = CARTESIAN_POINT ( 'NONE',  ( 11.62196639741666004, -16.27693748946514418, 5.853797745100183469 ) ) ;
#7904 = FACE_OUTER_BOUND ( 'NONE', #23645, .T. ) ;
#7905 = CARTESIAN_POINT ( 'NONE',  ( 8.303920738747214259, 3.683253992019856149, -1.500000000000001332 ) ) ;
#7906 = VECTOR ( 'NONE', #30468, 1000.000000000000000 ) ;
#7907 = CARTESIAN_POINT ( 'NONE',  ( -19.82747825358059401, 2.624647641736350234, 18.34726407865098707 ) ) ;
#7908 = EDGE_LOOP ( 'NONE', ( #13926, #2087, #8958, #6171 ) ) ;
#7909 = DIRECTION ( 'NONE',  ( 0.000000000000000000, -0.000000000000000000, -1.000000000000000000 ) ) ;
#7910 = CARTESIAN_POINT ( 'NONE',  ( -4.163336342344337027E-14, 1.387778780781445676E-14, 24.50000000000000000 ) ) ;
#7911 = CARTESIAN_POINT ( 'NONE',  ( 15.91781874854195422, -6.122627424449554212, 7.652108011868850035 ) ) ;
#7912 = EDGE_CURVE ( 'NONE', #13171, #14352, #29592, .T. ) ;
#7913 = DIRECTION ( 'NONE',  ( -0.000000000000000000, -0.000000000000000000, -1.000000000000000000 ) ) ;
#7914 = CARTESIAN_POINT ( 'NONE',  ( -12.24063095261064227, 4.490763173670005770, 1.500000000000001332 ) ) ;
#7915 = DIRECTION ( 'NONE',  ( -0.000000000000000000, 0.000000000000000000, 1.000000000000000000 ) ) ;
#7916 = CARTESIAN_POINT ( 'NONE',  ( 34.22030469044062073, -20.42639397296790804, 8.120957071897569435 ) ) ;
#7917 = DIRECTION ( 'NONE',  ( -0.000000000000000000, -0.000000000000000000, 1.000000000000000000 ) ) ;
#7918 = VERTEX_POINT ( 'NONE', #3813 ) ;
#7919 = CIRCLE ( 'NONE', #13403, 9.482273699623480212 ) ;
#7920 = CARTESIAN_POINT ( 'NONE',  ( 8.840471615930072247, -1.687027447297460236, 21.50000000000000000 ) ) ;
#7921 = LINE ( 'NONE', #12746, #18572 ) ;
#7922 = AXIS2_PLACEMENT_3D ( 'NONE', #21935, #2766, #24430 ) ;
#7923 = VERTEX_POINT ( 'NONE', #3514 ) ;
#7924 = AXIS2_PLACEMENT_3D ( 'NONE', #27488, #17980, #15463 ) ;
#7925 = ORIENTED_EDGE ( 'NONE', *, *, #7140, .F. ) ;
#7926 = FACE_OUTER_BOUND ( 'NONE', #16867, .T. ) ;
#7927 = EDGE_CURVE ( 'NONE', #28059, #10427, #2687, .T. ) ;
#7928 = CARTESIAN_POINT ( 'NONE',  ( -5.311554845790392498, 49.71917005564084491, -40.96330688025074807 ) ) ;
#7929 = ORIENTED_EDGE ( 'NONE', *, *, #4703, .F. ) ;
#7930 = EDGE_CURVE ( 'NONE', #18437, #3296, #29876, .T. ) ;
#7931 = AXIS2_PLACEMENT_3D ( 'NONE', #24645, #19813, #7981 ) ;
#7932 = DIRECTION ( 'NONE',  ( 0.000000000000000000, 0.000000000000000000, -1.000000000000000000 ) ) ;
#7933 = CARTESIAN_POINT ( 'NONE',  ( 12.35522127274689375, 11.74279147932066003, 18.34798005862930736 ) ) ;
#7934 = ORIENTED_EDGE ( 'NONE', *, *, #27856, .F. ) ;
#7935 = CARTESIAN_POINT ( 'NONE',  ( -16.82936799811533035, 2.561302842313196049, 7.080843742048788414 ) ) ;
#7936 = CARTESIAN_POINT ( 'NONE',  ( 16.63252861691851692, 3.817440173033144202, 20.13759033520874908 ) ) ;
#7937 = CARTESIAN_POINT ( 'NONE',  ( 40.05520465696179855, -7.028746455191999587, -16.50000000000000000 ) ) ;
#7938 = VERTEX_POINT ( 'NONE', #10674 ) ;
#7939 = DIRECTION ( 'NONE',  ( -0.9096319953545183301, -0.4154150130018863796, -0.000000000000000000 ) ) ;
#7940 = EDGE_LOOP ( 'NONE', ( #18521, #8804 ) ) ;
#7941 = DIRECTION ( 'NONE',  ( 0.000000000000000000, 1.000000000000000000, 1.193512090021232842E-16 ) ) ;
#7942 = AXIS2_PLACEMENT_3D ( 'NONE', #16000, #25668, #4288 ) ;
#7943 = AXIS2_PLACEMENT_3D ( 'NONE', #7889, #17081, #7579 ) ;
#7944 = ORIENTED_EDGE ( 'NONE', *, *, #18508, .T. ) ;
#7945 = CARTESIAN_POINT ( 'NONE',  ( -25.47847050916411504, 26.57182937991348481, 26.54355021145563143 ) ) ;
#7946 = CARTESIAN_POINT ( 'NONE',  ( 37.92610032463591807, 10.23617371602907689, 31.90285370532496856 ) ) ;
#7947 = CARTESIAN_POINT ( 'NONE',  ( 16.60164139905475267, 3.971857776421113595, 7.280727868105637768 ) ) ;
#7948 = CARTESIAN_POINT ( 'NONE',  ( -14.72475726066618051, 13.56098618572340619, 19.00652017443069752 ) ) ;
#7949 = AXIS2_PLACEMENT_3D ( 'NONE', #23239, #9069, #27640 ) ;
#7950 = DIRECTION ( 'NONE',  ( -0.000000000000000000, -0.000000000000000000, 1.000000000000000000 ) ) ;
#7951 = CARTESIAN_POINT ( 'NONE',  ( -37.86918475753925861, -10.24225134995086073, 31.89299558116904265 ) ) ;
#7952 = DIRECTION ( 'NONE',  ( 1.000000000000000000, 0.000000000000000000, 0.000000000000000000 ) ) ;
#7953 = CARTESIAN_POINT ( 'NONE',  ( 9.184850993605159777E-16, -7.500000000000007994, -87.50000000000000000 ) ) ;
#7954 = ORIENTED_EDGE ( 'NONE', *, *, #8534, .F. ) ;
#7955 = CARTESIAN_POINT ( 'NONE',  ( -19.92178149465837578, 1.957245511797580217, 5.810767894563978686 ) ) ;
#7956 = FACE_OUTER_BOUND ( 'NONE', #14159, .T. ) ;
#7957 = LINE ( 'NONE', #2536, #12094 ) ;
#7958 = LINE ( 'NONE', #1510, #1938 ) ;
#7959 = ORIENTED_EDGE ( 'NONE', *, *, #789, .F. ) ;
#7960 = ORIENTED_EDGE ( 'NONE', *, *, #15331, .T. ) ;
#7961 = CARTESIAN_POINT ( 'NONE',  ( 23.21352257770656635, -10.78826658734920052, 45.15942333309103418 ) ) ;
#7962 = DIRECTION ( 'NONE',  ( 0.1423148382732746797, -0.9898214418809342385, 0.000000000000000000 ) ) ;
#7963 = PRODUCT ( 'Housing  Cover Cap', 'Housing  Cover Cap', '', ( #7578 ) ) ;
#7964 = CARTESIAN_POINT ( 'NONE',  ( 18.67280747382547190, -7.164419611389371667, 18.84486140012301547 ) ) ;
#7965 = EDGE_LOOP ( 'NONE', ( #19488, #8423 ) ) ;
#7966 = DIRECTION ( 'NONE',  ( 0.000000000000000000, -1.132880637372608986E-16, 1.000000000000000000 ) ) ;
#7967 = LINE ( 'NONE', #17473, #21626 ) ;
#7968 = EDGE_CURVE ( 'NONE', #12097, #2241, #13336, .T. ) ;
#7969 = EDGE_CURVE ( 'NONE', #15053, #5977, #14070, .T. ) ;
#7970 = CARTESIAN_POINT ( 'NONE',  ( 6.962021646281529641, 6.437683520590196551, 13.00000000000000178 ) ) ;
#7971 = ORIENTED_EDGE ( 'NONE', *, *, #28194, .T. ) ;
#7972 = CARTESIAN_POINT ( 'NONE',  ( -10.29013980557132690, -17.15015428632898775, 20.32200205377525393 ) ) ;
#7973 = AXIS2_PLACEMENT_3D ( 'NONE', #9489, #21641, #7303 ) ;
#7974 = CARTESIAN_POINT ( 'NONE',  ( 11.72050123711542113, 12.41739018441317910, 6.233981582756856987 ) ) ;
#7975 = CARTESIAN_POINT ( 'NONE',  ( 19.76130408545751749, 3.194145055459935101, 7.652108011868850035 ) ) ;
#7976 = ORIENTED_EDGE ( 'NONE', *, *, #19143, .F. ) ;
#7977 = CARTESIAN_POINT ( 'NONE',  ( -5.604556300746500241, -15.53790034020399169, -0.6213203435596476032 ) ) ;
#7978 = EDGE_LOOP ( 'NONE', ( #10179, #15294, #570, #28682 ) ) ;
#7979 = DIRECTION ( 'NONE',  ( 1.000000000000000000, 1.734723475976805517E-15, 0.000000000000000000 ) ) ;
#7980 = UNCERTAINTY_MEASURE_WITH_UNIT (LENGTH_MEASURE( 1.000000000000000082E-05 ), #8840, 'distance_accuracy_value', 'NONE');
#7981 = DIRECTION ( 'NONE',  ( -1.000000000000000000, 0.000000000000000000, 0.000000000000000000 ) ) ;
#7982 = AXIS2_PLACEMENT_3D ( 'NONE', #26280, #24088, #21906 ) ;
#7983 = CARTESIAN_POINT ( 'NONE',  ( 3.685570353517261477, -16.10136545388692397, 1.500000000000000000 ) ) ;
#7984 = EDGE_LOOP ( 'NONE', ( #26934, #11570, #12128, #27524 ) ) ;
#7985 = CARTESIAN_POINT ( 'NONE',  ( 47.59023918323793367, 69.85947342368727675, 59.04212144534069040 ) ) ;
#7986 = CARTESIAN_POINT ( 'NONE',  ( 0.000000000000000000, 0.000000000000000000, 6.000000000000001776 ) ) ;
#7987 = DIRECTION ( 'NONE',  ( -0.000000000000000000, -0.000000000000000000, -1.000000000000000000 ) ) ;
#7988 = CARTESIAN_POINT ( 'NONE',  ( 27.86772728142310740, 25.09083747725281555, 34.49999999999999289 ) ) ;
#7989 = LINE ( 'NONE', #17332, #12909 ) ;
#7990 = CARTESIAN_POINT ( 'NONE',  ( 10.92346103252092604, -16.77505673787610974, 20.32842677360128292 ) ) ;
#7991 = ORIENTED_EDGE ( 'NONE', *, *, #15918, .F. ) ;
#7992 = CYLINDRICAL_SURFACE ( 'NONE', #2841, 12.66227964008302287 ) ;
#7993 = DIRECTION ( 'NONE',  ( -0.000000000000000000, 0.000000000000000000, 1.000000000000000000 ) ) ;
#7994 = CIRCLE ( 'NONE', #18942, 0.7500000000000006661 ) ;
#7995 = CARTESIAN_POINT ( 'NONE',  ( -13.59632618586111619, 10.29740991163845010, 18.39992786714538298 ) ) ;
#7996 = CARTESIAN_POINT ( 'NONE',  ( 43.96625041971210379, 68.08819673771459691, 61.68659123583229587 ) ) ;
#7997 = EDGE_LOOP ( 'NONE', ( #10287, #29351, #25224, #11377 ) ) ;
#7998 = CARTESIAN_POINT ( 'NONE',  ( 28.11261193835277084, -29.45712586627402985, 14.13030833143228371 ) ) ;
#7999 = LINE ( 'NONE', #12828, #24717 ) ;
#8000 = DIRECTION ( 'NONE',  ( -0.5406408174555976665, 0.8412535328311812055, 0.000000000000000000 ) ) ;
#8001 = CARTESIAN_POINT ( 'NONE',  ( -10.64374042650075403, -42.96126232887726815, -19.50000000000000355 ) ) ;
#8002 = AXIS2_PLACEMENT_3D ( 'NONE', #7535, #2385, #4877 ) ;
#8003 = FACE_BOUND ( 'NONE', #26448, .T. ) ;
#8004 = EDGE_CURVE ( 'NONE', #7607, #26631, #25022, .T. ) ;
#8005 = CARTESIAN_POINT ( 'NONE',  ( 15.48300807700231019, 34.15967020736680837, 37.50000000001828937 ) ) ;
#8006 = DIRECTION ( 'NONE',  ( 1.000000000000000000, 0.000000000000000000, 0.000000000000000000 ) ) ;
#8007 = ORIENTED_EDGE ( 'NONE', *, *, #24456, .T. ) ;
#8008 = CARTESIAN_POINT ( 'NONE',  ( 26.81368379037234817, 6.366017791192970066, 43.19835251265425313 ) ) ;
#8009 = ORIENTED_EDGE ( 'NONE', *, *, #27729, .T. ) ;
#8010 = DIRECTION ( 'NONE',  ( -0.000000000000000000, 1.132880637372608986E-16, -1.000000000000000000 ) ) ;
#8011 = CARTESIAN_POINT ( 'NONE',  ( -1.073881485057738949, 0.9711784013061123266, 1.500000000000000000 ) ) ;
#8012 = ORIENTED_EDGE ( 'NONE', *, *, #24279, .T. ) ;
#8013 = ORIENTED_EDGE ( 'NONE', *, *, #18029, .T. ) ;
#8014 = CARTESIAN_POINT ( 'NONE',  ( -9.982956658368037139, -17.33059308371925766, 7.454606537396337274 ) ) ;
#8015 = AXIS2_PLACEMENT_3D ( 'NONE', #1860, #30543, #9040 ) ;
#8016 = VERTEX_POINT ( 'NONE', #30017 ) ;
#8017 = DIRECTION ( 'NONE',  ( -1.000000000000000000, 0.000000000000000000, 0.000000000000000000 ) ) ;
#8018 = CARTESIAN_POINT ( 'NONE',  ( -23.81715554101158006, 29.69269061775747787, 34.50000000000000000 ) ) ;
#8019 = CARTESIAN_POINT ( 'NONE',  ( 27.75715622479469147, -6.315477654728063328E-15, 1.500000000000000000 ) ) ;
#8020 = CARTESIAN_POINT ( 'NONE',  ( -35.77650053662277685, 16.96546617299160076, 8.812125201147090081 ) ) ;
#8021 = CARTESIAN_POINT ( 'NONE',  ( -21.14898501148481813, 24.45236287589831292, -16.50001200000000523 ) ) ;
#8022 = ORIENTED_EDGE ( 'NONE', *, *, #21930, .T. ) ;
#8023 = DIRECTION ( 'NONE',  ( -0.000000000000000000, -0.000000000000000000, 1.000000000000000000 ) ) ;
#8024 = CARTESIAN_POINT ( 'NONE',  ( -24.35970437652574105, -13.37404834226503070, 42.96778633356041865 ) ) ;
#8025 = FACE_OUTER_BOUND ( 'NONE', #6084, .T. ) ;
#8026 = DIRECTION ( 'NONE',  ( 1.000000000000000000, 0.000000000000000000, 0.000000000000000000 ) ) ;
#8027 = EDGE_LOOP ( 'NONE', ( #8872, #737, #20334, #5541 ) ) ;
#8028 = CARTESIAN_POINT ( 'NONE',  ( -18.06093561247157808, -8.632161831585827727, 7.652108011868850035 ) ) ;
#8029 = CARTESIAN_POINT ( 'NONE',  ( -6.737371319102178013, 18.84978071134531064, 6.041646659195333058 ) ) ;
#8030 = CARTESIAN_POINT ( 'NONE',  ( 10.46384303394386528, -13.48464439008897919, 5.951255046771932733 ) ) ;
#8031 = EDGE_CURVE ( 'NONE', #14465, #681, #10766, .T. ) ;
#8032 = AXIS2_PLACEMENT_3D ( 'NONE', #19695, #7709, #15323 ) ;
#8033 = CARTESIAN_POINT ( 'NONE',  ( 12.56641067637329812, 40.32935944495179115, -1.500000000000000000 ) ) ;
#8034 = AXIS2_PLACEMENT_3D ( 'NONE', #1656, #22692, #22546 ) ;
#8035 = CARTESIAN_POINT ( 'NONE',  ( -33.01877980957529957, -12.12572312222180315, 35.60092001944731521 ) ) ;
#8036 = VERTEX_POINT ( 'NONE', #9104 ) ;
#8037 = EDGE_LOOP ( 'NONE', ( #15704, #14677, #26407, #12702 ) ) ;
#8038 = DIRECTION ( 'NONE',  ( -0.2817325568414292825, -0.9594929736144974797, 0.000000000000000000 ) ) ;
#8039 = EDGE_CURVE ( 'NONE', #1352, #30322, #26533, .T. ) ;
#8040 = DIRECTION ( 'NONE',  ( 0.000000000000000000, 0.000000000000000000, -1.000000000000000000 ) ) ;
#8041 = CARTESIAN_POINT ( 'NONE',  ( -13.02951369420309469, 10.96858531083378452, 5.796888747622817029 ) ) ;
#8042 = EDGE_CURVE ( 'NONE', #12536, #17576, #20937, .T. ) ;
#8043 = CARTESIAN_POINT ( 'NONE',  ( -0.02788623102222363703, -17.02558298240596102, 7.267659094423557953 ) ) ;
#8044 = VERTEX_POINT ( 'NONE', #30771 ) ;
#8045 = PLANE ( 'NONE',  #2952 ) ;
#8046 = CARTESIAN_POINT ( 'NONE',  ( 9.958038337755681368, 17.34466697471553331, 24.50000000000000000 ) ) ;
#8047 = ADVANCED_FACE ( 'NONE', ( #13937 ), #25644, .T. ) ;
#8048 = VERTEX_POINT ( 'NONE', #6757 ) ;
#8049 = EDGE_CURVE ( 'NONE', #9427, #24441, #14395, .T. ) ;
#8050 = CARTESIAN_POINT ( 'NONE',  ( -7.695850205855595760, -15.24499612925306913, 19.61324152429826739 ) ) ;
#8051 = CARTESIAN_POINT ( 'NONE',  ( -37.53333450813131833, 2.083350403252341998, 37.49999999994167865 ) ) ;
#8052 = ORIENTED_EDGE ( 'NONE', *, *, #24489, .F. ) ;
#8053 = CARTESIAN_POINT ( 'NONE',  ( -37.99999999999999289, 70.00000000000000000, -34.49999999999999289 ) ) ;
#8054 = ADVANCED_FACE ( 'NONE', ( #23902 ), #18773, .F. ) ;
#8055 = AXIS2_PLACEMENT_3D ( 'NONE', #13151, #22642, #17993 ) ;
#8056 = DIRECTION ( 'NONE',  ( 0.000000000000000000, 0.000000000000000000, -1.000000000000000000 ) ) ;
#8057 = DIRECTION ( 'NONE',  ( 1.000000000000000000, 0.000000000000000000, -0.000000000000000000 ) ) ;
#8058 = ORIENTED_EDGE ( 'NONE', *, *, #19531, .T. ) ;
#8059 = LINE ( 'NONE', #5865, #857 ) ;
#8060 = CARTESIAN_POINT ( 'NONE',  ( 13.01334791338956975, 10.97165762312710946, 19.21496526180054332 ) ) ;
#8061 = CARTESIAN_POINT ( 'NONE',  ( 16.14871318124067301, -5.543368461261742652, 6.147510495896839622 ) ) ;
#8062 = CARTESIAN_POINT ( 'NONE',  ( -7.730328572437709767, 4.608906612435681005, -1.500000000000001332 ) ) ;
#8063 = CARTESIAN_POINT ( 'NONE',  ( -32.19782014694307293, 14.25394737442115733, 35.54550565580015586 ) ) ;
#8064 = FACE_OUTER_BOUND ( 'NONE', #12470, .T. ) ;
#8065 = CARTESIAN_POINT ( 'NONE',  ( 35.77999848792182291, -16.92214645512589755, 17.15740857515053364 ) ) ;
#8066 = CARTESIAN_POINT ( 'NONE',  ( 5.881244434206234217, 6.812559277181991391, 21.50000000000000000 ) ) ;
#8067 = ORIENTED_EDGE ( 'NONE', *, *, #15231, .F. ) ;
#8068 = ADVANCED_FACE ( 'NONE', ( #19216 ), #26240, .F. ) ;
#8069 = ADVANCED_FACE ( 'NONE', ( #6918 ), #4261, .F. ) ;
#8070 = VECTOR ( 'NONE', #27589, 1000.000000000000000 ) ;
#8071 = LINE ( 'NONE', #29730, #11786 ) ;
#8072 = DIRECTION ( 'NONE',  ( -0.000000000000000000, 0.000000000000000000, 1.000000000000000000 ) ) ;
#8073 = ORIENTED_EDGE ( 'NONE', *, *, #5276, .T. ) ;
#8074 = EDGE_CURVE ( 'NONE', #21028, #18115, #23285, .T. ) ;
#8075 = ORIENTED_EDGE ( 'NONE', *, *, #29575, .T. ) ;
#8076 = CYLINDRICAL_SURFACE ( 'NONE', #14140, 1.447898107987198646 ) ;
#8077 = CARTESIAN_POINT ( 'NONE',  ( -7.943622683424091058, 49.36666681218739683, -67.73329464138640787 ) ) ;
#8078 = ADVANCED_FACE ( 'NONE', ( #21407, #2226, #25795 ), #30461, .T. ) ;
#8079 = CIRCLE ( 'NONE', #22016, 0.7500000000000006661 ) ;
#8080 = CARTESIAN_POINT ( 'NONE',  ( 6.778663211761462470, -6.630478080506934546, 13.00000000000000178 ) ) ;
#8081 = EDGE_CURVE ( 'NONE', #19471, #29398, #25940, .T. ) ;
#8082 = ORIENTED_EDGE ( 'NONE', *, *, #29543, .F. ) ;
#8083 = ORIENTED_EDGE ( 'NONE', *, *, #26013, .T. ) ;
#8084 = CARTESIAN_POINT ( 'NONE',  ( -19.70934530863873135, 3.501268498360765147, 6.755862304746362845 ) ) ;
#8085 = FACE_OUTER_BOUND ( 'NONE', #13921, .T. ) ;
#8086 = DIRECTION ( 'NONE',  ( 1.000000000000000000, 0.000000000000000000, 0.000000000000000000 ) ) ;
#8087 = ORIENTED_EDGE ( 'NONE', *, *, #25559, .T. ) ;
#8088 = CARTESIAN_POINT ( 'NONE',  ( -5.292460273040080487, 16.19569186415849060, 20.32222155561919053 ) ) ;
#8089 = EDGE_LOOP ( 'NONE', ( #11121, #17191, #27616, #29872 ) ) ;
#8090 = AXIS2_PLACEMENT_3D ( 'NONE', #1081, #2682, #20107 ) ;
#8091 = CARTESIAN_POINT ( 'NONE',  ( 39.52380524533145945, -7.028748154382054913, -11.49999999999999645 ) ) ;
#8092 = VERTEX_POINT ( 'NONE', #4572 ) ;
#8093 = DIRECTION ( 'NONE',  ( 0.000000000000000000, 0.000000000000000000, 1.000000000000000000 ) ) ;
#8094 = EDGE_CURVE ( 'NONE', #6549, #17738, #14223, .T. ) ;
#8095 = FACE_OUTER_BOUND ( 'NONE', #7747, .T. ) ;
#8096 = CARTESIAN_POINT ( 'NONE',  ( 16.63252861691852758, 3.817440173033142425, 7.441806358946449151 ) ) ;
#8097 = DIRECTION ( 'NONE',  ( 0.000000000000000000, 0.000000000000000000, -1.000000000000000000 ) ) ;
#8098 = EDGE_CURVE ( 'NONE', #1458, #20151, #25039, .T. ) ;
#8099 = CARTESIAN_POINT ( 'NONE',  ( -8.172867764805138435, -14.97344430594795739, 20.25542030744407640 ) ) ;
#8100 = CARTESIAN_POINT ( 'NONE',  ( -10.21480246439553063, 41.11241556754047366, 28.96073186326400872 ) ) ;
#8101 = CARTESIAN_POINT ( 'NONE',  ( 77.99999999999998579, -42.50000000000002132, 32.26246401786215756 ) ) ;
#8102 = FACE_OUTER_BOUND ( 'NONE', #4925, .T. ) ;
#8103 = ORIENTED_EDGE ( 'NONE', *, *, #25101, .T. ) ;
#8104 = CARTESIAN_POINT ( 'NONE',  ( 9.048061653868893828, -14.41834352799975960, 6.974106381145714018 ) ) ;
#8105 = CARTESIAN_POINT ( 'NONE',  ( -30.31362811597099238, 26.74039424657907205, 8.772790042427574875 ) ) ;
#8106 = DIRECTION ( 'NONE',  ( 0.000000000000000000, 0.000000000000000000, 1.000000000000000000 ) ) ;
#8107 = ORIENTED_EDGE ( 'NONE', *, *, #18151, .T. ) ;
#8108 = EDGE_LOOP ( 'NONE', ( #7934, #16655, #10093, #14633, #17796 ) ) ;
#8109 = DIRECTION ( 'NONE',  ( -0.000000000000000000, -1.000000000000000000, -0.000000000000000000 ) ) ;
#8110 = AXIS2_PLACEMENT_3D ( 'NONE', #5386, #12413, #10061 ) ;
#8111 = AXIS2_PLACEMENT_3D ( 'NONE', #5481, #14828, #17015 ) ;
#8112 = DIRECTION ( 'NONE',  ( 1.000000000000000000, 0.000000000000000000, 0.000000000000000000 ) ) ;
#8113 = CIRCLE ( 'NONE', #610, 0.7499999999999997780 ) ;
#8114 = CARTESIAN_POINT ( 'NONE',  ( -5.865338193562681823, 19.13956943172005865, 7.652108011868850035 ) ) ;
#8115 = VERTEX_POINT ( 'NONE', #5339 ) ;
#8116 = DIRECTION ( 'NONE',  ( 1.000000000000000000, 0.000000000000000000, 0.000000000000000000 ) ) ;
#8117 = DIRECTION ( 'NONE',  ( -0.000000000000000000, 1.000000000000000000, -0.000000000000000000 ) ) ;
#8118 = LINE ( 'NONE', #27141, #14902 ) ;
#8119 = B_SPLINE_CURVE_WITH_KNOTS ( 'NONE', 3,
 ( #15570, #28153, #6782, #10741, #13964, #20823, #23460, #17761, #8986, #23318, #2101, #18502, #11623, #18802 ),
 .UNSPECIFIED., .F., .F.,
 ( 4, 2, 2, 2, 2, 2, 4 ),
 ( 0.02129242833620984335, 0.02395618414067833199, 0.02661993994514682063, 0.03194745155408380138, 0.03461120735855229003, 0.03727496316302077867, 0.04260247477195776289 ),
 .UNSPECIFIED. ) ;
#8120 = ORIENTED_EDGE ( 'NONE', *, *, #1967, .T. ) ;
#8121 = CARTESIAN_POINT ( 'NONE',  ( -9.819201815016002755, -17.42389611976320296, 19.96797677718663522 ) ) ;
#8122 = DIRECTION ( 'NONE',  ( 0.000000000000000000, -0.000000000000000000, -1.000000000000000000 ) ) ;
#8123 = CARTESIAN_POINT ( 'NONE',  ( 16.83427080350348248, 2.570616772381430604, 5.862424720655265098 ) ) ;
#8124 = ORIENTED_EDGE ( 'NONE', *, *, #11225, .T. ) ;
#8125 = CARTESIAN_POINT ( 'NONE',  ( -65.00000000000000000, -70.00000000000000000, 12.49999999999999112 ) ) ;
#8126 = ORIENTED_EDGE ( 'NONE', *, *, #27842, .T. ) ;
#8127 = DIRECTION ( 'NONE',  ( -0.000000000000000000, -0.000000000000000000, -1.000000000000000000 ) ) ;
#8128 = CARTESIAN_POINT ( 'NONE',  ( -32.19782014694307293, 14.25394737442115733, 39.78814634291943975 ) ) ;
#8129 = VERTEX_POINT ( 'NONE', #12205 ) ;
#8130 = VECTOR ( 'NONE', #24535, 1000.000000000000000 ) ;
#8131 = CARTESIAN_POINT ( 'NONE',  ( 4.782940318440153327, 19.43789448792816543, 7.500147780736496017 ) ) ;
#8132 = AXIS2_PLACEMENT_3D ( 'NONE', #18275, #5805, #27799 ) ;
#8133 = DIRECTION ( 'NONE',  ( -1.000000000000000000, 0.000000000000000000, 0.000000000000000000 ) ) ;
#8134 = CARTESIAN_POINT ( 'NONE',  ( -50.00000000000000000, -50.00000000000000000, 12.49999999999998401 ) ) ;
#8135 = DIRECTION ( 'NONE',  ( -1.000000000000000000, 0.000000000000000000, 0.000000000000000000 ) ) ;
#8136 =( BOUNDED_CURVE ( )  B_SPLINE_CURVE ( 3, ( #21020, #18552, #28056, #30542 ),
 .UNSPECIFIED., .F., .T. ) 
 B_SPLINE_CURVE_WITH_KNOTS ( ( 4, 4 ),
 ( 0.4107522400370940407, 0.7424477459033789195 ),
 .UNSPECIFIED. ) 
 CURVE ( )  GEOMETRIC_REPRESENTATION_ITEM ( )  RATIONAL_B_SPLINE_CURVE ( ( 1.000000000000000000, 0.9908525036704132205, 0.9908525036704132205, 1.000000000000000000 ) ) 
 REPRESENTATION_ITEM ( '' )  );
#8137 = CARTESIAN_POINT ( 'NONE',  ( -15.85884089648730999, 35.55173462727350397, 27.50000000000000355 ) ) ;
#8138 = LINE ( 'NONE', #27163, #867 ) ;
#8139 = CARTESIAN_POINT ( 'NONE',  ( 10.68464666747176750, -16.90719797777717304, 18.47110296274026098 ) ) ;
#8140 = ORIENTED_EDGE ( 'NONE', *, *, #30686, .F. ) ;
#8142 = B_SPLINE_CURVE_WITH_KNOTS ( 'NONE', 3,
 ( #13165, #6289, #13488, #24868, #27663, #15802, #3505, #29692, #22506, #20634, #3802, #30152, #8339, #8781, #18308, #20336, #5679, #15175, #1150, #17853 ),
 .UNSPECIFIED., .F., .F.,
 ( 4, 2, 2, 2, 2, 2, 2, 2, 2, 4 ),
 ( 0.000000000000000000, 0.06250000000000044409, 0.1250000000000008882, 0.1875000000000013323, 0.2187500000000013600, 0.2500000000000013878, 0.3125000000000010547, 0.3750000000000007216, 0.4375000000000003886, 0.5000000000000000000 ),
 .UNSPECIFIED. ) ;
#8141 = CARTESIAN_POINT ( 'NONE',  ( 24.50428919468314959, 7.442132857256931189, 49.39104690844359880 ) ) ;
#8143 = CARTESIAN_POINT ( 'NONE',  ( -15.89252301733159989, 12.17122019226247431, 19.89182036555910571 ) ) ;
#8144 = CARTESIAN_POINT ( 'NONE',  ( 33.56327786402390245, 10.46063060613185414, 35.60191137445556819 ) ) ;
#8145 = CARTESIAN_POINT ( 'NONE',  ( -23.07950435457403415, 11.62838985844543060, 44.91415175113220215 ) ) ;
#8146 = ORIENTED_EDGE ( 'NONE', *, *, #28220, .F. ) ;
#8147 = CARTESIAN_POINT ( 'NONE',  ( 31.04966398092921409, -25.72093259340003968, 8.382396669768365172 ) ) ;
#8148 = DIRECTION ( 'NONE',  ( 1.000000000000000000, 0.000000000000000000, 4.565061778886335400E-17 ) ) ;
#8149 = B_SPLINE_SURFACE_WITH_KNOTS ( 'NONE', 3, 1, ( 
 ( #17907, #12756 ),
 ( #22565, #26808 ),
 ( #10718, #15391 ),
 ( #24447, #24915 ),
 ( #3395, #3088 ),
 ( #3712, #1060 ),
 ( #10248, #13225 ),
 ( #22713, #29133 ),
 ( #24595, #12923 ),
 ( #7768, #3552 ),
 ( #17275, #7935 ),
 ( #19762, #12609 ),
 ( #17441, #22259 ),
 ( #8084, #30056 ),
 ( #18517, #4475 ),
 ( #8847, #13834 ),
 ( #6798, #3860 ),
 ( #27883, #20980 ),
 ( #11033, #18662 ),
 ( #28168, #16323 ),
 ( #6504, #6352 ),
 ( #18207, #18054 ),
 ( #15700, #15865 ),
 ( #28018, #30365 ),
 ( #9146, #13384 ),
 ( #13687, #22875 ),
 ( #1824, #11346 ),
 ( #4303, #25681 ),
 ( #6197, #25841 ),
 ( #6651, #20681 ),
 ( #18372, #23018 ) ),
 .UNSPECIFIED., .F., .F., .F.,
 ( 4, 3, 3, 3, 3, 3, 3, 3, 3, 3, 4 ),
 ( 2, 2 ),
 ( 0.000000000000000000, 0.05425176834609633791, 0.1085332949128352958, 0.1623767749169382768, 0.2157504826133063158, 0.2688657508888171455, 0.3218907763505476360, 0.3749548578363336993, 0.4282048033836242107, 0.4818374082110501444, 0.4999999999131655715 ),
 ( 0.000000000000000000, 1.000000000000000000 ),
 .UNSPECIFIED. ) ;
#8150 = CARTESIAN_POINT ( 'NONE',  ( 12.76513901707091492, 11.27219777367672648, 7.453286057244485008 ) ) ;
#8151 = DIRECTION ( 'NONE',  ( 1.000000000000000000, 0.000000000000000000, 0.000000000000000000 ) ) ;
#8152 = VECTOR ( 'NONE', #17453, 1000.000000000000000 ) ;
#8153 = CARTESIAN_POINT ( 'NONE',  ( 6.974883619896790954, 5.687793815610376669, 1.500000000000001332 ) ) ;
#8154 = CYLINDRICAL_SURFACE ( 'NONE', #18864, 0.7500000000000007772 ) ;
#8155 = VECTOR ( 'NONE', #16223, 1000.000000000000000 ) ;
#8156 = CARTESIAN_POINT ( 'NONE',  ( 16.78403870108500584, 2.933703390053540527, 7.626437579292367097 ) ) ;
#8157 = AXIS2_PLACEMENT_3D ( 'NONE', #13139, #18582, #9367 ) ;
#8158 = ORIENTED_EDGE ( 'NONE', *, *, #7088, .T. ) ;
#8159 = CARTESIAN_POINT ( 'NONE',  ( 24.86084284002701850, 6.930828199065646622, 44.94877300773885764 ) ) ;
#8160 = DIRECTION ( 'NONE',  ( 0.000000000000000000, 0.000000000000000000, 1.000000000000000000 ) ) ;
#8161 = CARTESIAN_POINT ( 'NONE',  ( 47.00000000000044764, -4.926614671774132148E-13, 82.49999999999998579 ) ) ;
#8162 = VERTEX_POINT ( 'NONE', #24364 ) ;
#8163 = ORIENTED_EDGE ( 'NONE', *, *, #16475, .T. ) ;
#8164 = CARTESIAN_POINT ( 'NONE',  ( -8.499586724479453181, -2.959227181723774525, 1.500000000000001332 ) ) ;
#8165 = VERTEX_POINT ( 'NONE', #29201 ) ;
#8166 = CARTESIAN_POINT ( 'NONE',  ( -50.00000000000000000, -50.00000000000000000, 62.49999999999999289 ) ) ;
#8167 = CARTESIAN_POINT ( 'NONE',  ( -15.34618031767422863, 12.82553819247483951, 5.652196082369963293 ) ) ;
#8168 = DIRECTION ( 'NONE',  ( 1.000000000000000000, 0.000000000000000000, 0.000000000000000000 ) ) ;
#8169 = CARTESIAN_POINT ( 'NONE',  ( -35.29666319828150023, 18.12171425783904866, 8.528199801003413683 ) ) ;
#8170 = DIRECTION ( 'NONE',  ( 0.000000000000000000, 0.000000000000000000, 1.000000000000000000 ) ) ;
#8171 = DIRECTION ( 'NONE',  ( -0.5503133621338236470, -0.8349582046168341209, 0.000000000000000000 ) ) ;
#8172 = CARTESIAN_POINT ( 'NONE',  ( -37.99999999999999289, 209.2686044187655909, -40.50000000000000000 ) ) ;
#8173 = CARTESIAN_POINT ( 'NONE',  ( 3.474270935886293543, -15.38174572367601911, 1.500000000000001332 ) ) ;
#8174 = CARTESIAN_POINT ( 'NONE',  ( -2.810445847081922022, -9.056208293496300854, 1.500000000000001332 ) ) ;
#8175 = ORIENTED_EDGE ( 'NONE', *, *, #11480, .T. ) ;
#8176 = VECTOR ( 'NONE', #30316, 1000.000000000000000 ) ;
#8177 = VECTOR ( 'NONE', #22002, 1000.000000000000000 ) ;
#8178 = PLANE ( 'NONE',  #30708 ) ;
#8179 = CARTESIAN_POINT ( 'NONE',  ( -5.973959739936658409, 19.10558604466630328, 7.652108011868850035 ) ) ;
#8180 = CARTESIAN_POINT ( 'NONE',  ( 10.39243974596413445, -13.53611166824776646, 5.872146474157316831 ) ) ;
#8181 = CARTESIAN_POINT ( 'NONE',  ( 39.83602371821015709, 11.57901747687536265, -19.50000000000000355 ) ) ;
#8182 = DIRECTION ( 'NONE',  ( 0.000000000000000000, -1.000000000000000000, 0.000000000000000000 ) ) ;
#8183 = ORIENTED_EDGE ( 'NONE', *, *, #10090, .F. ) ;
#8184 = ORIENTED_EDGE ( 'NONE', *, *, #21177, .T. ) ;
#8185 = DIRECTION ( 'NONE',  ( 0.000000000000000000, 0.000000000000000000, 1.000000000000000000 ) ) ;
#8186 = CARTESIAN_POINT ( 'NONE',  ( 39.00000000000000000, -5.563236990218592304, -1.500000000000000000 ) ) ;
#8187 = CARTESIAN_POINT ( 'NONE',  ( -13.09601454503479268, 10.89247868135537267, 5.749228751562096562 ) ) ;
#8188 = CARTESIAN_POINT ( 'NONE',  ( 2.703030265324084080, -12.75514121382991384, 1.500000000000001332 ) ) ;
#8189 = ORIENTED_EDGE ( 'NONE', *, *, #30, .T. ) ;
#8190 = ITEM_DEFINED_TRANSFORMATION ( 'NONE', 'NONE', #13397,  #7396 ) ;
#8191 = CARTESIAN_POINT ( 'NONE',  ( 15.81223572262636878, -6.365019322297388094, 20.34789198813115263 ) ) ;
#8192 = CARTESIAN_POINT ( 'NONE',  ( 0.000000000000000000, 44.39187623478217404, -19.50000000000000355 ) ) ;
#8193 = ORIENTED_EDGE ( 'NONE', *, *, #578, .T. ) ;
#8194 = DIRECTION ( 'NONE',  ( -0.000000000000000000, 1.132880637372608986E-16, -1.000000000000000000 ) ) ;
#8195 = CARTESIAN_POINT ( 'NONE',  ( -35.00000000000000000, 70.00000000000000000, -22.50000000000003908 ) ) ;
#8196 = CARTESIAN_POINT ( 'NONE',  ( -36.72813896306210069, -7.597066778515316088, 37.50000000000667200 ) ) ;
#8197 = EDGE_CURVE ( 'NONE', #12669, #19397, #9100, .T. ) ;
#8198 = ORIENTED_EDGE ( 'NONE', *, *, #16853, .T. ) ;
#8199 = CARTESIAN_POINT ( 'NONE',  ( 11.22181534970138905, -16.55562029408563163, 5.652912763329821288 ) ) ;
#8200 = FACE_OUTER_BOUND ( 'NONE', #9264, .T. ) ;
#8201 = FACE_OUTER_BOUND ( 'NONE', #535, .T. ) ;
#8202 = CARTESIAN_POINT ( 'NONE',  ( -1.246245039005656974, 2.728895986063601509, 24.50000000000000000 ) ) ;
#8203 = EDGE_CURVE ( 'NONE', #25490, #11996, #29024, .T. ) ;
#8204 = ORIENTED_EDGE ( 'NONE', *, *, #13955, .F. ) ;
#8205 = APPLICATION_CONTEXT ( 'automotive_design' ) ;
#8206 = CARTESIAN_POINT ( 'NONE',  ( -1.246245039005721811, -2.728895986063572643, 24.50000000000000000 ) ) ;
#8207 = DIRECTION ( 'NONE',  ( -0.000000000000000000, -0.000000000000000000, -1.000000000000000000 ) ) ;
#8208 = EDGE_CURVE ( 'NONE', #22536, #6221, #6569, .T. ) ;
#8209 = CARTESIAN_POINT ( 'NONE',  ( 1.530808498934191521E-15, -12.50000000000000000, -87.50000000000000000 ) ) ;
#8210 = CARTESIAN_POINT ( 'NONE',  ( -40.22764886168826592, -5.870704729722422854, -16.50000000000000000 ) ) ;
#8211 = DIRECTION ( 'NONE',  ( -0.8349582046168341209, 0.5503133621338236470, 0.000000000000000000 ) ) ;
#8212 = AXIS2_PLACEMENT_3D ( 'NONE', #8660, #29557, #24881 ) ;
#8213 = DIRECTION ( 'NONE',  ( 1.000000000000000000, 0.000000000000000000, 0.000000000000000000 ) ) ;
#8214 = DIRECTION ( 'NONE',  ( 0.000000000000000000, 0.000000000000000000, 1.000000000000000000 ) ) ;
#8215 = ORIENTED_EDGE ( 'NONE', *, *, #25909, .T. ) ;
#8216 = CARTESIAN_POINT ( 'NONE',  ( 7.974144905643786529, 5.130938270761634890, 21.50000000000000000 ) ) ;
#8217 = CARTESIAN_POINT ( 'NONE',  ( 4.512576344050363453, 19.48449473338812510, 7.272192800924343281 ) ) ;
#8218 = EDGE_CURVE ( 'NONE', #15437, #2838, #3009, .T. ) ;
#8219 = ORIENTED_EDGE ( 'NONE', *, *, #907, .F. ) ;
#8220 = ORIENTED_EDGE ( 'NONE', *, *, #26378, .F. ) ;
#8221 = EDGE_CURVE ( 'NONE', #19990, #26044, #29050, .T. ) ;
#8222 = DIRECTION ( 'NONE',  ( 1.000000000000000000, 0.000000000000000000, -0.000000000000000000 ) ) ;
#8223 = CARTESIAN_POINT ( 'NONE',  ( -32.74775157610760346, -27.21557300919352329, -19.50000000000000355 ) ) ;
#8224 = CARTESIAN_POINT ( 'NONE',  ( -6.207687030005119233, 49.61523691829047067, -68.66397725790081097 ) ) ;
#8225 = ORIENTED_EDGE ( 'NONE', *, *, #24838, .T. ) ;
#8226 = CARTESIAN_POINT ( 'NONE',  ( -5.549075634136965363, 16.11684027513961226, 18.34798005863078885 ) ) ;
#8227 = CARTESIAN_POINT ( 'NONE',  ( 12.82328378257164303, 11.20259424400690840, 18.63641924841378028 ) ) ;
#8228 = ORIENTED_EDGE ( 'NONE', *, *, #12895, .F. ) ;
#8229 = VERTEX_POINT ( 'NONE', #26710 ) ;
#8230 = LINE ( 'NONE', #24750, #9804 ) ;
#8231 = CARTESIAN_POINT ( 'NONE',  ( 19.70572240696341382, 3.522277800415037685, 20.29915277494337644 ) ) ;
#8232 = DIRECTION ( 'NONE',  ( 0.000000000000000000, 1.000000000000000000, -0.000000000000000000 ) ) ;
#8233 = ORIENTED_EDGE ( 'NONE', *, *, #450, .F. ) ;
#8234 = CARTESIAN_POINT ( 'NONE',  ( -5.296822449995211457, 16.19439135686744180, 18.37259980046033547 ) ) ;
#8235 = AXIS2_PLACEMENT_3D ( 'NONE', #12843, #4087, #2194 ) ;
#8236 = ADVANCED_FACE ( 'NONE', ( #506 ), #7838, .F. ) ;
#8237 = EDGE_LOOP ( 'NONE', ( #25594, #307 ) ) ;
#8238 = ADVANCED_FACE ( 'NONE', ( #26563 ), #26878, .T. ) ;
#8239 = CARTESIAN_POINT ( 'NONE',  ( 43.34097750826427387, 11.89502811014146033, 1.500000000000000000 ) ) ;
#8240 = VERTEX_POINT ( 'NONE', #24514 ) ;
#8241 = EDGE_CURVE ( 'NONE', #9598, #9741, #657, .T. ) ;
#8242 = DIRECTION ( 'NONE',  ( -0.000000000000000000, -0.000000000000000000, -1.000000000000000000 ) ) ;
#8243 = EDGE_CURVE ( 'NONE', #3557, #28757, #19639, .T. ) ;
#8244 = DIRECTION ( 'NONE',  ( 0.000000000000000000, -1.132880637372608986E-16, 1.000000000000000000 ) ) ;
#8245 = CARTESIAN_POINT ( 'NONE',  ( 16.57326105224178647, 4.109591991357616436, 6.233981582756856987 ) ) ;
#8246 = CARTESIAN_POINT ( 'NONE',  ( -14.88989150774293790, 13.37932992012220623, 18.63641924841378028 ) ) ;
#8247 = CARTESIAN_POINT ( 'NONE',  ( -4.163336342344337027E-14, 1.387778780781445676E-14, 34.49999999999999289 ) ) ;
#8248 = EDGE_CURVE ( 'NONE', #10258, #30397, #7483, .T. ) ;
#8249 = CARTESIAN_POINT ( 'NONE',  ( -33.30753377797442027, -22.11854778782412367, 30.86655168617016187 ) ) ;
#8250 = CARTESIAN_POINT ( 'NONE',  ( -10.47960520055065636, -7.757439966934454034, 24.50000000000000000 ) ) ;
#8251 = FACE_OUTER_BOUND ( 'NONE', #1674, .T. ) ;
#8252 = ORIENTED_EDGE ( 'NONE', *, *, #14683, .F. ) ;
#8253 = EDGE_CURVE ( 'NONE', #29075, #9580, #2174, .T. ) ;
#8254 = DIRECTION ( 'NONE',  ( 0.7557495743542581579, 0.6548607339452852116, 0.000000000000000000 ) ) ;
#8255 = CARTESIAN_POINT ( 'NONE',  ( 9.991354877675737711, -13.81564317159775257, 18.35718225375110180 ) ) ;
#8256 = DIRECTION ( 'NONE',  ( -0.000000000000000000, -0.000000000000000000, -1.000000000000000000 ) ) ;
#8257 = VERTEX_POINT ( 'NONE', #16835 ) ;
#8258 = VERTEX_POINT ( 'NONE', #289 ) ;
#8260 = EDGE_CURVE ( 'NONE', #7465, #24236, #12002, .T. ) ;
#8259 = CIRCLE ( 'NONE', #25687, 1.447898107987198646 ) ;
#8261 = CARTESIAN_POINT ( 'NONE',  ( 17.96688762764192759, -8.785985129476815203, 18.84056766331480404 ) ) ;
#8262 = CARTESIAN_POINT ( 'NONE',  ( 3.196529495465388226, 8.413215745755008967, -1.500000000000000888 ) ) ;
#8263 = CARTESIAN_POINT ( 'NONE',  ( -5.025762778208111570, 19.37674427759095508, 6.864725433338323413 ) ) ;
#8264 = EDGE_LOOP ( 'NONE', ( #10443, #30740, #10239, #21563 ) ) ;
#8265 = DIRECTION ( 'NONE',  ( 0.000000000000000000, 0.000000000000000000, -1.000000000000000000 ) ) ;
#8266 = CARTESIAN_POINT ( 'NONE',  ( 49.99999999999998579, 70.00000000000000000, -92.50000000000000000 ) ) ;
#8267 = CARTESIAN_POINT ( 'NONE',  ( -4.622016212553093695, -12.19167610014704906, 1.500000000000001332 ) ) ;
#8268 = ORIENTED_EDGE ( 'NONE', *, *, #4112, .T. ) ;
#8269 = DIRECTION ( 'NONE',  ( 0.000000000000000000, 0.000000000000000000, -1.000000000000000000 ) ) ;
#8270 = MECHANICAL_DESIGN_GEOMETRIC_PRESENTATION_REPRESENTATION (  '', ( #27682 ), #21193 ) ;
#8271 = CYLINDRICAL_SURFACE ( 'NONE', #2274, 0.7500000000000006661 ) ;
#8272 = CARTESIAN_POINT ( 'NONE',  ( 16.86926274317445618, 2.283828795636142495, 7.080843742048788414 ) ) ;
#8273 = ORIENTED_EDGE ( 'NONE', *, *, #4791, .F. ) ;
#8274 = CARTESIAN_POINT ( 'NONE',  ( 12.50580948684386406, 11.57370347876661576, 5.670038381137163519 ) ) ;
#8275 = EDGE_CURVE ( 'NONE', #8512, #8763, #28985, .T. ) ;
#8276 = ORIENTED_EDGE ( 'NONE', *, *, #30149, .F. ) ;
#8277 = DIRECTION ( 'NONE',  ( 0.000000000000000000, 1.000000000000000000, -0.000000000000000000 ) ) ;
#8278 = ADVANCED_FACE ( 'NONE', ( #28688 ), #28848, .F. ) ;
#8279 = CARTESIAN_POINT ( 'NONE',  ( 32.06827542805550024, -14.53851282002520229, 35.54771035678264468 ) ) ;
#8280 = ORIENTED_EDGE ( 'NONE', *, *, #10532, .F. ) ;
#8281 = EDGE_CURVE ( 'NONE', #1147, #22188, #22493, .T. ) ;
#8282 = ORIENTED_EDGE ( 'NONE', *, *, #8253, .F. ) ;
#8283 = CIRCLE ( 'NONE', #1308, 7.500000000000000000 ) ;
#8284 = CARTESIAN_POINT ( 'NONE',  ( 4.339153914952783353, 19.54170514621186783, 6.892848776733236704 ) ) ;
#8285 = CARTESIAN_POINT ( 'NONE',  ( 32.44940373544195467, 8.539989232413363496, 41.44564370983190571 ) ) ;
#8286 = CARTESIAN_POINT ( 'NONE',  ( 37.99999999999999289, 80.00000000000000000, 0.000000000000000000 ) ) ;
#8287 = AXIS2_PLACEMENT_3D ( 'NONE', #14814, #16857, #19348 ) ;
#8288 = CARTESIAN_POINT ( 'NONE',  ( -21.86019681245148405, 31.48592878035298170, 34.80090346875805807 ) ) ;
#8289 = CARTESIAN_POINT ( 'NONE',  ( 9.669732009941350626, -14.02977311367122937, 20.32842677360128292 ) ) ;
#8290 = CARTESIAN_POINT ( 'NONE',  ( 16.74328840634221649, 3.194145055459935101, 20.34789198813115263 ) ) ;
#8291 = ORIENTED_EDGE ( 'NONE', *, *, #19493, .F. ) ;
#8292 = DIRECTION ( 'NONE',  ( -1.000000000000000000, 0.000000000000000000, 0.000000000000000000 ) ) ;
#8293 = CARTESIAN_POINT ( 'NONE',  ( 18.05613910678267331, -8.642405844459421616, 5.940635272151477686 ) ) ;
#8294 = CARTESIAN_POINT ( 'NONE',  ( -15.40675500887359384, 12.78077869785448151, 18.34838970509067479 ) ) ;
#8295 = AXIS2_PLACEMENT_3D ( 'NONE', #7135, #6814, #16341 ) ;
#8296 = DIRECTION ( 'NONE',  ( -1.000000000000000000, 0.000000000000000000, 0.000000000000000000 ) ) ;
#8297 = LINE ( 'NONE', #27327, #28840 ) ;
#8298 = ORIENTED_EDGE ( 'NONE', *, *, #7473, .T. ) ;
#8299 = DIRECTION ( 'NONE',  ( -0.000000000000000000, -0.000000000000000000, -1.000000000000000000 ) ) ;
#8300 = AXIS2_PLACEMENT_3D ( 'NONE', #17504, #27174, #5803 ) ;
#8301 = DIRECTION ( 'NONE',  ( -0.000000000000000000, -0.000000000000000000, 1.000000000000000000 ) ) ;
#8302 = CARTESIAN_POINT ( 'NONE',  ( -5.548724899233042684, 19.23375410423648191, 20.25336174263950184 ) ) ;
#8303 = DIRECTION ( 'NONE',  ( -1.000000000000000000, 0.000000000000000000, 0.000000000000000000 ) ) ;
#8304 = DIRECTION ( 'NONE',  ( 0.000000000000000000, 0.000000000000000000, -1.000000000000000000 ) ) ;
#8305 = PLANE ( 'NONE',  #941 ) ;
#8306 = VECTOR ( 'NONE', #15013, 1000.000000000000000 ) ;
#8307 = CARTESIAN_POINT ( 'NONE',  ( 18.08806846220652531, 37.65969142884505771, 29.27956356433786311 ) ) ;
#8308 = EDGE_CURVE ( 'NONE', #8162, #17860, #18871, .T. ) ;
#8309 = VERTEX_POINT ( 'NONE', #26498 ) ;
#8310 = VECTOR ( 'NONE', #1192, 1000.000000000000000 ) ;
#8311 = EDGE_CURVE ( 'NONE', #19687, #30853, #8563, .T. ) ;
#8312 = CARTESIAN_POINT ( 'NONE',  ( 24.75988009833579540, 7.043597625963923470, 45.01551998635105889 ) ) ;
#8313 = ORIENTED_EDGE ( 'NONE', *, *, #5986, .T. ) ;
#8314 = CARTESIAN_POINT ( 'NONE',  ( -32.94612346989018192, 8.892333671926630601, 40.87496192031042597 ) ) ;
#8315 = ORIENTED_EDGE ( 'NONE', *, *, #24835, .T. ) ;
#8316 = ORIENTED_EDGE ( 'NONE', *, *, #19851, .T. ) ;
#8317 = CARTESIAN_POINT ( 'NONE',  ( -9.131494062835630032, -2.555255504830938218, 1.500000000000001332 ) ) ;
#8318 = CARTESIAN_POINT ( 'NONE',  ( -19.93457197822651850, 1.617270501065022126, 19.85730954408917981 ) ) ;
#8319 = VECTOR ( 'NONE', #24229, 1000.000000000000000 ) ;
#8320 =( BOUNDED_CURVE ( )  B_SPLINE_CURVE ( 3, ( #17845, #29687, #27362, #10354 ),
 .UNSPECIFIED., .F., .T. ) 
 B_SPLINE_CURVE_WITH_KNOTS ( ( 4, 4 ),
 ( 3.552344893626886879, 3.884040399493172036 ),
 .UNSPECIFIED. ) 
 CURVE ( )  GEOMETRIC_REPRESENTATION_ITEM ( )  RATIONAL_B_SPLINE_CURVE ( ( 1.000000000000000000, 0.9908525036704132205, 0.9908525036704132205, 1.000000000000000000 ) ) 
 REPRESENTATION_ITEM ( '' )  );
#8321 = ORIENTED_EDGE ( 'NONE', *, *, #578, .F. ) ;
#8322 = LINE ( 'NONE', #14863, #21325 ) ;
#8323 = CIRCLE ( 'NONE', #3777, 29.99999999999928946 ) ;
#8324 = DIRECTION ( 'NONE',  ( 1.982541115402065110E-16, 0.000000000000000000, -1.000000000000000000 ) ) ;
#8325 = CARTESIAN_POINT ( 'NONE',  ( -37.99999999999999289, 90.00000000000001421, -22.50000000000000711 ) ) ;
#8326 = DIRECTION ( 'NONE',  ( 0.000000000000000000, 0.000000000000000000, 1.000000000000000000 ) ) ;
#8327 = VECTOR ( 'NONE', #27068, 1000.000000000000000 ) ;
#8328 = DIRECTION ( 'NONE',  ( 0.000000000000000000, 0.000000000000000000, -1.000000000000000000 ) ) ;
#8329 = VECTOR ( 'NONE', #29722, 1000.000000000000000 ) ;
#8330 = CARTESIAN_POINT ( 'NONE',  ( 32.98805937973593672, -80.00000000000000000, 13.00000000000000178 ) ) ;
#8331 = LINE ( 'NONE', #29227, #10616 ) ;
#8332 = CARTESIAN_POINT ( 'NONE',  ( 0.6919288935074161540, -20.00608154967866881, 5.704143890883081269 ) ) ;
#8333 = DIRECTION ( 'NONE',  ( -0.000000000000000000, -0.000000000000000000, -1.000000000000000000 ) ) ;
#8334 = ORIENTED_EDGE ( 'NONE', *, *, #15462, .T. ) ;
#8335 = AXIS2_PLACEMENT_3D ( 'NONE', #22466, #1114, #5173 ) ;
#8336 = AXIS2_PLACEMENT_3D ( 'NONE', #20593, #30118, #23394 ) ;
#8337 = CARTESIAN_POINT ( 'NONE',  ( -10.81179434590808697, -16.84691785479785864, 20.29090034784956131 ) ) ;
#8338 = CARTESIAN_POINT ( 'NONE',  ( -14.75084321123812003, -8.599826344683139112, 7.098451512883313441 ) ) ;
#8339 = CARTESIAN_POINT ( 'NONE',  ( -4.600690885565751564, 16.38836304891476914, 6.385774490351136201 ) ) ;
#8340 = CARTESIAN_POINT ( 'NONE',  ( 11.94785300146925522, -16.06093515404948135, 6.560937769032974209 ) ) ;
#8341 = CARTESIAN_POINT ( 'NONE',  ( 40.89187623478217404, -5.790488632116400858, -19.50000000000000355 ) ) ;
#8342 = CARTESIAN_POINT ( 'NONE',  ( 16.69721919944051791, -13.88429941593332551, -1.500000000000000000 ) ) ;
#8343 = ORIENTED_EDGE ( 'NONE', *, *, #22945, .T. ) ;
#8344 = ORIENTED_EDGE ( 'NONE', *, *, #15087, .T. ) ;
#8345 = CARTESIAN_POINT ( 'NONE',  ( 0.000000000000000000, 65.00000000000000000, 50.49999999999998579 ) ) ;
#8346 = CARTESIAN_POINT ( 'NONE',  ( -10.64374042650075403, -42.96126232887726815, -19.50000000000000355 ) ) ;
#8347 = CARTESIAN_POINT ( 'NONE',  ( -2.296078483958558625, -42.45314922741754771, 34.61196682005081726 ) ) ;
#8348 = DIRECTION ( 'NONE',  ( -0.000000000000000000, -0.000000000000000000, 1.000000000000000000 ) ) ;
#8349 = ORIENTED_EDGE ( 'NONE', *, *, #26558, .T. ) ;
#8350 = CARTESIAN_POINT ( 'NONE',  ( 3.094187858404264357, 16.79444423853821533, 6.392658652357121163 ) ) ;
#8351 = VECTOR ( 'NONE', #23518, 1000.000000000000000 ) ;
#8352 = CARTESIAN_POINT ( 'NONE',  ( 10.11202017158399968, 41.14070756921128691, -1.500000000000000000 ) ) ;
#8353 = CARTESIAN_POINT ( 'NONE',  ( -11.36561296172221169, -16.47845303048202936, 6.530762810602277924 ) ) ;
#8354 = AXIS2_PLACEMENT_3D ( 'NONE', #24568, #22073, #29570 ) ;
#8355 = ORIENTED_EDGE ( 'NONE', *, *, #6161, .T. ) ;
#8356 = B_SPLINE_CURVE_WITH_KNOTS ( 'NONE', 3,
 ( #4385, #1605, #2195, #27644, #6268, #18591 ),
 .UNSPECIFIED., .F., .F.,
 ( 4, 2, 4 ),
 ( 1.408367944307647113, 1.570796326794821507, 1.733224709277370712 ),
 .UNSPECIFIED. ) ;
#8357 = CIRCLE ( 'NONE', #19297, 21.71568325578193637 ) ;
#8358 = CARTESIAN_POINT ( 'NONE',  ( -5.687793815610304726, 6.974883619896852238, -3.621320343559650379 ) ) ;
#8359 = CARTESIAN_POINT ( 'NONE',  ( 19.56075217167569846, 4.168887357664726068, 19.08830981656264214 ) ) ;
#8360 = ORIENTED_EDGE ( 'NONE', *, *, #25196, .F. ) ;
#8361 = CARTESIAN_POINT ( 'NONE',  ( 11.91611018267553490, -16.06265986513585275, 6.919864475265772974 ) ) ;
#8362 = AXIS2_PLACEMENT_3D ( 'NONE', #1717, #29818, #8460 ) ;
#8363 = CARTESIAN_POINT ( 'NONE',  ( 32.19782014694308003, -14.25394737442115201, 39.78814634291934738 ) ) ;
#8364 = FACE_OUTER_BOUND ( 'NONE', #20785, .T. ) ;
#8365 = CIRCLE ( 'NONE', #3365, 20.32284676574536064 ) ;
#8366 = ORIENTED_EDGE ( 'NONE', *, *, #28881, .T. ) ;
#8367 = LINE ( 'NONE', #27398, #19290 ) ;
#8368 = CARTESIAN_POINT ( 'NONE',  ( 17.75446986341059841, 9.207540381081344094, 24.50000000000000000 ) ) ;
#8369 = CARTESIAN_POINT ( 'NONE',  ( -30.31220697679117393, 11.23460505553742550, 1.500000000000000000 ) ) ;
#8370 = DIRECTION ( 'NONE',  ( 1.000000000000000000, 0.000000000000000000, 0.000000000000000000 ) ) ;
#8371 = VECTOR ( 'NONE', #22422, 1000.000000000000000 ) ;
#8372 = DIRECTION ( 'NONE',  ( 1.000000000000000000, 0.000000000000000000, 0.000000000000000000 ) ) ;
#8373 = CIRCLE ( 'NONE', #25801, 9.084132297865673777 ) ;
#8374 = FACE_OUTER_BOUND ( 'NONE', #8653, .T. ) ;
#8375 = DIRECTION ( 'NONE',  ( -0.000000000000000000, 0.000000000000000000, -1.000000000000000000 ) ) ;
#8376 = CYLINDRICAL_SURFACE ( 'NONE', #27845, 1.000000000000011324 ) ;
#8377 = ORIENTED_EDGE ( 'NONE', *, *, #24212, .F. ) ;
#8378 = CARTESIAN_POINT ( 'NONE',  ( 0.000000000000000000, 87.00000000000001421, 12.49999999999999112 ) ) ;
#8379 = CARTESIAN_POINT ( 'NONE',  ( -9.288552932812276453, -14.26664216879104430, 18.83976166372255534 ) ) ;
#8380 = VERTEX_POINT ( 'NONE', #21654 ) ;
#8381 = EDGE_LOOP ( 'NONE', ( #16352, #19369, #22133, #11079 ) ) ;
#8382 = FACE_BOUND ( 'NONE', #26017, .T. ) ;
#8383 = CARTESIAN_POINT ( 'NONE',  ( 20.65888525914559892, 38.75220717792412728, -19.50000000000000355 ) ) ;
#8384 = VECTOR ( 'NONE', #758, 1000.000000000000000 ) ;
#8385 = PLANE ( 'NONE',  #12399 ) ;
#8386 = ORIENTED_EDGE ( 'NONE', *, *, #450, .T. ) ;
#8387 = AXIS2_PLACEMENT_3D ( 'NONE', #8779, #6598, #8950 ) ;
#8388 = ADVANCED_BREP_SHAPE_REPRESENTATION ( '', ( #2654, #7396 ), #14351 ) ;
#8389 = DIRECTION ( 'NONE',  ( 0.000000000000000000, 0.000000000000000000, 1.000000000000000000 ) ) ;
#8390 = AXIS2_PLACEMENT_3D ( 'NONE', #6248, #23069, #17961 ) ;
#8391 = DIRECTION ( 'NONE',  ( 1.000000000000000000, 0.000000000000000000, 0.000000000000000000 ) ) ;
#8392 = VERTEX_POINT ( 'NONE', #9502 ) ;
#8393 = ORIENTED_EDGE ( 'NONE', *, *, #14265, .F. ) ;
#8394 = EDGE_CURVE ( 'NONE', #20108, #19511, #30426, .T. ) ;
#8395 = CARTESIAN_POINT ( 'NONE',  ( -22.50000000000000711, 1.020384741037239916E-14, 52.50000000000000000 ) ) ;
#8396 = LINE ( 'NONE', #5586, #20726 ) ;
#8397 = CIRCLE ( 'NONE', #6882, 0.7441270634456903510 ) ;
#8398 = CARTESIAN_POINT ( 'NONE',  ( 14.96983285839275268, 13.26353275515934982, 7.652108011868850035 ) ) ;
#8399 = CARTESIAN_POINT ( 'NONE',  ( -5.078594737417330585, 37.17323350146568828, 37.50000000004207834 ) ) ;
#8400 = VERTEX_POINT ( 'NONE', #4977 ) ;
#8401 = PLANE ( 'NONE',  #5377 ) ;
#8402 = ORIENTED_EDGE ( 'NONE', *, *, #25241, .T. ) ;
#8403 = CARTESIAN_POINT ( 'NONE',  ( 24.44496207165490276, 7.595930209050162141, 45.15942333309104129 ) ) ;
#8404 = ORIENTED_EDGE ( 'NONE', *, *, #18029, .F. ) ;
#8405 = CARTESIAN_POINT ( 'NONE',  ( -6.096671963363472280, 19.04856480014127840, 20.34789198813115618 ) ) ;
#8406 = CARTESIAN_POINT ( 'NONE',  ( 3.763133143576435913, -8.268028093133381162, 21.50000000000000000 ) ) ;
#8407 = B_SPLINE_SURFACE_WITH_KNOTS ( 'NONE', 3, 1, ( 
 ( #20125, #29956 ),
 ( #29805, #17482 ),
 ( #13271, #27004 ),
 ( #15272, #5632 ),
 ( #24803, #29643 ),
 ( #15127, #8448 ),
 ( #24643, #3277 ),
 ( #17791, #12806 ),
 ( #947, #10459 ),
 ( #19973, #29492 ),
 ( #3440, #12961 ) ),
 .UNSPECIFIED., .F., .F., .F.,
 ( 4, 1, 1, 1, 1, 1, 1, 1, 4 ),
 ( 2, 2 ),
 ( 3.141592653589793116, 3.534291735288517255, 3.926990816987241395, 4.319689898685965090, 4.712388980384689674, 5.105088062083414258, 5.497787143782137953, 5.890486225480861648, 6.283185307179586232 ),
 ( 0.000000000000000000, 1.000000000000000000 ),
 .UNSPECIFIED. ) ;
#8408 = CARTESIAN_POINT ( 'NONE',  ( 19.59127448685153539, 4.109591991357616436, 6.233981582756856987 ) ) ;
#8409 = DIRECTION ( 'NONE',  ( 0.000000000000000000, 0.000000000000000000, -1.000000000000000000 ) ) ;
#8410 = VECTOR ( 'NONE', #8023, 1000.000000000000000 ) ;
#8411 = CIRCLE ( 'NONE', #23332, 9.084132297865673777 ) ;
#8412 = AXIS2_PLACEMENT_3D ( 'NONE', #17903, #8842, #18366 ) ;
#8413 = CARTESIAN_POINT ( 'NONE',  ( 0.000000000000000000, 0.000000000000000000, -11.49999999999999645 ) ) ;
#8414 = CARTESIAN_POINT ( 'NONE',  ( -1.438332125858111432, 8.884323311075791096, -1.500000000000000888 ) ) ;
#8415 = CARTESIAN_POINT ( 'NONE',  ( -19.93913687200723572, 1.772791844786497872, 18.64703902303423178 ) ) ;
#8416 = LINE ( 'NONE', #13556, #9866 ) ;
#8417 = VERTEX_POINT ( 'NONE', #9350 ) ;
#8418 = PLANE ( 'NONE',  #16776 ) ;
#8419 = CARTESIAN_POINT ( 'NONE',  ( 11.48757468322166986, -16.39371511241313328, 18.44527579819791185 ) ) ;
#8420 = CIRCLE ( 'NONE', #22388, 0.7500000000000006661 ) ;
#8421 = CARTESIAN_POINT ( 'NONE',  ( 31.18890335284659443, -19.89223002944918761, 34.80090346875810781 ) ) ;
#8422 = ORIENTED_EDGE ( 'NONE', *, *, #20630, .F. ) ;
#8423 = ORIENTED_EDGE ( 'NONE', *, *, #13745, .T. ) ;
#8424 = CARTESIAN_POINT ( 'NONE',  ( 44.20394856031893482, 69.15214064669606842, 13.40394286660155210 ) ) ;
#8425 = EDGE_CURVE ( 'NONE', #8747, #29572, #20995, .T. ) ;
#8426 = CARTESIAN_POINT ( 'NONE',  ( 11.11118051879627799, -16.62953239715189824, 5.652196082369963293 ) ) ;
#8427 = EDGE_CURVE ( 'NONE', #4181, #18831, #29711, .T. ) ;
#8428 = B_SPLINE_CURVE_WITH_KNOTS ( 'NONE', 3,
 ( #30501, #23479, #27571, #10881, #20392, #1975, #29914, #30207, #8551, #25216, #11185, #1525, #27720, #25381, #13537, #20535, #4011, #16014 ),
 .UNSPECIFIED., .F., .F.,
 ( 4, 2, 2, 2, 2, 2, 2, 2, 4 ),
 ( 0.003174295595554272285, 0.003570702171545501145, 0.003967108747536730005, 0.004363515323527957998, 0.004759921899519186858, 0.005156328475510415718, 0.005552735051501644578, 0.005949141627492873438, 0.006345548203484102298 ),
 .UNSPECIFIED. ) ;
#8429 = CARTESIAN_POINT ( 'NONE',  ( -4.573183673931451310, 16.39543396787673402, 6.755862304746362845 ) ) ;
#8430 = VERTEX_POINT ( 'NONE', #3413 ) ;
#8431 = DIRECTION ( 'NONE',  ( 0.000000000000000000, 0.000000000000000000, 1.000000000000000000 ) ) ;
#8432 = CARTESIAN_POINT ( 'NONE',  ( 5.141690706682880752, -7.488956955540417404, 13.22130136205108819 ) ) ;
#8433 = B_SPLINE_CURVE_WITH_KNOTS ( 'NONE', 3,
 ( #16556, #24031, #19203, #2677, #26073, #23886, #9856, #28572, #7524, #13922, #16411, #9398, #21223, #4708, #2058, #11581, #21073, #30596, #7202, #23567 ),
 .UNSPECIFIED., .F., .F.,
 ( 4, 2, 2, 2, 2, 2, 2, 2, 2, 4 ),
 ( 0.000000000000000000, 0.06250000000000076328, 0.1250000000000012212, 0.1875000000000016653, 0.2187500000000017208, 0.2500000000000017764, 0.3125000000000014433, 0.3750000000000010547, 0.4375000000000007216, 0.5000000000000000000 ),
 .UNSPECIFIED. ) ;
#8434 = EDGE_CURVE ( 'NONE', #8903, #20793, #1074, .T. ) ;
#8435 = CARTESIAN_POINT ( 'NONE',  ( 23.21076833940160000, 12.23288291591659771, 48.76310947893255587 ) ) ;
#8436 = DIRECTION ( 'NONE',  ( -0.000000000000000000, -0.000000000000000000, 1.000000000000000000 ) ) ;
#8437 = ORIENTED_EDGE ( 'NONE', *, *, #26378, .T. ) ;
#8438 = ADVANCED_FACE ( 'NONE', ( #14642 ), #2793, .F. ) ;
#8439 = DIRECTION ( 'NONE',  ( 1.000000000000000000, 0.000000000000000000, 0.000000000000000000 ) ) ;
#8440 = CIRCLE ( 'NONE', #18889, 0.7500000000000000000 ) ;
#8441 = CARTESIAN_POINT ( 'NONE',  ( -70.00000000000000000, 70.00000000000000000, -92.50000000000000000 ) ) ;
#8442 = AXIS2_PLACEMENT_3D ( 'NONE', #20677, #6346, #8389 ) ;
#8443 = CARTESIAN_POINT ( 'NONE',  ( 19.79689803950977378, 2.967719242317201633, 7.632642797338977658 ) ) ;
#8444 = VERTEX_POINT ( 'NONE', #14792 ) ;
#8445 = CARTESIAN_POINT ( 'NONE',  ( 14.94527285076313916, 13.31737086058187458, 5.653912893140659257 ) ) ;
#8446 = EDGE_LOOP ( 'NONE', ( #17702, #30394, #25882, #28951 ) ) ;
#8447 = EDGE_CURVE ( 'NONE', #17647, #1314, #24999, .T. ) ;
#8448 = CARTESIAN_POINT ( 'NONE',  ( 27.75715622479469147, -6.315477654728063328E-15, 1.500000000000001332 ) ) ;
#8449 = CARTESIAN_POINT ( 'NONE',  ( 1.000000000000000000, 29.50000000000000000, 24.50000000000000000 ) ) ;
#8450 = EDGE_LOOP ( 'NONE', ( #26012, #28936, #18670, #17136 ) ) ;
#8451 = AXIS2_PLACEMENT_3D ( 'NONE', #6106, #13463, #18584 ) ;
#8452 = EDGE_CURVE ( 'NONE', #17270, #16132, #18072, .T. ) ;
#8453 = ORIENTED_EDGE ( 'NONE', *, *, #3632, .F. ) ;
#8454 = EDGE_CURVE ( 'NONE', #13705, #21089, #15014, .T. ) ;
#8455 = CARTESIAN_POINT ( 'NONE',  ( 4.313865120791889218, 19.54726060313607050, 6.560937769032974209 ) ) ;
#8456 = CARTESIAN_POINT ( 'NONE',  ( 33.03707461445869598, 8.975870916883787132, 40.76550527633506960 ) ) ;
#8457 = CARTESIAN_POINT ( 'NONE',  ( -37.16608720827707657, 51.86186943028246787, 97.07879600563551037 ) ) ;
#8458 = CIRCLE ( 'NONE', #11942, 1.447898107987198646 ) ;
#8459 = CARTESIAN_POINT ( 'NONE',  ( -21.86019681245147694, -31.48592878035298170, 27.50000000000000355 ) ) ;
#8460 = DIRECTION ( 'NONE',  ( 1.000000000000000000, 0.000000000000000000, 0.000000000000000000 ) ) ;
#8461 = CARTESIAN_POINT ( 'NONE',  ( -2.662523238938575343, -12.47340865698848056, 1.500000000000001332 ) ) ;
#8462 = ORIENTED_EDGE ( 'NONE', *, *, #24018, .T. ) ;
#8463 = CARTESIAN_POINT ( 'NONE',  ( -19.77136997667518514, 3.131761183015793204, 20.12545155307891065 ) ) ;
#8464 = CARTESIAN_POINT ( 'NONE',  ( 18.21588581002256646, -8.300927319590593711, 5.701226463332907279 ) ) ;
#8465 = CARTESIAN_POINT ( 'NONE',  ( -15.98876933090332919, 12.04425525511918238, 19.25672174529527325 ) ) ;
#8466 = CARTESIAN_POINT ( 'NONE',  ( 45.40481135428485260, 69.10336821983588607, 60.91566813060281049 ) ) ;
#8467 = VERTEX_POINT ( 'NONE', #25549 ) ;
#8468 = VERTEX_POINT ( 'NONE', #20698 ) ;
#8469 = EDGE_CURVE ( 'NONE', #30552, #17265, #13554, .T. ) ;
#8470 = CARTESIAN_POINT ( 'NONE',  ( -15.34307810681595718, 12.82926163924266483, 7.652108011868850035 ) ) ;
#8471 = ADVANCED_FACE ( 'NONE', ( #4029 ), #1683, .F. ) ;
#8472 = CARTESIAN_POINT ( 'NONE',  ( -5.544451646083596863, 16.11829163520481956, 20.34789198813115263 ) ) ;
#8473 = LINE ( 'NONE', #24509, #5799 ) ;
#8474 = DIRECTION ( 'NONE',  ( -0.000000000000000000, 0.000000000000000000, 1.000000000000000000 ) ) ;
#8475 = CIRCLE ( 'NONE', #22405, 0.7500000000000002220 ) ;
#8476 = EDGE_CURVE ( 'NONE', #1130, #17481, #27454, .T. ) ;
#8477 = CARTESIAN_POINT ( 'NONE',  ( -4.776122516674677878E-15, -42.50000000000000000, 27.50000000000000355 ) ) ;
#8478 = LINE ( 'NONE', #22019, #454 ) ;
#8479 = ORIENTED_EDGE ( 'NONE', *, *, #22585, .T. ) ;
#8480 = EDGE_CURVE ( 'NONE', #18371, #9025, #27275, .T. ) ;
#8481 = AXIS2_PLACEMENT_3D ( 'NONE', #26443, #9904, #19419 ) ;
#8482 = DIRECTION ( 'NONE',  ( 1.000000000000000000, 0.000000000000000000, 0.000000000000000000 ) ) ;
#8483 = DIRECTION ( 'NONE',  ( 1.000000000000000000, 0.000000000000000000, 0.000000000000000000 ) ) ;
#8484 = CARTESIAN_POINT ( 'NONE',  ( -37.99999999999999289, 90.00000000000001421, -34.49999999999999289 ) ) ;
#8485 = ORIENTED_EDGE ( 'NONE', *, *, #14321, .T. ) ;
#8486 = VERTEX_POINT ( 'NONE', #10737 ) ;
#8487 = ADVANCED_FACE ( 'NONE', ( #27741 ), #20247, .T. ) ;
#8488 = CARTESIAN_POINT ( 'NONE',  ( -19.69679205574296788, 3.469720661875622891, 6.913388067999415298 ) ) ;
#8489 = LINE ( 'NONE', #24847, #1578 ) ;
#8490 = EDGE_LOOP ( 'NONE', ( #7893, #13931, #15623, #23623 ) ) ;
#8491 = CARTESIAN_POINT ( 'NONE',  ( 39.99999999999998579, 63.74772708486752038, 62.49999999999999289 ) ) ;
#8492 = CYLINDRICAL_SURFACE ( 'NONE', #19753, 0.7500000000000006661 ) ;
#8493 = CARTESIAN_POINT ( 'NONE',  ( -0.1262659238204836554, -8.999114229549588728, 21.50000000000000000 ) ) ;
#8494 = CARTESIAN_POINT ( 'NONE',  ( -36.62615482024158098, 14.61410224498927946, 16.44210843200423255 ) ) ;
#8495 = VECTOR ( 'NONE', #13470, 1000.000000000000000 ) ;
#8496 = CARTESIAN_POINT ( 'NONE',  ( -5.549074438232175055, 16.11683645458453995, 18.34798005862662507 ) ) ;
#8497 = DIRECTION ( 'NONE',  ( -0.000000000000000000, 1.132880637372608986E-16, -1.000000000000000000 ) ) ;
#8498 = CARTESIAN_POINT ( 'NONE',  ( 11.10715495309692891, -16.63223102436628409, 7.652108011868850035 ) ) ;
#8499 = CARTESIAN_POINT ( 'NONE',  ( -38.00000000000000000, 80.00000000000000000, 15.49999999999998579 ) ) ;
#8500 = CARTESIAN_POINT ( 'NONE',  ( -16.94861615807197097, 1.782241101862044319, 7.652108011868850923 ) ) ;
#8501 = ORIENTED_EDGE ( 'NONE', *, *, #21277, .T. ) ;
#8502 = EDGE_CURVE ( 'NONE', #26952, #16888, #25402, .T. ) ;
#8503 = ADVANCED_FACE ( 'NONE', ( #15718 ), #20551, .F. ) ;
#8504 = AXIS2_PLACEMENT_3D ( 'NONE', #23161, #16464, #18509 ) ;
#8505 = CARTESIAN_POINT ( 'NONE',  ( -9.159129059799163031, -14.35414742152909362, 20.05479082170252525 ) ) ;
#8506 = CARTESIAN_POINT ( 'NONE',  ( -17.86647173498021246, -9.028149653223252358, 7.559636331181775581 ) ) ;
#8507 = CARTESIAN_POINT ( 'NONE',  ( -6.290842788517061912, 19.00387417064636253, 7.603368798681074736 ) ) ;
#8508 = CARTESIAN_POINT ( 'NONE',  ( 11.56680498864186291, -16.33760111733342413, 5.810767894563978686 ) ) ;
#8509 = CARTESIAN_POINT ( 'NONE',  ( 35.76344986165623396, 22.29344514668041199, -19.50000000000000355 ) ) ;
#8510 = CARTESIAN_POINT ( 'NONE',  ( -2.081668171172168513E-14, 75.00000000000001421, 52.49999999999999289 ) ) ;
#8511 = VERTEX_POINT ( 'NONE', #30074 ) ;
#8512 = VERTEX_POINT ( 'NONE', #8711 ) ;
#8513 = DIRECTION ( 'NONE',  ( 0.000000000000000000, 1.000000000000000000, 0.000000000000000000 ) ) ;
#8514 = CARTESIAN_POINT ( 'NONE',  ( -37.98493438988128901, 11.12428508575241004, -1.500000000000000000 ) ) ;
#8515 = CARTESIAN_POINT ( 'NONE',  ( -2.341318239117458511, -42.45126916401905959, 28.84393386495551681 ) ) ;
#8516 = CARTESIAN_POINT ( 'NONE',  ( 12.33859880789482233, -8.132258305203423632, -16.50000000000000000 ) ) ;
#8517 = ORIENTED_EDGE ( 'NONE', *, *, #26947, .F. ) ;
#8518 = AXIS2_PLACEMENT_3D ( 'NONE', #23827, #21485, #9336 ) ;
#8519 = CARTESIAN_POINT ( 'NONE',  ( -11.21147646446735102, 30.29926891764210595, -1.500000000000000000 ) ) ;
#8520 = CARTESIAN_POINT ( 'NONE',  ( -5.374868878254082105, 44.10336124695542992, -19.50000000000000355 ) ) ;
#8521 = CARTESIAN_POINT ( 'NONE',  ( -11.19942626343432046, -16.59192963269641652, 7.272049892295485485 ) ) ;
#8522 = VERTEX_POINT ( 'NONE', #1234 ) ;
#8523 = CYLINDRICAL_SURFACE ( 'NONE', #371, 0.7500000000000006661 ) ;
#8524 = CARTESIAN_POINT ( 'NONE',  ( -20.69299247485714588, -36.03354106283070024, 34.51170679603197300 ) ) ;
#8525 = ORIENTED_EDGE ( 'NONE', *, *, #24096, .F. ) ;
#8526 = DIRECTION ( 'NONE',  ( -0.000000000000000000, -0.000000000000000000, 1.000000000000000000 ) ) ;
#8527 = ORIENTED_EDGE ( 'NONE', *, *, #14985, .T. ) ;
#8528 = DIRECTION ( 'NONE',  ( 0.000000000000000000, 0.000000000000000000, -1.000000000000000000 ) ) ;
#8529 = CARTESIAN_POINT ( 'NONE',  ( 0.000000000000000000, 1.699320956058915452E-16, -1.500000000000001776 ) ) ;
#8530 = CARTESIAN_POINT ( 'NONE',  ( 0.000000000000000000, 0.000000000000000000, 1.500000000000000000 ) ) ;
#8531 = CIRCLE ( 'NONE', #15995, 0.7500000000000004441 ) ;
#8532 = CARTESIAN_POINT ( 'NONE',  ( -17.02500080809207361, 1.126395502097476520, 5.759928666072748449 ) ) ;
#8534 = EDGE_CURVE ( 'NONE', #14561, #17054, #20010, .T. ) ;
#8533 = DIRECTION ( 'NONE',  ( 0.000000000000000000, 0.000000000000000000, 1.000000000000000000 ) ) ;
#8535 = CARTESIAN_POINT ( 'NONE',  ( -24.35970437652574105, -13.37404834226503070, -16.55003854064094426 ) ) ;
#8536 = DIRECTION ( 'NONE',  ( 1.000000000000000000, 0.000000000000000000, 0.000000000000000000 ) ) ;
#8537 = AXIS2_PLACEMENT_3D ( 'NONE', #17511, #29369, #6109 ) ;
#8538 = CARTESIAN_POINT ( 'NONE',  ( 9.860909914091287476, -13.90333503830274609, 7.652108011868850923 ) ) ;
#8539 = DIRECTION ( 'NONE',  ( 1.000000000000000000, 0.000000000000000000, 0.000000000000000000 ) ) ;
#8540 = DIRECTION ( 'NONE',  ( -1.000000000000000000, 0.000000000000000000, -4.565061778886335400E-17 ) ) ;
#8541 = VERTEX_POINT ( 'NONE', #3728 ) ;
#8542 = ORIENTED_EDGE ( 'NONE', *, *, #25401, .T. ) ;
#8543 = DIRECTION ( 'NONE',  ( 0.000000000000000000, 1.132880637372608986E-16, -1.000000000000000000 ) ) ;
#8544 = CARTESIAN_POINT ( 'NONE',  ( 39.83602371822922095, -11.57901747687539640, -19.50000000000000355 ) ) ;
#8545 = DIRECTION ( 'NONE',  ( -0.000000000000000000, -0.000000000000000000, 1.000000000000000000 ) ) ;
#8546 = VERTEX_POINT ( 'NONE', #3567 ) ;
#8547 = CARTESIAN_POINT ( 'NONE',  ( 7.500000000000000000, 0.000000000000000000, 0.000000000000000000 ) ) ;
#8548 = DIRECTION ( 'NONE',  ( 0.000000000000000000, 0.000000000000000000, 1.000000000000000000 ) ) ;
#8549 = ORIENTED_EDGE ( 'NONE', *, *, #15887, .F. ) ;
#8550 = VERTEX_POINT ( 'NONE', #17925 ) ;
#8551 = CARTESIAN_POINT ( 'NONE',  ( -11.35999944890269830, -16.46057145267183586, 19.47728749465736442 ) ) ;
#8552 = CARTESIAN_POINT ( 'NONE',  ( -8.550548372801090480, -14.74545326687210434, 20.34789198813115263 ) ) ;
#8553 = AXIS2_PLACEMENT_3D ( 'NONE', #6781, #4455, #13963 ) ;
#8554 = CARTESIAN_POINT ( 'NONE',  ( -10.55542352351189095, -17.00870908956209249, 18.34777357837151968 ) ) ;
#8555 = CARTESIAN_POINT ( 'NONE',  ( -19.64177907938615064, 36.71644397333972876, 24.50000000000000000 ) ) ;
#8556 = ORIENTED_EDGE ( 'NONE', *, *, #13204, .T. ) ;
#8557 = CARTESIAN_POINT ( 'NONE',  ( 8.413215745754998309, -3.196529495465417980, 1.500000000000001332 ) ) ;
#8558 = VERTEX_POINT ( 'NONE', #27437 ) ;
#8559 = CARTESIAN_POINT ( 'NONE',  ( 49.99999999999998579, -50.00000000000000000, -87.50000000000000000 ) ) ;
#8560 = CARTESIAN_POINT ( 'NONE',  ( 28.34828976096172681, 29.18752572968383419, 1.500000000000000000 ) ) ;
#8561 = VERTEX_POINT ( 'NONE', #1390 ) ;
#8562 = CARTESIAN_POINT ( 'NONE',  ( -6.102995743689038299, 19.04655207687856233, 18.34869673959211767 ) ) ;
#8563 = CIRCLE ( 'NONE', #29976, 9.084132297865673777 ) ;
#8564 = LINE ( 'NONE', #25398, #24542 ) ;
#8565 = DIRECTION ( 'NONE',  ( -0.000000000000000000, 1.000000000000000000, 0.000000000000000000 ) ) ;
#8566 = CARTESIAN_POINT ( 'NONE',  ( -13.23566211985188446, 10.73140863935235600, 18.36582235739946611 ) ) ;
#8567 = CARTESIAN_POINT ( 'NONE',  ( 1.590931199584701305, -16.99685872687011212, 6.037360021877312910 ) ) ;
#8568 = DIRECTION ( 'NONE',  ( -0.000000000000000000, -0.000000000000000000, -1.000000000000000000 ) ) ;
#8569 = CARTESIAN_POINT ( 'NONE',  ( -19.87079772360653607, 2.422354609568011519, 18.34838970509067479 ) ) ;
#8570 = DIRECTION ( 'NONE',  ( 1.000000000000000000, 0.000000000000000000, 0.000000000000000000 ) ) ;
#8571 = VERTEX_POINT ( 'NONE', #10907 ) ;
#8572 = DIRECTION ( 'NONE',  ( -0.000000000000000000, 0.000000000000000000, 1.000000000000000000 ) ) ;
#8573 = AXIS2_PLACEMENT_3D ( 'NONE', #4596, #23459, #8985 ) ;
#8574 = CARTESIAN_POINT ( 'NONE',  ( 23.69412710310942316, 29.84645176427128277, 34.80090346875809360 ) ) ;
#8575 = ORIENTED_EDGE ( 'NONE', *, *, #6930, .T. ) ;
#8576 = EDGE_LOOP ( 'NONE', ( #1205, #18432, #28252, #21161, #25804, #12163 ) ) ;
#8577 = DIRECTION ( 'NONE',  ( 0.000000000000000000, 0.000000000000000000, -1.000000000000000000 ) ) ;
#8578 = DIRECTION ( 'NONE',  ( -0.4154150130018840481, 0.9096319953545194403, 0.000000000000000000 ) ) ;
#8579 = CARTESIAN_POINT ( 'NONE',  ( -5.762218391735200562, 19.17087124927422437, 5.670038381137163519 ) ) ;
#8580 = VERTEX_POINT ( 'NONE', #23804 ) ;
#8581 = CYLINDRICAL_SURFACE ( 'NONE', #15128, 6.000000000000005329 ) ;
#8582 = CARTESIAN_POINT ( 'NONE',  ( -12.84881549437216819, 11.17046077493017897, 7.267659094423557065 ) ) ;
#8583 = CARTESIAN_POINT ( 'NONE',  ( 2.168404344971008868E-16, 30.50000000000000000, 1.500000000000000000 ) ) ;
#8584 = EDGE_LOOP ( 'NONE', ( #30779, #9816, #12208, #17630 ) ) ;
#8585 = VECTOR ( 'NONE', #29474, 1000.000000000000227 ) ;
#8586 = CARTESIAN_POINT ( 'NONE',  ( -57.50000000000001421, 50.00000000000000000, -87.50000000000000000 ) ) ;
#8587 = CARTESIAN_POINT ( 'NONE',  ( 14.39714448835432670, 13.90806243540158071, 5.951255046771932733 ) ) ;
#8588 = CARTESIAN_POINT ( 'NONE',  ( -33.03705654931147251, -8.970011997839668183, 40.76699977217946724 ) ) ;
#8589 = ORIENTED_EDGE ( 'NONE', *, *, #24863, .F. ) ;
#8590 = CARTESIAN_POINT ( 'NONE',  ( 19.54426622602689179, 37.07991288358296345, 1.499999999999999778 ) ) ;
#8591 = ORIENTED_EDGE ( 'NONE', *, *, #29583, .T. ) ;
#8592 = CIRCLE ( 'NONE', #25508, 7.500000000000000000 ) ;
#8593 = ORIENTED_EDGE ( 'NONE', *, *, #24439, .F. ) ;
#8594 = ORIENTED_EDGE ( 'NONE', *, *, #17172, .T. ) ;
#8595 = CARTESIAN_POINT ( 'NONE',  ( 4.678038002344204749, 19.46363151887951659, 5.872146474157316831 ) ) ;
#8596 = CARTESIAN_POINT ( 'NONE',  ( 33.21383100183306425, 9.208170138131603011, 40.53341495146639772 ) ) ;
#8597 = CARTESIAN_POINT ( 'NONE',  ( 6.139601762201234436, 19.03438667047814903, 18.84056766331482535 ) ) ;
#8598 = ORIENTED_EDGE ( 'NONE', *, *, #1927, .T. ) ;
#8599 = CARTESIAN_POINT ( 'NONE',  ( -9.268856789657290207, -38.25380398711768493, 34.80090346875804386 ) ) ;
#8600 = DIRECTION ( 'NONE',  ( 0.000000000000000000, 1.000000000000000000, 0.000000000000000000 ) ) ;
#8601 = CARTESIAN_POINT ( 'NONE',  ( 19.89797503522100541, 2.188012981718272076, 19.33715507985239412 ) ) ;
#8602 = EDGE_LOOP ( 'NONE', ( #26174, #7630, #16944, #26807 ) ) ;
#8603 = EDGE_CURVE ( 'NONE', #28210, #2701, #13058, .T. ) ;
#8604 = AXIS2_PLACEMENT_3D ( 'NONE', #14146, #21631, #30673 ) ;
#8605 = LINE ( 'NONE', #20587, #30656 ) ;
#8606 = CARTESIAN_POINT ( 'NONE',  ( 18.12620810650619418, -8.494884113463655240, 7.500898271101006820 ) ) ;
#8607 = CARTESIAN_POINT ( 'NONE',  ( -13.78503626495109913, 10.05991541429405167, 5.872146474157316831 ) ) ;
#8608 = CARTESIAN_POINT ( 'NONE',  ( 3.835725748988828787, 16.61467071301743559, 20.32367522806703874 ) ) ;
#8609 = ORIENTED_EDGE ( 'NONE', *, *, #27567, .F. ) ;
#8610 = CARTESIAN_POINT ( 'NONE',  ( 0.000000000000000000, 0.000000000000000000, -92.50000000000000000 ) ) ;
#8611 = CARTESIAN_POINT ( 'NONE',  ( 12.93167884982522153, 11.07185515092108297, 6.143977687428010981 ) ) ;
#8612 = DIRECTION ( 'NONE',  ( 1.000000000000000000, 0.000000000000000000, 0.000000000000000000 ) ) ;
#8613 = EDGE_CURVE ( 'NONE', #18506, #7773, #10554, .T. ) ;
#8614 = DIRECTION ( 'NONE',  ( -0.000000000000000000, -0.000000000000000000, 1.000000000000000000 ) ) ;
#8615 = ADVANCED_FACE ( 'NONE', ( #30831 ), #261, .T. ) ;
#8616 = LINE ( 'NONE', #18127, #30836 ) ;
#8617 = ORIENTED_EDGE ( 'NONE', *, *, #20863, .T. ) ;
#8618 = CARTESIAN_POINT ( 'NONE',  ( -33.54152001338305666, -10.01313039630840152, 35.75338942090700556 ) ) ;
#8619 = DIRECTION ( 'NONE',  ( -0.000000000000000000, -0.000000000000000000, 1.000000000000000000 ) ) ;
#8620 = CARTESIAN_POINT ( 'NONE',  ( 1.000000000000008438, 17.23749217771910480, 1.500000000000000000 ) ) ;
#8621 = ORIENTED_EDGE ( 'NONE', *, *, #12266, .T. ) ;
#8622 = AXIS2_PLACEMENT_3D ( 'NONE', #11227, #15598, #3599 ) ;
#8623 = ORIENTED_EDGE ( 'NONE', *, *, #28658, .T. ) ;
#8624 = FACE_OUTER_BOUND ( 'NONE', #23936, .T. ) ;
#8625 = CIRCLE ( 'NONE', #142, 21.71568325578263625 ) ;
#8626 = DIRECTION ( 'NONE',  ( 1.000000000000000000, 0.000000000000000000, 0.000000000000000000 ) ) ;
#8627 = EDGE_LOOP ( 'NONE', ( #18060, #19920, #4428, #23172 ) ) ;
#8628 = CARTESIAN_POINT ( 'NONE',  ( 0.08889351957746359501, -20.00017437841852441, 7.626647697317581631 ) ) ;
#8629 = ADVANCED_FACE ( 'NONE', ( #28358 ), #4780, .T. ) ;
#8630 = PLANE ( 'NONE',  #30695 ) ;
#8631 = EDGE_CURVE ( 'NONE', #11387, #30416, #21311, .T. ) ;
#8632 = CYLINDRICAL_SURFACE ( 'NONE', #18496, 14.52510309069105965 ) ;
#8633 = ADVANCED_FACE ( 'NONE', ( #2140 ), #1993, .F. ) ;
#8634 = CARTESIAN_POINT ( 'NONE',  ( -24.27860874716793660, -23.00333360197815935, -16.50001199999999812 ) ) ;
#8635 = CARTESIAN_POINT ( 'NONE',  ( 52.16608720827707657, -51.86186943028246787, 12.49999999999998401 ) ) ;
#8636 = EDGE_CURVE ( 'NONE', #26988, #10421, #4554, .T. ) ;
#8637 = LINE ( 'NONE', #3797, #29048 ) ;
#8638 = CARTESIAN_POINT ( 'NONE',  ( 0.5710336623368666986, -20.00960304012540547, 7.627891251804737927 ) ) ;
#8639 = CARTESIAN_POINT ( 'NONE',  ( -3.395021109945014270, 30.50000000000000355, 24.50000000000000000 ) ) ;
#8640 = ORIENTED_EDGE ( 'NONE', *, *, #18628, .T. ) ;
#8641 = ADVANCED_FACE ( 'NONE', ( #14288 ), #11808, .T. ) ;
#8642 = FACE_OUTER_BOUND ( 'NONE', #17003, .T. ) ;
#8643 = DIRECTION ( 'NONE',  ( 0.000000000000000000, 0.000000000000000000, 1.000000000000000000 ) ) ;
#8644 = ADVANCED_FACE ( 'NONE', ( #9628, #16647 ), #6982, .T. ) ;
#8645 = CARTESIAN_POINT ( 'NONE',  ( -6.044935790874364834, 19.08338196164711320, 7.652108011868850035 ) ) ;
#8646 = VECTOR ( 'NONE', #9194, 1000.000000000000000 ) ;
#8647 = CARTESIAN_POINT ( 'NONE',  ( 10.04466414020357057, -13.77914355952372638, 7.627891251804737927 ) ) ;
#8648 = EDGE_CURVE ( 'NONE', #29085, #18738, #11516, .T. ) ;
#8649 = VECTOR ( 'NONE', #19035, 1000.000000000000000 ) ;
#8650 = B_SPLINE_CURVE_WITH_KNOTS ( 'NONE', 3,
 ( #17101, #22690, #8532, #25191, #30037, #17887, #3836, #3536, #27551, #27402, #17568, #13361, #1342, #22855, #1506, #10860 ),
 .UNSPECIFIED., .F., .F.,
 ( 4, 2, 2, 2, 2, 2, 2, 4 ),
 ( 0.5000000000000000000, 0.6250000000000002220, 0.6875000000000004441, 0.7187500000000005551, 0.7500000000000006661, 0.8125000000000004441, 0.8750000000000002220, 1.000000000000000000 ),
 .UNSPECIFIED. ) ;
#8651 = CARTESIAN_POINT ( 'NONE',  ( -25.19442432475839055, 35.44676296258369064, -19.50000000000000355 ) ) ;
#8652 = LINE ( 'NONE', #30156, #12608 ) ;
#8653 = EDGE_LOOP ( 'NONE', ( #21876, #5630, #7459, #13115 ) ) ;
#8654 = DIRECTION ( 'NONE',  ( 0.000000000000000000, 0.000000000000000000, 1.000000000000000000 ) ) ;
#8655 = CARTESIAN_POINT ( 'NONE',  ( -5.374868878254082105, 44.10336124695542992, -19.50000000000000355 ) ) ;
#8656 = CARTESIAN_POINT ( 'NONE',  ( 37.01788418253418200, -13.43971458426429066, 31.66419126466463752 ) ) ;
#8657 = CARTESIAN_POINT ( 'NONE',  ( -5.976020107417634009, 19.08630880174946043, 5.652196082369965069 ) ) ;
#8658 = ORIENTED_EDGE ( 'NONE', *, *, #9213, .T. ) ;
#8659 = CARTESIAN_POINT ( 'NONE',  ( 3.537840656620562019, 16.69140805417697138, 5.759928666072750225 ) ) ;
#8660 = CARTESIAN_POINT ( 'NONE',  ( -4.163336342344337027E-14, -1.387778780781445676E-14, 1.500000000000000000 ) ) ;
#8661 = EDGE_CURVE ( 'NONE', #17425, #5751, #22986, .T. ) ;
#8662 = ORIENTED_EDGE ( 'NONE', *, *, #17175, .F. ) ;
#8663 = VECTOR ( 'NONE', #14482, 1000.000000000000000 ) ;
#8664 = CARTESIAN_POINT ( 'NONE',  ( 2.878478920843542177, 0.8451976705242683074, 24.50000000000000000 ) ) ;
#8665 = CARTESIAN_POINT ( 'NONE',  ( 22.58267429318974706, -26.57182937991349903, -1.500000000000000000 ) ) ;
#8666 = ORIENTED_EDGE ( 'NONE', *, *, #14717, .F. ) ;
#8667 = CARTESIAN_POINT ( 'NONE',  ( -30.38302862529102200, -15.53680216053817986, 40.87496192038616982 ) ) ;
#8668 = CIRCLE ( 'NONE', #9143, 0.7500000000000006661 ) ;
#8669 = EDGE_CURVE ( 'NONE', #23120, #24284, #7136, .T. ) ;
#8670 = AXIS2_PLACEMENT_3D ( 'NONE', #15815, #18477, #6001 ) ;
#8671 = EDGE_CURVE ( 'NONE', #20089, #7538, #108, .T. ) ;
#8672 = CARTESIAN_POINT ( 'NONE',  ( 4.622016212553096359, -12.19167610014704906, 24.50000000000000000 ) ) ;
#8673 = ORIENTED_EDGE ( 'NONE', *, *, #12144, .T. ) ;
#8674 = DIRECTION ( 'NONE',  ( 0.000000000000000000, 0.000000000000000000, 1.000000000000000000 ) ) ;
#8675 = CARTESIAN_POINT ( 'NONE',  ( 64.99999999999998579, -36.86186943028246787, 12.49999999999999112 ) ) ;
#8676 = CARTESIAN_POINT ( 'NONE',  ( 1.239979252855711866, -19.96159058730291136, 18.84486140012300126 ) ) ;
#8677 = CYLINDRICAL_SURFACE ( 'NONE', #26234, 6.000000000000001776 ) ;
#8678 = CARTESIAN_POINT ( 'NONE',  ( -3.469446951953614189E-15, -30.50000000000000711, 24.50000000000000000 ) ) ;
#8679 = DIRECTION ( 'NONE',  ( 0.000000000000000000, 0.000000000000000000, -1.000000000000000000 ) ) ;
#8680 = DIRECTION ( 'NONE',  ( -0.000000000000000000, -0.000000000000000000, 1.000000000000000000 ) ) ;
#8681 = DIRECTION ( 'NONE',  ( 0.000000000000000000, 1.000000000000000000, 0.000000000000000000 ) ) ;
#8682 = DIRECTION ( 'NONE',  ( 0.000000000000000000, 1.000000000000000000, 0.000000000000000000 ) ) ;
#8683 = CARTESIAN_POINT ( 'NONE',  ( -6.062559277181930106, 5.881244434206302607, 21.50000000000000000 ) ) ;
#8684 = DIRECTION ( 'NONE',  ( 0.000000000000000000, 0.000000000000000000, 1.000000000000000000 ) ) ;
#8685 = EDGE_LOOP ( 'NONE', ( #6679, #17449, #7672, #4338, #14178, #13565, #27908, #6271, #24480, #28066, #26208, #20426, #27777, #13212, #2311, #28326 ) ) ;
#8686 = EDGE_LOOP ( 'NONE', ( #29054, #16429, #19970, #21482 ) ) ;
#8687 = DIRECTION ( 'NONE',  ( -0.000000000000000000, -0.000000000000000000, 1.000000000000000000 ) ) ;
#8688 = AXIS2_PLACEMENT_3D ( 'NONE', #2773, #12599, #3386 ) ;
#8689 = DIRECTION ( 'NONE',  ( 0.6548607339452889864, 0.7557495743542548272, 0.000000000000000000 ) ) ;
#8690 = ORIENTED_EDGE ( 'NONE', *, *, #8004, .F. ) ;
#8691 = LINE ( 'NONE', #29743, #5423 ) ;
#8692 = DIRECTION ( 'NONE',  ( 0.000000000000000000, 0.000000000000000000, 1.000000000000000000 ) ) ;
#8693 = EDGE_CURVE ( 'NONE', #13794, #624, #2286, .T. ) ;
#8694 = VERTEX_POINT ( 'NONE', #28654 ) ;
#8695 = ORIENTED_EDGE ( 'NONE', *, *, #11159, .T. ) ;
#8696 = CARTESIAN_POINT ( 'NONE',  ( -15.71962203721309592, -1.249857212218242974, 1.500000000000001332 ) ) ;
#8697 = DIRECTION ( 'NONE',  ( 0.000000000000000000, 1.000000000000000000, 1.193512090021232842E-16 ) ) ;
#8698 = CARTESIAN_POINT ( 'NONE',  ( -8.546421330728131593, -14.74799399454104076, 18.34798005862930381 ) ) ;
#8699 = CARTESIAN_POINT ( 'NONE',  ( 4.963855673496207821, 42.15448181593355059, 34.60401223484481648 ) ) ;
#8700 = EDGE_LOOP ( 'NONE', ( #28361, #11221, #16200, #23914 ) ) ;
#8701 = CARTESIAN_POINT ( 'NONE',  ( -38.00000000000000000, 80.00000000000000000, -7.533656238527846826E-15 ) ) ;
#8702 = VERTEX_POINT ( 'NONE', #7284 ) ;
#8703 = CARTESIAN_POINT ( 'NONE',  ( 30.53339558441486190, -7.800891647352842462, 43.48653168448678485 ) ) ;
#8704 = CARTESIAN_POINT ( 'NONE',  ( 39.52380524535562500, 7.028748154183637631, -11.49999999999999645 ) ) ;
#8705 = VERTEX_POINT ( 'NONE', #16342 ) ;
#8706 = VECTOR ( 'NONE', #4960, 1000.000000000000000 ) ;
#8707 = CARTESIAN_POINT ( 'NONE',  ( -4.163336342344337027E-14, -1.387778780781445676E-14, 1.500000000000000000 ) ) ;
#8708 = CARTESIAN_POINT ( 'NONE',  ( 5.139473829620250456, -42.22092639811037174, 28.86348903593575699 ) ) ;
#8709 = CARTESIAN_POINT ( 'NONE',  ( 16.71904594334104388, 3.341332093703274442, 7.643931100913408550 ) ) ;
#8710 = CARTESIAN_POINT ( 'NONE',  ( -8.266165397079788590, -14.91833037834293307, 20.29915277494337644 ) ) ;
#8711 = CARTESIAN_POINT ( 'NONE',  ( 13.88429941593329531, 16.69721919943964039, 1.500000000000000000 ) ) ;
#8712 = DIRECTION ( 'NONE',  ( 0.000000000000000000, 1.000000000000000000, 1.193512090021232842E-16 ) ) ;
#8713 = DIRECTION ( 'NONE',  ( -0.000000000000000000, -0.000000000000000000, -1.000000000000000000 ) ) ;
#8714 = ORIENTED_EDGE ( 'NONE', *, *, #26578, .T. ) ;
#8715 = CARTESIAN_POINT ( 'NONE',  ( 11.77505735701808121, -16.18809529858903673, 18.73743063545763121 ) ) ;
#8716 = CARTESIAN_POINT ( 'NONE',  ( 34.83396020575241891, -10.30249279383517624, 34.80090346875810070 ) ) ;
#8717 = ORIENTED_EDGE ( 'NONE', *, *, #15315, .T. ) ;
#8718 = ORIENTED_EDGE ( 'NONE', *, *, #5583, .F. ) ;
#8719 = CARTESIAN_POINT ( 'NONE',  ( 49.99999999999998579, 70.00000000000000000, 22.49999999999999289 ) ) ;
#8720 = CARTESIAN_POINT ( 'NONE',  ( -67.00000000000000000, 50.00000000000000000, 62.49999999999999289 ) ) ;
#8721 = CARTESIAN_POINT ( 'NONE',  ( 33.42925964089141644, -11.06161099612213228, 35.54550565580004928 ) ) ;
#8722 = ORIENTED_EDGE ( 'NONE', *, *, #26877, .F. ) ;
#8723 = CYLINDRICAL_SURFACE ( 'NONE', #5677, 20.00000000000000000 ) ;
#8724 = DIRECTION ( 'NONE',  ( 0.000000000000000000, 0.000000000000000000, 1.000000000000000000 ) ) ;
#8725 = CIRCLE ( 'NONE', #12716, 0.7499999999999997780 ) ;
#8726 = CYLINDRICAL_SURFACE ( 'NONE', #12936, 2.000000000000001776 ) ;
#8727 = EDGE_LOOP ( 'NONE', ( #9644, #5607, #9650 ) ) ;
#8728 = LINE ( 'NONE', #4191, #3807 ) ;
#8729 = CARTESIAN_POINT ( 'NONE',  ( 0.000000000000000000, 10.00000000000003375, -87.50000000000000000 ) ) ;
#8730 = EDGE_LOOP ( 'NONE', ( #18214, #27262, #21690, #8158, #1948 ) ) ;
#8731 = EDGE_LOOP ( 'NONE', ( #25889, #25910, #26551, #26896 ) ) ;
#8732 = CARTESIAN_POINT ( 'NONE',  ( 0.000000000000000000, 15.00000000000001954, 29.43090101791767665 ) ) ;
#8733 = ORIENTED_EDGE ( 'NONE', *, *, #10143, .T. ) ;
#8734 = VERTEX_POINT ( 'NONE', #14458 ) ;
#8735 = CARTESIAN_POINT ( 'NONE',  ( -5.130938270761554065, 7.974144905643839820, 13.00000000000000178 ) ) ;
#8736 = CARTESIAN_POINT ( 'NONE',  ( 32.28307784207223108, -8.475829241206289666, 41.62281023987511475 ) ) ;
#8737 = EDGE_LOOP ( 'NONE', ( #19098, #14560, #3012, #8658 ) ) ;
#8738 = CIRCLE ( 'NONE', #754, 5.000000000000004441 ) ;
#8739 = CARTESIAN_POINT ( 'NONE',  ( -36.00000000000000000, -2.601438916704193360, 34.80090346875805096 ) ) ;
#8740 = CARTESIAN_POINT ( 'NONE',  ( 39.99999999999998579, 80.00000000000001421, 22.49999999999999289 ) ) ;
#8741 = FACE_OUTER_BOUND ( 'NONE', #5416, .T. ) ;
#8742 = VERTEX_POINT ( 'NONE', #23960 ) ;
#8743 = CARTESIAN_POINT ( 'NONE',  ( -16.93532286002824350, 1.879651667671730531, 20.32842677360128292 ) ) ;
#8744 = CARTESIAN_POINT ( 'NONE',  ( 15.55167013926946673, -6.938753487154071919, 5.862424720655265098 ) ) ;
#8745 = CARTESIAN_POINT ( 'NONE',  ( -13.52555592105307980, 10.38406032642568277, 5.678370764302467677 ) ) ;
#8746 = CARTESIAN_POINT ( 'NONE',  ( 4.330755352941443093, 19.54356050811956180, 19.14333282897057842 ) ) ;
#8747 = VERTEX_POINT ( 'NONE', #21625 ) ;
#8748 = ORIENTED_EDGE ( 'NONE', *, *, #7912, .T. ) ;
#8749 = DIRECTION ( 'NONE',  ( -0.000000000000000000, -0.000000000000000000, 1.000000000000000000 ) ) ;
#8750 = CARTESIAN_POINT ( 'NONE',  ( 10.08428597738326893, -13.75408489947211521, 5.653604225791663218 ) ) ;
#8751 = CARTESIAN_POINT ( 'NONE',  ( 8.197313248159948884, -3.914781618004724795, -1.500000000000002220 ) ) ;
#8752 = CARTESIAN_POINT ( 'NONE',  ( -5.055631408663415094, 19.36903233965648141, 19.00652017443069752 ) ) ;
#8753 = DIRECTION ( 'NONE',  ( 0.000000000000000000, -0.000000000000000000, -1.000000000000000000 ) ) ;
#8754 = EDGE_CURVE ( 'NONE', #3343, #25145, #28038, .T. ) ;
#8755 = LINE ( 'NONE', #13299, #27368 ) ;
#8756 = ORIENTED_EDGE ( 'NONE', *, *, #6473, .F. ) ;
#8757 = CARTESIAN_POINT ( 'NONE',  ( -19.92072812706008023, 1.967956072006117996, 7.500147780736496017 ) ) ;
#8758 = DIRECTION ( 'NONE',  ( 1.000000000000000000, 0.000000000000000000, 0.000000000000000000 ) ) ;
#8759 = CARTESIAN_POINT ( 'NONE',  ( 19.83258132550258424, 2.584089194578470750, 18.54479204710284179 ) ) ;
#8760 = EDGE_LOOP ( 'NONE', ( #5225, #26507, #22110, #10840 ) ) ;
#8761 = VECTOR ( 'NONE', #10479, 1000.000000000000000 ) ;
#8762 = LINE ( 'NONE', #545, #13316 ) ;
#8763 = VERTEX_POINT ( 'NONE', #25698 ) ;
#8764 = CARTESIAN_POINT ( 'NONE',  ( -19.84344116185557283, 2.497567387674354489, 7.652108011868850035 ) ) ;
#8765 = EDGE_CURVE ( 'NONE', #14232, #21410, #16028, .T. ) ;
#8766 = VECTOR ( 'NONE', #938, 1000.000000000000000 ) ;
#8767 = CARTESIAN_POINT ( 'NONE',  ( -19.91153203745398770, 1.881428233485403556, 20.15039051365863543 ) ) ;
#8768 = EDGE_LOOP ( 'NONE', ( #3510, #21833, #11526, #25676 ) ) ;
#8769 = DIRECTION ( 'NONE',  ( 0.000000000000000000, 0.000000000000000000, 1.000000000000000000 ) ) ;
#8770 = DIRECTION ( 'NONE',  ( -0.000000000000000000, 1.132880637372608986E-16, -1.000000000000000000 ) ) ;
#8771 = CARTESIAN_POINT ( 'NONE',  ( -13.72594918703051725, -39.82203247533167456, 21.93451384618056110 ) ) ;
#8772 = CYLINDRICAL_SURFACE ( 'NONE', #14784, 0.7500000000000006661 ) ;
#8773 = CARTESIAN_POINT ( 'NONE',  ( 2.516121109503181685, 8.728722367416592576, -1.500000000000000666 ) ) ;
#8774 = VECTOR ( 'NONE', #7950, 1000.000000000000000 ) ;
#8775 = EDGE_CURVE ( 'NONE', #1242, #28669, #17778, .T. ) ;
#8776 = DIRECTION ( 'NONE',  ( -0.000000000000000000, -0.000000000000000000, -1.000000000000000000 ) ) ;
#8777 = DIRECTION ( 'NONE',  ( 0.000000000000000000, -1.132880637372608986E-16, 1.000000000000000000 ) ) ;
#8778 = ORIENTED_EDGE ( 'NONE', *, *, #12803, .F. ) ;
#8779 = CARTESIAN_POINT ( 'NONE',  ( 39.99999999999998579, 87.00000000000001421, 59.49999999999999289 ) ) ;
#8780 = DIRECTION ( 'NONE',  ( -0.000000000000000000, -0.000000000000000000, -1.000000000000000000 ) ) ;
#8781 = CARTESIAN_POINT ( 'NONE',  ( -4.699300155672233359, 16.36248368692520927, 6.143977687428009204 ) ) ;
#8782 = AXIS2_PLACEMENT_3D ( 'NONE', #19992, #27172, #5800 ) ;
#8783 = CARTESIAN_POINT ( 'NONE',  ( 0.5584673446549298648, -9.967293815311123240, 0.7361406979141417173 ) ) ;
#8784 = AXIS2_PLACEMENT_3D ( 'NONE', #13317, #25151, #29854 ) ;
#8785 = SURFACE_STYLE_USAGE ( .BOTH. , #20637 ) ;
#8786 = EDGE_CURVE ( 'NONE', #25279, #8903, #16291, .T. ) ;
#8787 = DIRECTION ( 'NONE',  ( 0.000000000000000000, -0.5000000000000012212, 0.8660254037844380415 ) ) ;
#8788 = ORIENTED_EDGE ( 'NONE', *, *, #16599, .F. ) ;
#8789 = APPLICATION_CONTEXT ( 'automotive_design' ) ;
#8790 = CARTESIAN_POINT ( 'NONE',  ( -0.4553004113513210993, -19.99503986737292038, 19.96302680909624527 ) ) ;
#8791 = B_SPLINE_CURVE_WITH_KNOTS ( 'NONE', 3,
 ( #6444, #20620, #11432, #1298, #22960, #20476, #27964, #6126, #8771, #8942, #27654, #17997, #1615, #25475 ),
 .UNSPECIFIED., .F., .F.,
 ( 4, 2, 2, 2, 2, 2, 4 ),
 ( 0.02138939971592041661, 0.02672123144516384136, 0.02938714730978555373, 0.03205306317440725916, 0.03738489490365068391, 0.04005081076827241016, 0.04271672663289412947 ),
 .UNSPECIFIED. ) ;
#8792 = CARTESIAN_POINT ( 'NONE',  ( 5.105024945673418912, -42.22604126506271882, -1.500000000000000000 ) ) ;
#8793 = ADVANCED_FACE ( 'NONE', ( #29619 ), #6061, .F. ) ;
#8794 = CARTESIAN_POINT ( 'NONE',  ( 18.39838276040765308, -32.69867910685736234, 37.50000000001998757 ) ) ;
#8795 = EDGE_CURVE ( 'NONE', #25580, #19866, #23348, .T. ) ;
#8796 = DIRECTION ( 'NONE',  ( 1.000000000000000000, 0.000000000000000000, 0.000000000000000000 ) ) ;
#8797 = ORIENTED_EDGE ( 'NONE', *, *, #30719, .F. ) ;
#8798 = CARTESIAN_POINT ( 'NONE',  ( 3.264443111031099409, 16.75603743214636765, 7.269896094239229889 ) ) ;
#8799 = ORIENTED_EDGE ( 'NONE', *, *, #7282, .T. ) ;
#8800 = AXIS2_PLACEMENT_3D ( 'NONE', #23422, #20632, #13325 ) ;
#8801 = CARTESIAN_POINT ( 'NONE',  ( -10.64374042650075403, -42.96126232887726815, -19.50000000000000355 ) ) ;
#8802 = CARTESIAN_POINT ( 'NONE',  ( -35.00000000000000000, 90.00000000000001421, -22.50000000000002487 ) ) ;
#8803 = COLOUR_RGB ( '',0.7921568627450980005, 0.8196078431372548767, 0.9333333333333333481 ) ;
#8804 = ORIENTED_EDGE ( 'NONE', *, *, #13774, .T. ) ;
#8805 = EDGE_CURVE ( 'NONE', #9785, #6184, #8119, .T. ) ;
#8806 = CIRCLE ( 'NONE', #3902, 0.7500000000000011102 ) ;
#8807 = CARTESIAN_POINT ( 'NONE',  ( -19.72128910681292169, -31.90111139983629229, 37.50000000003792167 ) ) ;
#8808 = VERTEX_POINT ( 'NONE', #1078 ) ;
#8809 = CARTESIAN_POINT ( 'NONE',  ( -32.06725342158289038, -14.54034564589948708, 39.79052675593695199 ) ) ;
#8810 = VECTOR ( 'NONE', #21530, 1000.000000000000000 ) ;
#8811 = EDGE_CURVE ( 'NONE', #22904, #29639, #28740, .T. ) ;
#8812 = CIRCLE ( 'NONE', #29716, 0.7500000000000006661 ) ;
#8813 = CARTESIAN_POINT ( 'NONE',  ( -6.974883619896829146, -5.687793815610328707, -1.500000000000002220 ) ) ;
#8814 = CARTESIAN_POINT ( 'NONE',  ( 20.71335220384823117, 27.86167394782616213, -6.500000000000000888 ) ) ;
#8815 = ADVANCED_FACE ( 'NONE', ( #1959 ), #8418, .F. ) ;
#8816 = ORIENTED_EDGE ( 'NONE', *, *, #21570, .T. ) ;
#8817 = CARTESIAN_POINT ( 'NONE',  ( 23.21352257770656990, 10.78826658734920230, 45.15942333309104129 ) ) ;
#8818 = ADVANCED_FACE ( 'NONE', ( #27279 ), #5912, .F. ) ;
#8819 = CARTESIAN_POINT ( 'NONE',  ( 16.59744209610425614, 3.993643014774751698, 6.037360021877315575 ) ) ;
#8820 = DIRECTION ( 'NONE',  ( -1.000000000000000000, 0.000000000000000000, 0.000000000000000000 ) ) ;
#8821 = CARTESIAN_POINT ( 'NONE',  ( -42.40070334633576010, 68.50292470094652231, 12.78726508192041855 ) ) ;
#8822 = B_SPLINE_CURVE_WITH_KNOTS ( 'NONE', 3,
 ( #6276, #3637, #27651, #25623, #15788, #27814, #13312 ),
 .UNSPECIFIED., .F., .F.,
 ( 4, 3, 4 ),
 ( 0.000000000000000000, 0.005031266826610968426, 0.01006253384379828669 ),
 .UNSPECIFIED. ) ;
#8823 = AXIS2_PLACEMENT_3D ( 'NONE', #2643, #4824, #4675 ) ;
#8824 = CARTESIAN_POINT ( 'NONE',  ( 18.33599632111990729, -7.986941774664182425, 20.34789198813115263 ) ) ;
#8825 = CARTESIAN_POINT ( 'NONE',  ( 3.395021109945009385, -30.50000000000000711, 24.50000000000000000 ) ) ;
#8826 = CARTESIAN_POINT ( 'NONE',  ( -32.98805937973593672, 80.00000000000000000, 13.00000000000000178 ) ) ;
#8827 = LINE ( 'NONE', #8535, #26481 ) ;
#8828 = CARTESIAN_POINT ( 'NONE',  ( 9.248129367672065726, 2.094186647214772989, 21.50000000000000000 ) ) ;
#8829 = CARTESIAN_POINT ( 'NONE',  ( 38.00000000000000711, 209.2686044187655909, -22.50000000000002487 ) ) ;
#8830 = CARTESIAN_POINT ( 'NONE',  ( -9.225205623866960636, -14.30976465319822211, 18.72771030977187223 ) ) ;
#8831 = ORIENTED_EDGE ( 'NONE', *, *, #13390, .F. ) ;
#8832 = VERTEX_POINT ( 'NONE', #13094 ) ;
#8833 = VECTOR ( 'NONE', #22076, 1000.000000000000000 ) ;
#8834 = CARTESIAN_POINT ( 'NONE',  ( -7.749586724479453181, -2.959227181723774525, -1.500000000000002220 ) ) ;
#8835 = FACE_OUTER_BOUND ( 'NONE', #18317, .T. ) ;
#8836 = EDGE_CURVE ( 'NONE', #18738, #13283, #22587, .T. ) ;
#8837 = CARTESIAN_POINT ( 'NONE',  ( -11.86767874445213167, -1.850092897552710225, 1.500000000000001332 ) ) ;
#8838 = EDGE_CURVE ( 'NONE', #1929, #13391, #10299, .T. ) ;
#8839 = ORIENTED_EDGE ( 'NONE', *, *, #4616, .F. ) ;
#8840 =( LENGTH_UNIT ( ) NAMED_UNIT ( * ) SI_UNIT ( .MILLI., .METRE. ) );
#8841 = AXIS2_PLACEMENT_3D ( 'NONE', #18269, #25740, #25289 ) ;
#8842 = DIRECTION ( 'NONE',  ( 0.000000000000000000, 1.000000000000000000, -0.000000000000000000 ) ) ;
#8843 = EDGE_CURVE ( 'NONE', #14509, #6239, #4377, .T. ) ;
#8844 = CARTESIAN_POINT ( 'NONE',  ( 9.439370189418763601, -14.17768557490412640, 18.47056384035244037 ) ) ;
#8845 = AXIS2_PLACEMENT_3D ( 'NONE', #1220, #10720, #27724 ) ;
#8846 = VERTEX_POINT ( 'NONE', #11946 ) ;
#8847 = CARTESIAN_POINT ( 'NONE',  ( -19.71077436674131178, 3.493128416889931032, 6.530762810602277924 ) ) ;
#8848 = EDGE_CURVE ( 'NONE', #13827, #7538, #3827, .T. ) ;
#8849 = VECTOR ( 'NONE', #12514, 999.9999999999998863 ) ;
#8850 = VECTOR ( 'NONE', #9126, 1000.000000000000000 ) ;
#8851 = CARTESIAN_POINT ( 'NONE',  ( -5.720368925487725242, -43.64004031045374887, -16.49999999999999645 ) ) ;
#8852 = FACE_OUTER_BOUND ( 'NONE', #25630, .T. ) ;
#8853 = VERTEX_POINT ( 'NONE', #9898 ) ;
#8854 = CARTESIAN_POINT ( 'NONE',  ( -37.16608720827707657, 65.00000000000000000, 57.49999999999999289 ) ) ;
#8855 = ORIENTED_EDGE ( 'NONE', *, *, #5206, .T. ) ;
#8856 = VECTOR ( 'NONE', #5482, 1000.000000000000000 ) ;
#8857 = ADVANCED_FACE ( 'NONE', ( #28471 ), #7723, .F. ) ;
#8858 = FACE_OUTER_BOUND ( 'NONE', #18944, .T. ) ;
#8859 = DIRECTION ( 'NONE',  ( 1.000000000000000000, 0.000000000000000000, 0.000000000000000000 ) ) ;
#8860 = AXIS2_PLACEMENT_3D ( 'NONE', #7977, #19971, #22452 ) ;
#8861 = ORIENTED_EDGE ( 'NONE', *, *, #28868, .F. ) ;
#8862 = VECTOR ( 'NONE', #29457, 1000.000000000000000 ) ;
#8863 = FACE_OUTER_BOUND ( 'NONE', #17465, .T. ) ;
#8864 = DIRECTION ( 'NONE',  ( -0.000000000000000000, 1.132880637372608986E-16, -1.000000000000000000 ) ) ;
#8865 = DIRECTION ( 'NONE',  ( -1.000000000000000000, 0.000000000000000000, 0.000000000000000000 ) ) ;
#8866 = LINE ( 'NONE', #4025, #23241 ) ;
#8867 = CARTESIAN_POINT ( 'NONE',  ( 25.53015708495999547, -6.470147010658199527, 48.66282223834831200 ) ) ;
#8868 = B_SPLINE_CURVE_WITH_KNOTS ( 'NONE', 3,
 ( #2496, #28860, #19030, #12165 ),
 .UNSPECIFIED., .F., .F.,
 ( 4, 4 ),
 ( 0.000000000000000000, 0.005028157979160191408 ),
 .UNSPECIFIED. ) ;
#8869 = DIRECTION ( 'NONE',  ( 0.000000000000000000, 0.000000000000000000, -1.000000000000000000 ) ) ;
#8870 = LINE ( 'NONE', #3568, #7539 ) ;
#8871 = FACE_OUTER_BOUND ( 'NONE', #16013, .T. ) ;
#8872 = ORIENTED_EDGE ( 'NONE', *, *, #15485, .F. ) ;
#8873 = AXIS2_PLACEMENT_3D ( 'NONE', #23338, #4763, #6968 ) ;
#8874 = EDGE_CURVE ( 'NONE', #22820, #1637, #27749, .T. ) ;
#8875 = AXIS2_PLACEMENT_3D ( 'NONE', #2334, #26362, #23688 ) ;
#8876 = EDGE_CURVE ( 'NONE', #2425, #20269, #4332, .T. ) ;
#8877 = CARTESIAN_POINT ( 'NONE',  ( 10.14446381905444561, -13.71082019663804452, 18.39992786714538298 ) ) ;
#8878 = CARTESIAN_POINT ( 'NONE',  ( 36.00000000000001421, 2.601438916704194249, 27.50000000000000355 ) ) ;
#8879 = AXIS2_PLACEMENT_3D ( 'NONE', #21933, #562, #19595 ) ;
#8880 = ORIENTED_EDGE ( 'NONE', *, *, #24663, .F. ) ;
#8881 = ORIENTED_EDGE ( 'NONE', *, *, #22169, .F. ) ;
#8882 = CARTESIAN_POINT ( 'NONE',  ( -5.549074438707202184, 16.11683645443577717, 5.652196082367002106 ) ) ;
#8883 = EDGE_LOOP ( 'NONE', ( #11950, #11373 ) ) ;
#8884 = CARTESIAN_POINT ( 'NONE',  ( 11.77411685406914188, -16.16721897189997037, 18.73377938172349033 ) ) ;
#8885 = AXIS2_PLACEMENT_3D ( 'NONE', #16172, #4163, #23485 ) ;
#8886 = CARTESIAN_POINT ( 'NONE',  ( -13.04869608158528393, 10.94699654828723645, 7.526951045817045660 ) ) ;
#8887 = AXIS2_PLACEMENT_3D ( 'NONE', #18788, #20947, #4274 ) ;
#8888 = DIRECTION ( 'NONE',  ( 0.000000000000000000, 0.000000000000000000, 1.000000000000000000 ) ) ;
#8889 = VERTEX_POINT ( 'NONE', #26595 ) ;
#8890 = CARTESIAN_POINT ( 'NONE',  ( 29.61203839202725518, -15.40012917324033381, 41.62281023987508632 ) ) ;
#8891 = CARTESIAN_POINT ( 'NONE',  ( -32.49058853941425440, -8.555876215535434426, 41.40177460044399993 ) ) ;
#8892 = ORIENTED_EDGE ( 'NONE', *, *, #19283, .F. ) ;
#8893 = DIRECTION ( 'NONE',  ( -1.000000000000000000, 0.000000000000000000, 0.000000000000000000 ) ) ;
#8894 = ORIENTED_EDGE ( 'NONE', *, *, #19817, .T. ) ;
#8895 = CARTESIAN_POINT ( 'NONE',  ( 39.99999999999998579, 90.00000000000001421, 27.49999999999998934 ) ) ;
#8896 = PRODUCT_DEFINITION_CONTEXT ( 'detailed design', #4016, 'design' ) ;
#8897 = VECTOR ( 'NONE', #1503, 1000.000000000000000 ) ;
#8898 = VERTEX_POINT ( 'NONE', #7243 ) ;
#8899 = AXIS2_PLACEMENT_3D ( 'NONE', #27164, #27014, #22162 ) ;
#8900 = ORIENTED_EDGE ( 'NONE', *, *, #24351, .T. ) ;
#8901 = CARTESIAN_POINT ( 'NONE',  ( 33.26833594138172145, 9.291422874672347731, 40.45861409864419045 ) ) ;
#8902 = CARTESIAN_POINT ( 'NONE',  ( -17.59389297287863485, -9.510918850537244396, 6.392525840300348428 ) ) ;
#8903 = VERTEX_POINT ( 'NONE', #14723 ) ;
#8904 = AXIS2_PLACEMENT_3D ( 'NONE', #28717, #25651, #9682 ) ;
#8905 = CARTESIAN_POINT ( 'NONE',  ( -27.03943647958861263, -26.20092231554396278, 34.80090346875804386 ) ) ;
#8906 = DIRECTION ( 'NONE',  ( 0.000000000000000000, 0.000000000000000000, 1.000000000000000000 ) ) ;
#8907 = CARTESIAN_POINT ( 'NONE',  ( 16.77888236039447278, 2.967719242317201633, 20.32842677360128292 ) ) ;
#8908 = VERTEX_POINT ( 'NONE', #9735 ) ;
#8909 = CARTESIAN_POINT ( 'NONE',  ( -19.81587719261256453, 2.836291464538557516, 20.29090034784956131 ) ) ;
#8910 = CARTESIAN_POINT ( 'NONE',  ( 15.45190528822776344, -7.145941350103559131, 7.176035686813569292 ) ) ;
#8911 = EDGE_CURVE ( 'NONE', #28030, #20761, #2880, .T. ) ;
#8912 = CARTESIAN_POINT ( 'NONE',  ( -14.01100295375882965, 9.765235586930179679, 6.672349528511551497 ) ) ;
#8913 = CARTESIAN_POINT ( 'NONE',  ( 3.424309912165880210, 16.71834993634869448, 18.56793045041961321 ) ) ;
#8914 = ORIENTED_EDGE ( 'NONE', *, *, #2381, .F. ) ;
#8915 = ORIENTED_EDGE ( 'NONE', *, *, #12643, .F. ) ;
#8916 = EDGE_CURVE ( 'NONE', #14001, #12141, #21902, .T. ) ;
#8917 = FACE_BOUND ( 'NONE', #24843, .T. ) ;
#8918 = PRODUCT_DEFINITION_FORMATION_WITH_SPECIFIED_SOURCE ( 'ANY', '', #5199, .NOT_KNOWN. ) ;
#8919 = CARTESIAN_POINT ( 'NONE',  ( 15.53710936759973116, 12.59357901975564076, 19.21471108562413832 ) ) ;
#8920 = B_SPLINE_SURFACE_WITH_KNOTS ( 'NONE', 3, 1, ( 
 ( #5982, #8496 ),
 ( #27358, #22649 ),
 ( #17999, #13481 ),
 ( #22962, #24459 ),
 ( #17129, #2207 ),
 ( #23561, #7622 ),
 ( #14639, #28420 ),
 ( #19620, #19474 ),
 ( #28988, #24141 ),
 ( #29142, #17287 ),
 ( #7777, #4549 ),
 ( #14789, #16552 ),
 ( #9233, #23417 ),
 ( #18748, #7043 ),
 ( #3102, #26820 ),
 ( #26651, #24306 ),
 ( #2789, #12308 ),
 ( #21810, #452 ),
 ( #2053, #2956 ),
 ( #12474, #25770 ),
 ( #28265, #5282 ),
 ( #21964, #4400 ),
 ( #18604, #592 ),
 ( #5445, #14948 ),
 ( #9970, #10110 ),
 ( #11576, #11725 ),
 ( #12621, #30446 ),
 ( #6891, #21216 ),
 ( #9087, #28115 ),
 ( #6737, #16248 ),
 ( #21070, #30592 ) ),
 .UNSPECIFIED., .F., .F., .F.,
 ( 4, 3, 3, 3, 3, 3, 3, 3, 3, 3, 4 ),
 ( 2, 2 ),
 ( 0.4999999998345686092, 0.5360336730431939367, 0.5907651151589012883, 0.6456034593241830599, 0.6998270958050434309, 0.7529536536315937223, 0.8052385063053260073, 0.8575343587103997356, 0.9106564858195042023, 0.9648414833209685293, 1.000000006602610236 ),
 ( 0.000000000000000000, 1.000000000000000000 ),
 .UNSPECIFIED. ) ;
#8921 = CARTESIAN_POINT ( 'NONE',  ( -4.721574378597740207, 16.35655934831870084, 18.80699882434806369 ) ) ;
#8922 = CYLINDRICAL_SURFACE ( 'NONE', #22723, 9.482273699623480212 ) ;
#8923 = VECTOR ( 'NONE', #15444, 1000.000000000000000 ) ;
#8924 = CARTESIAN_POINT ( 'NONE',  ( -3.515970705488605130, -17.06554576617236307, 1.500000000000000000 ) ) ;
#8925 = CIRCLE ( 'NONE', #25836, 0.7500000000000006661 ) ;
#8926 = CARTESIAN_POINT ( 'NONE',  ( 36.00000000000000000, -1.546978760965586295E-11, 34.75735931288068059 ) ) ;
#8927 = CARTESIAN_POINT ( 'NONE',  ( 23.11524226670867321, -11.10088790631998634, 49.35779847069012050 ) ) ;
#8928 = EDGE_LOOP ( 'NONE', ( #14893, #24086, #11584, #18136 ) ) ;
#8929 = CARTESIAN_POINT ( 'NONE',  ( -17.06646200723453433, 0.6378183210065198061, 6.560937769032974209 ) ) ;
#8930 = AXIS2_PLACEMENT_3D ( 'NONE', #12917, #22704, #25206 ) ;
#8931 = DIRECTION ( 'NONE',  ( 0.000000000000000000, 0.000000000000000000, 1.000000000000000000 ) ) ;
#8932 = ORIENTED_EDGE ( 'NONE', *, *, #23604, .F. ) ;
#8933 = CARTESIAN_POINT ( 'NONE',  ( 37.16608720827707657, 51.86186943028246787, 57.49999999999999289 ) ) ;
#8934 = ORIENTED_EDGE ( 'NONE', *, *, #6189, .T. ) ;
#8935 = CARTESIAN_POINT ( 'NONE',  ( -3.431238874299064712, -42.34547772617858641, 28.85304416643127823 ) ) ;
#8936 = UNCERTAINTY_MEASURE_WITH_UNIT (LENGTH_MEASURE( 1.000000000000000082E-05 ), #12715, 'distance_accuracy_value', 'NONE');
#8937 = VECTOR ( 'NONE', #27668, 1000.000000000000000 ) ;
#8938 = CARTESIAN_POINT ( 'NONE',  ( -12.50000000000000000, 0.000000000000000000, -52.50000000000000000 ) ) ;
#8939 = ORIENTED_EDGE ( 'NONE', *, *, #24637, .F. ) ;
#8940 = DIRECTION ( 'NONE',  ( -0.000000000000000000, -0.000000000000000000, 1.000000000000000000 ) ) ;
#8941 = CARTESIAN_POINT ( 'NONE',  ( 13.46952963749417798, 48.15317560926965257, -61.67470994988012478 ) ) ;
#8942 = CARTESIAN_POINT ( 'NONE',  ( -16.01986981312618852, -38.75956249542284127, 22.81220643827916561 ) ) ;
#8943 = LINE ( 'NONE', #29997, #14342 ) ;
#8944 = DIRECTION ( 'NONE',  ( 1.000000000000000000, 0.000000000000000000, 0.000000000000000000 ) ) ;
#8945 = AXIS2_PLACEMENT_3D ( 'NONE', #29433, #17571, #1044 ) ;
#8946 = CARTESIAN_POINT ( 'NONE',  ( -12.24063095261064227, 4.490763173670005770, 24.50000000000000000 ) ) ;
#8947 = CARTESIAN_POINT ( 'NONE',  ( 1.792916928892099859, -16.98383425522535006, 6.782048567692550378 ) ) ;
#8948 = CARTESIAN_POINT ( 'NONE',  ( -19.18576292979354037, 22.55620591602727387, 24.50000000000000000 ) ) ;
#8949 = ORIENTED_EDGE ( 'NONE', *, *, #10730, .T. ) ;
#8950 = DIRECTION ( 'NONE',  ( 0.000000000000000000, 0.000000000000000000, 1.000000000000000000 ) ) ;
#8951 = LINE ( 'NONE', #21694, #21743 ) ;
#8952 = ORIENTED_EDGE ( 'NONE', *, *, #5385, .T. ) ;
#8953 = LINE ( 'NONE', #18469, #11069 ) ;
#8954 = DIRECTION ( 'NONE',  ( -0.000000000000000000, -1.000000000000000000, -0.000000000000000000 ) ) ;
#8955 = CARTESIAN_POINT ( 'NONE',  ( 23.96732207938043402, -33.98584080152387088, -1.500000000000000000 ) ) ;
#8956 = CIRCLE ( 'NONE', #6943, 6.000000000000005329 ) ;
#8957 = CARTESIAN_POINT ( 'NONE',  ( 25.19442432473618254, -35.44676296258426618, -19.50000000000000355 ) ) ;
#8958 = ORIENTED_EDGE ( 'NONE', *, *, #23694, .F. ) ;
#8959 = CARTESIAN_POINT ( 'NONE',  ( -0.1550506074450101746, -19.99977091204052115, 20.22277707861862339 ) ) ;
#8960 = CARTESIAN_POINT ( 'NONE',  ( 1.000000000000000000, 29.50000000000000000, 43.10779406592839536 ) ) ;
#8961 = CARTESIAN_POINT ( 'NONE',  ( 35.21442488810127713, -18.31310691302397231, 31.23994917172689156 ) ) ;
#8962 = DIRECTION ( 'NONE',  ( 0.000000000000000000, 0.000000000000000000, -1.000000000000000000 ) ) ;
#8963 = ORIENTED_EDGE ( 'NONE', *, *, #10536, .F. ) ;
#8964 = FACE_BOUND ( 'NONE', #669, .T. ) ;
#8965 = DIRECTION ( 'NONE',  ( 1.000000000000000000, -2.890115478905172036E-15, 0.000000000000000000 ) ) ;
#8966 = DIRECTION ( 'NONE',  ( -0.000000000000000000, -0.000000000000000000, -1.000000000000000000 ) ) ;
#8967 = ORIENTED_EDGE ( 'NONE', *, *, #17426, .F. ) ;
#8968 = AXIS2_PLACEMENT_3D ( 'NONE', #20268, #8888, #1699 ) ;
#8969 = CARTESIAN_POINT ( 'NONE',  ( -18.17090117368252322, -32.80884700149822208, 37.50000000002933120 ) ) ;
#8970 = ORIENTED_EDGE ( 'NONE', *, *, #21099, .T. ) ;
#8971 = DIRECTION ( 'NONE',  ( 1.000000000000000000, 0.000000000000000000, 0.000000000000000000 ) ) ;
#8972 = LINE ( 'NONE', #20808, #19337 ) ;
#8973 = DIRECTION ( 'NONE',  ( 0.000000000000000000, 1.000000000000000000, -1.669238443041286689E-16 ) ) ;
#8974 = ORIENTED_EDGE ( 'NONE', *, *, #4207, .F. ) ;
#8975 = CARTESIAN_POINT ( 'NONE',  ( 12.17894461864673517, 11.93905285490450119, 18.34938820207544907 ) ) ;
#8976 = CARTESIAN_POINT ( 'NONE',  ( 16.74250988114178185, 3.198928528055117848, 5.652196082368483587 ) ) ;
#8977 = EDGE_CURVE ( 'NONE', #3499, #3241, #9967, .T. ) ;
#8978 = DIRECTION ( 'NONE',  ( -0.000000000000000000, -0.000000000000000000, -1.000000000000000000 ) ) ;
#8979 = ADVANCED_FACE ( 'NONE', ( #4746 ), #16754, .T. ) ;
#8980 = CARTESIAN_POINT ( 'NONE',  ( -40.58796716123164572, 67.65997107450050407, 12.49999999999998579 ) ) ;
#8981 = EDGE_CURVE ( 'NONE', #16618, #7784, #7323, .T. ) ;
#8982 = ADVANCED_FACE ( 'NONE', ( #14580 ), #29694, .F. ) ;
#8983 = CYLINDRICAL_SURFACE ( 'NONE', #14779, 1.999999999999998224 ) ;
#8984 = CARTESIAN_POINT ( 'NONE',  ( 0.000000000000000000, 12.50000000000000000, -87.50000000000000000 ) ) ;
#8985 = DIRECTION ( 'NONE',  ( 0.000000000000000000, 1.000000000000000000, 0.000000000000000000 ) ) ;
#8986 = CARTESIAN_POINT ( 'NONE',  ( 12.11357906259289230, 40.40859726677000197, 21.44996032281847320 ) ) ;
#8987 = CARTESIAN_POINT ( 'NONE',  ( 69.99999999999998579, 50.00000000000000000, 12.49999999999999112 ) ) ;
#8988 = ADVANCED_FACE ( 'NONE', ( #22048 ), #19879, .F. ) ;
#8989 = CARTESIAN_POINT ( 'NONE',  ( -18.46427634282259334, -7.732205987805708780, 19.56050940960062690 ) ) ;
#8990 = AXIS2_PLACEMENT_3D ( 'NONE', #3626, #29208, #1129 ) ;
#8991 = CARTESIAN_POINT ( 'NONE',  ( -3.763133143576374628, 8.268028093133407808, 13.22130136205108997 ) ) ;
#8992 = ORIENTED_EDGE ( 'NONE', *, *, #24601, .T. ) ;
#8993 = VERTEX_POINT ( 'NONE', #12558 ) ;
#8994 = DIRECTION ( 'NONE',  ( 0.000000000000000000, 0.000000000000000000, -1.000000000000000000 ) ) ;
#8995 = CARTESIAN_POINT ( 'NONE',  ( 5.105024945673418912, -42.22604126506271882, -1.500000000000000000 ) ) ;
#8996 = ADVANCED_FACE ( 'NONE', ( #27054 ), #17871, .T. ) ;
#8997 = DIRECTION ( 'NONE',  ( 1.000000000000000000, 0.000000000000000000, 0.000000000000000000 ) ) ;
#8998 = ORIENTED_EDGE ( 'NONE', *, *, #5777, .F. ) ;
#8999 = CARTESIAN_POINT ( 'NONE',  ( 0.000000000000000000, 0.000000000000000000, 26.00000000000000355 ) ) ;
#9000 = CARTESIAN_POINT ( 'NONE',  ( 15.40685886292496676, -7.237730981567044530, 19.66989035740801839 ) ) ;
#9001 = EDGE_CURVE ( 'NONE', #9137, #9666, #15275, .T. ) ;
#9002 = FACE_OUTER_BOUND ( 'NONE', #7173, .T. ) ;
#9003 = ADVANCED_FACE ( 'NONE', ( #22825 ), #22970, .T. ) ;
#9004 = VERTEX_POINT ( 'NONE', #20488 ) ;
#9005 = DIRECTION ( 'NONE',  ( 1.000000000000000000, 0.000000000000000000, 0.000000000000000000 ) ) ;
#9006 = CARTESIAN_POINT ( 'NONE',  ( 15.28716501070585387, 12.89617714416415239, 5.849008070840543638 ) ) ;
#9007 = CARTESIAN_POINT ( 'NONE',  ( 0.000000000000000000, 0.000000000000000000, 21.50000000000000000 ) ) ;
#9008 = ORIENTED_EDGE ( 'NONE', *, *, #21011, .T. ) ;
#9009 = FACE_OUTER_BOUND ( 'NONE', #5048, .T. ) ;
#9010 = DIRECTION ( 'NONE',  ( 0.000000000000000000, 1.132880637372608986E-16, -1.000000000000000000 ) ) ;
#9011 = AXIS2_PLACEMENT_3D ( 'NONE', #9007, #16018, #30059 ) ;
#9012 = CARTESIAN_POINT ( 'NONE',  ( 22.95669091611932089, -27.54300778121948312, 1.500000000000000000 ) ) ;
#9013 = VERTEX_POINT ( 'NONE', #1628 ) ;
#9014 = DIRECTION ( 'NONE',  ( 1.000000000000000000, 0.000000000000000000, 0.000000000000000000 ) ) ;
#9015 = EDGE_CURVE ( 'NONE', #2444, #15417, #9243, .T. ) ;
#9016 = LINE ( 'NONE', #23182, #326 ) ;
#9017 = EDGE_CURVE ( 'NONE', #26600, #14545, #12571, .T. ) ;
#9018 = DIRECTION ( 'NONE',  ( 0.000000000000000000, 0.000000000000000000, 1.000000000000000000 ) ) ;
#9019 = CARTESIAN_POINT ( 'NONE',  ( -0.5696721008582752432, -20.00987732873323566, 7.080843742048788414 ) ) ;
#9020 = ADVANCED_FACE ( 'NONE', ( #6749 ), #18389, .T. ) ;
#9021 = EDGE_CURVE ( 'NONE', #18086, #1853, #28431, .T. ) ;
#9022 = DIRECTION ( 'NONE',  ( 0.000000000000000000, 1.000000000000000000, 0.000000000000000000 ) ) ;
#9023 = CARTESIAN_POINT ( 'NONE',  ( -17.06430796155045115, 0.6673913134545759185, 19.61324152429826739 ) ) ;
#9024 = LINE ( 'NONE', #16036, #21339 ) ;
#9025 = VERTEX_POINT ( 'NONE', #12050 ) ;
#9026 = ADVANCED_FACE ( 'NONE', ( #6907 ), #23728, .F. ) ;
#9027 = DIRECTION ( 'NONE',  ( 0.9594929736144974797, 0.2817325568414297265, 0.000000000000000000 ) ) ;
#9028 = CARTESIAN_POINT ( 'NONE',  ( 34.13832859401787800, -12.80067323710190053, 27.50000000000001776 ) ) ;
#9029 = ORIENTED_EDGE ( 'NONE', *, *, #9021, .T. ) ;
#9030 = VERTEX_POINT ( 'NONE', #12198 ) ;
#9031 = EDGE_CURVE ( 'NONE', #23685, #353, #9297, .T. ) ;
#9032 = DIRECTION ( 'NONE',  ( 0.000000000000000000, 0.000000000000000000, 1.000000000000000000 ) ) ;
#9033 = EDGE_CURVE ( 'NONE', #17339, #12561, #16883, .T. ) ;
#9034 = AXIS2_PLACEMENT_3D ( 'NONE', #22191, #29220, #27192 ) ;
#9035 = ORIENTED_EDGE ( 'NONE', *, *, #25213, .T. ) ;
#9036 = CIRCLE ( 'NONE', #13021, 0.7500000000000002220 ) ;
#9037 = DIRECTION ( 'NONE',  ( 0.000000000000000000, 1.000000000000000000, 1.193512090021232842E-16 ) ) ;
#9038 = LINE ( 'NONE', #1855, #5447 ) ;
#9039 = DIRECTION ( 'NONE',  ( 1.000000000000000000, 0.000000000000000000, 0.000000000000000000 ) ) ;
#9040 = DIRECTION ( 'NONE',  ( 0.000000000000000000, 1.000000000000000000, 1.193512090021232842E-16 ) ) ;
#9041 = EDGE_LOOP ( 'NONE', ( #8349, #22380 ) ) ;
#9042 = EDGE_LOOP ( 'NONE', ( #25865, #15155, #4731, #24771 ) ) ;
#9043 = EDGE_CURVE ( 'NONE', #21028, #1458, #1333, .T. ) ;
#9044 = CARTESIAN_POINT ( 'NONE',  ( 0.000000000000000000, 0.000000000000000000, 1.500000000000000000 ) ) ;
#9045 = EDGE_CURVE ( 'NONE', #2551, #19699, #13802, .T. ) ;
#9046 = ORIENTED_EDGE ( 'NONE', *, *, #6512, .F. ) ;
#9047 = ORIENTED_EDGE ( 'NONE', *, *, #8203, .F. ) ;
#9048 = FACE_BOUND ( 'NONE', #10031, .T. ) ;
#9049 = CARTESIAN_POINT ( 'NONE',  ( -17.58178100985202619, -9.533151461302367125, 6.788986777570709563 ) ) ;
#9050 = AXIS2_PLACEMENT_3D ( 'NONE', #23555, #2201, #30738 ) ;
#9051 = EDGE_CURVE ( 'NONE', #14360, #28559, #9700, .T. ) ;
#9052 = CARTESIAN_POINT ( 'NONE',  ( -23.59263552078000359, 12.85968412197262545, 48.13036513616685141 ) ) ;
#9053 = CARTESIAN_POINT ( 'NONE',  ( 19.77267785325472005, 3.123260753354262231, 18.34969686940296185 ) ) ;
#9054 = ORIENTED_EDGE ( 'NONE', *, *, #28685, .T. ) ;
#9055 = CARTESIAN_POINT ( 'NONE',  ( -19.78525473782456956, 3.044038662852082133, 20.19668224736330941 ) ) ;
#9056 = LINE ( 'NONE', #16841, #21203 ) ;
#9057 = CARTESIAN_POINT ( 'NONE',  ( -15.84987138805249707, 12.22653209092614901, 7.280727868105637768 ) ) ;
#9058 = CARTESIAN_POINT ( 'NONE',  ( 4.866781629985560187, 19.41732998781225916, 18.44527579819791185 ) ) ;
#9059 = EDGE_LOOP ( 'NONE', ( #12103, #14009, #4559, #5815 ) ) ;
#9060 = VERTEX_POINT ( 'NONE', #19376 ) ;
#9061 = DIRECTION ( 'NONE',  ( -1.000000000000000000, 0.000000000000000000, -0.000000000000000000 ) ) ;
#9062 = CARTESIAN_POINT ( 'NONE',  ( 10.58819075804203891, -13.39403179698335045, 6.147510495896841398 ) ) ;
#9063 = AXIS2_PLACEMENT_3D ( 'NONE', #12155, #9813, #9197 ) ;
#9064 = CARTESIAN_POINT ( 'NONE',  ( 15.40745978470623356, 12.75221478727799784, 18.72886616302734453 ) ) ;
#9065 = CARTESIAN_POINT ( 'NONE',  ( -5.869193111140220687, 19.13804834536702160, 18.35377592296120497 ) ) ;
#9066 = DIRECTION ( 'NONE',  ( -0.000000000000000000, -0.000000000000000000, -1.000000000000000000 ) ) ;
#9067 = CARTESIAN_POINT ( 'NONE',  ( 35.89043209166288051, 3.548455793333529673, 34.73498294778850948 ) ) ;
#9068 = ITEM_DEFINED_TRANSFORMATION ( 'NONE', 'NONE', #1934,  #7396 ) ;
#9069 = DIRECTION ( 'NONE',  ( -0.000000000000000000, -0.000000000000000000, 1.000000000000000000 ) ) ;
#9070 = EDGE_LOOP ( 'NONE', ( #26684, #11491 ) ) ;
#9071 = VECTOR ( 'NONE', #21301, 1000.000000000000000 ) ;
#9072 = CARTESIAN_POINT ( 'NONE',  ( 1.340340228783115428, -19.95510490826381655, 6.919864475265769421 ) ) ;
#9073 = DIRECTION ( 'NONE',  ( -0.5406408174555974444, -0.8412535328311813165, -0.000000000000000000 ) ) ;
#9074 = CARTESIAN_POINT ( 'NONE',  ( 19.85594780280176153, 2.397944088302077503, 18.72886616302735519 ) ) ;
#9075 = ORIENTED_EDGE ( 'NONE', *, *, #18908, .F. ) ;
#9076 = CARTESIAN_POINT ( 'NONE',  ( -0.1262659238204836554, -8.999114229549588728, -3.621320343559650379 ) ) ;
#9077 = VERTEX_POINT ( 'NONE', #19209 ) ;
#9078 = EDGE_CURVE ( 'NONE', #18371, #28054, #28737, .T. ) ;
#9079 = CARTESIAN_POINT ( 'NONE',  ( 15.84452017418782432, -6.290821626254208709, 5.652605728828373977 ) ) ;
#9080 = FACE_OUTER_BOUND ( 'NONE', #2681, .T. ) ;
#9081 = EDGE_LOOP ( 'NONE', ( #8593, #16506 ) ) ;
#9082 = CARTESIAN_POINT ( 'NONE',  ( 2.498618104684224850, -39.50000000000000000, 27.50000000000000711 ) ) ;
#9083 = CARTESIAN_POINT ( 'NONE',  ( -15.16120755655624741, 17.22181377296911720, -1.500000000000000000 ) ) ;
#9084 = B_SPLINE_CURVE_WITH_KNOTS ( 'NONE', 3,
 ( #4792, #2151, #28367, #6990, #21634, #9485, #7147, #9174, #16658, #2465, #11983, #11527, #21475, #117, #9637, #13863, #14466, #6826 ),
 .UNSPECIFIED., .F., .F.,
 ( 4, 2, 2, 2, 2, 2, 2, 2, 4 ),
 ( 0.000000000000000000, 0.0003967869494442882641, 0.0007935738988885765281, 0.001190360848332864792, 0.001587147797777153056, 0.001983934747221441537, 0.002380721696665729584, 0.002777508646110017632, 0.003174295595554306113 ),
 .UNSPECIFIED. ) ;
#9085 = CARTESIAN_POINT ( 'NONE',  ( -5.729465025513086419E-13, 44.07656359094158915, -16.50000000000000000 ) ) ;
#9086 = DIRECTION ( 'NONE',  ( 0.000000000000000000, 1.000000000000000000, 0.000000000000000000 ) ) ;
#9087 = CARTESIAN_POINT ( 'NONE',  ( -6.116198564155506112, 19.06064343544020190, 20.33971507717571114 ) ) ;
#9088 = DIRECTION ( 'NONE',  ( 0.9594929736144992560, 0.2817325568414232317, 0.000000000000000000 ) ) ;
#9089 = CARTESIAN_POINT ( 'NONE',  ( -16.93068695965898840, 1.913742347956913115, 7.626437579292364433 ) ) ;
#9090 = ORIENTED_EDGE ( 'NONE', *, *, #1998, .T. ) ;
#9091 = DIRECTION ( 'NONE',  ( 0.000000000000000000, 0.000000000000000000, 1.000000000000000000 ) ) ;
#9092 = CARTESIAN_POINT ( 'NONE',  ( -0.1262659238204836554, -8.999114229549588728, 21.50000000000000000 ) ) ;
#9093 = ORIENTED_EDGE ( 'NONE', *, *, #5765, .T. ) ;
#9094 = CARTESIAN_POINT ( 'NONE',  ( 49.99999999999998579, 70.00000000000000000, -75.50000000000001421 ) ) ;
#9095 = CARTESIAN_POINT ( 'NONE',  ( 9.922755320353061848, -13.86203410616582232, 7.652108011868850035 ) ) ;
#9096 = DIRECTION ( 'NONE',  ( 1.000000000000000000, 0.000000000000000000, 0.000000000000000000 ) ) ;
#9097 = DIRECTION ( 'NONE',  ( -0.000000000000000000, 1.132880637372608986E-16, -1.000000000000000000 ) ) ;
#9098 = ORIENTED_EDGE ( 'NONE', *, *, #14936, .F. ) ;
#9099 = CARTESIAN_POINT ( 'NONE',  ( 0.08889351957746016719, -20.00017437841852441, 20.32243167357988511 ) ) ;
#9100 = CIRCLE ( 'NONE', #5113, 10.00000000000000000 ) ;
#9101 = AXIS2_PLACEMENT_3D ( 'NONE', #7363, #11574, #28723 ) ;
#9102 = PLANE ( 'NONE',  #30573 ) ;
#9103 = CARTESIAN_POINT ( 'NONE',  ( 12.79109178508979916, -40.15612306122757502, 29.04694596669003914 ) ) ;
#9105 = CIRCLE ( 'NONE', #13102, 0.7500000000000011102 ) ;
#9104 = CARTESIAN_POINT ( 'NONE',  ( -37.99999999999999289, 70.00000000000000000, -22.50000000000000711 ) ) ;
#9106 = VERTEX_POINT ( 'NONE', #5179 ) ;
#9107 = CARTESIAN_POINT ( 'NONE',  ( 6.437683520590175235, -6.962021646281549181, 21.50000000000000000 ) ) ;
#9108 = CARTESIAN_POINT ( 'NONE',  ( 4.336808689942017736E-16, 42.50000000000000000, -1.500000000000000000 ) ) ;
#9109 = CARTESIAN_POINT ( 'NONE',  ( 0.000000000000000000, -2.435693370351110282E-15, 21.50000000000000355 ) ) ;
#9110 = ORIENTED_EDGE ( 'NONE', *, *, #5206, .F. ) ;
#9111 = DIRECTION ( 'NONE',  ( 0.000000000000000000, 0.000000000000000000, -1.000000000000000000 ) ) ;
#9112 = VERTEX_POINT ( 'NONE', #5958 ) ;
#9113 = CARTESIAN_POINT ( 'NONE',  ( 1.868132521858655084E-15, 50.00000000000000000, -40.00000000000000711 ) ) ;
#9114 = CARTESIAN_POINT ( 'NONE',  ( 30.50257113119999275, -15.54031451041691803, 40.76699977199266556 ) ) ;
#9115 = CARTESIAN_POINT ( 'NONE',  ( -8.074094344234884818E-15, 42.50000000000000000, 19.72227980406325543 ) ) ;
#9116 = ORIENTED_EDGE ( 'NONE', *, *, #29177, .F. ) ;
#9117 = CARTESIAN_POINT ( 'NONE',  ( 23.59223810913926656, 12.86535672232149530, 43.88527982313174647 ) ) ;
#9118 = VECTOR ( 'NONE', #20479, 1000.000000000000000 ) ;
#9119 = CARTESIAN_POINT ( 'NONE',  ( 12.76326067947990772, 11.27442216569340161, 18.54473042795395088 ) ) ;
#9120 = CARTESIAN_POINT ( 'NONE',  ( 0.000000000000000000, 0.000000000000000000, 92.49999999999998579 ) ) ;
#9121 = CARTESIAN_POINT ( 'NONE',  ( -52.16608720827707657, 51.86186943028246787, 97.07879600563551037 ) ) ;
#9122 = VERTEX_POINT ( 'NONE', #5649 ) ;
#9123 = CIRCLE ( 'NONE', #14602, 0.7500000000000006661 ) ;
#9124 = CARTESIAN_POINT ( 'NONE',  ( -9.248129367672078160, -2.094186647214714814, 21.50000000000000000 ) ) ;
#9125 = LINE ( 'NONE', #18645, #22749 ) ;
#9126 = DIRECTION ( 'NONE',  ( -0.000000000000000000, -0.000000000000000000, 1.000000000000000000 ) ) ;
#9127 = FACE_OUTER_BOUND ( 'NONE', #6994, .T. ) ;
#9128 = CARTESIAN_POINT ( 'NONE',  ( 3.113107691796848542, 16.79024107225415463, 19.02573955821369722 ) ) ;
#9129 = DIRECTION ( 'NONE',  ( 0.000000000000000000, 0.000000000000000000, 1.000000000000000000 ) ) ;
#9130 = AXIS2_PLACEMENT_3D ( 'NONE', #21241, #25797, #16576 ) ;
#9131 = DIRECTION ( 'NONE',  ( -1.000000000000000000, 0.000000000000000000, 0.000000000000000000 ) ) ;
#9132 = ORIENTED_EDGE ( 'NONE', *, *, #26718, .T. ) ;
#9133 = ORIENTED_EDGE ( 'NONE', *, *, #26906, .T. ) ;
#9134 = CARTESIAN_POINT ( 'NONE',  ( 8.757878075398934925, -7.394122547431893011, -1.500000000000000000 ) ) ;
#9135 = CARTESIAN_POINT ( 'NONE',  ( -10.11202017158235833, -41.14070756921188377, -1.500000000000000000 ) ) ;
#9136 = CARTESIAN_POINT ( 'NONE',  ( 29.61203839202723032, 15.40012917324034092, -16.55003854064094426 ) ) ;
#9137 = VERTEX_POINT ( 'NONE', #5798 ) ;
#9138 = DIRECTION ( 'NONE',  ( 1.000000000000000000, 0.000000000000000000, 0.000000000000000000 ) ) ;
#9139 = CIRCLE ( 'NONE', #23568, 0.6002263538043648428 ) ;
#9140 = CARTESIAN_POINT ( 'NONE',  ( -6.507434545313869556, 15.78991698230835716, 19.47952243369111258 ) ) ;
#9141 = DIRECTION ( 'NONE',  ( 1.000000000000000000, 0.000000000000000000, 0.000000000000000000 ) ) ;
#9142 = EDGE_CURVE ( 'NONE', #2810, #8702, #21233, .T. ) ;
#9143 = AXIS2_PLACEMENT_3D ( 'NONE', #29157, #12948, #27135 ) ;
#9144 = ORIENTED_EDGE ( 'NONE', *, *, #18908, .T. ) ;
#9145 = AXIS2_PLACEMENT_3D ( 'NONE', #30428, #30720, #2336 ) ;
#9146 = CARTESIAN_POINT ( 'NONE',  ( -19.80175191879421348, 2.933369436805203900, 5.749228751562096562 ) ) ;
#9147 = CARTESIAN_POINT ( 'NONE',  ( -33.14492811172277698, -23.43596546612170073, -6.499905845449016617 ) ) ;
#9148 = ADVANCED_BREP_SHAPE_REPRESENTATION ( '', ( #3175, #7396 ), #9395 ) ;
#9149 = CARTESIAN_POINT ( 'NONE',  ( -11.79670489141087231, -42.17678086688154337, -16.49999999999999645 ) ) ;
#9150 = EDGE_CURVE ( 'NONE', #18592, #6758, #3297, .T. ) ;
#9151 = CARTESIAN_POINT ( 'NONE',  ( -33.32515425934906972, 22.24716177112028248, 34.67326153719451298 ) ) ;
#9152 = EDGE_LOOP ( 'NONE', ( #8970, #16522 ) ) ;
#9153 = DIRECTION ( 'NONE',  ( -0.000000000000000000, 1.000000000000000000, 0.000000000000000000 ) ) ;
#9154 = EDGE_CURVE ( 'NONE', #6837, #24446, #1847, .T. ) ;
#9155 = CARTESIAN_POINT ( 'NONE',  ( 42.49999999999998579, 50.00000000000000000, -87.50000000000000000 ) ) ;
#9156 = CARTESIAN_POINT ( 'NONE',  ( -14.76380438154529173, 13.49194818783279537, 6.144783687052509435 ) ) ;
#9157 = ORIENTED_EDGE ( 'NONE', *, *, #12817, .T. ) ;
#9158 = CARTESIAN_POINT ( 'NONE',  ( 16.87575838019316876, 2.225846228041723940, 19.60617949693493500 ) ) ;
#9159 = DIRECTION ( 'NONE',  ( 0.9898214418809327952, -0.1423148382732850048, 0.000000000000000000 ) ) ;
#9160 = CARTESIAN_POINT ( 'NONE',  ( 9.301547456646380496, 8.591538895647095941, -1.500000000000000000 ) ) ;
#9161 = CARTESIAN_POINT ( 'NONE',  ( 16.70665413472817562, 3.412884783584984927, 7.627891251804737927 ) ) ;
#9162 = EDGE_CURVE ( 'NONE', #3597, #17587, #22605, .T. ) ;
#9163 = ADVANCED_FACE ( 'NONE', ( #8917, #20738 ), #4217, .F. ) ;
#9164 = DIRECTION ( 'NONE',  ( 0.000000000000000000, 1.000000000000000000, 0.000000000000000000 ) ) ;
#9165 = CIRCLE ( 'NONE', #26609, 7.500000000000000000 ) ;
#9166 = CARTESIAN_POINT ( 'NONE',  ( 8.884323311075775109, 1.438332125858202692, 1.500000000000001332 ) ) ;
#9167 = DIRECTION ( 'NONE',  ( 0.000000000000000000, 0.000000000000000000, 1.000000000000000000 ) ) ;
#9168 = ORIENTED_EDGE ( 'NONE', *, *, #13955, .T. ) ;
#9169 = CIRCLE ( 'NONE', #28025, 0.7499999999999997780 ) ;
#9170 = CARTESIAN_POINT ( 'NONE',  ( -6.315055774899184904, 15.86014940733236678, 6.037360021877316463 ) ) ;
#9171 = DIRECTION ( 'NONE',  ( 0.000000000000000000, 0.000000000000000000, 1.000000000000000000 ) ) ;
#9172 = ORIENTED_EDGE ( 'NONE', *, *, #22538, .F. ) ;
#9173 = ORIENTED_EDGE ( 'NONE', *, *, #2724, .F. ) ;
#9174 = CARTESIAN_POINT ( 'NONE',  ( 4.333676792162787450, 19.52490442444424801, 19.08830981656264214 ) ) ;
#9175 = B_SPLINE_CURVE_WITH_KNOTS ( 'NONE', 3,
 ( #2254, #14104, #18806, #16758, #30490, #19252, #26274, #4912, #21592, #226 ),
 .UNSPECIFIED., .F., .F.,
 ( 4, 2, 2, 2, 4 ),
 ( 0.2152766488939568124, 0.2238273688332776123, 0.2394469624395233198, 0.2472567592426461458, 0.2550665560457689995 ),
 .UNSPECIFIED. ) ;
#9176 = ORIENTED_EDGE ( 'NONE', *, *, #25564, .F. ) ;
#9177 = CARTESIAN_POINT ( 'NONE',  ( 25.10445388623454477, -25.60065097860747585, 1.500000000000000000 ) ) ;
#9178 = ADVANCED_FACE ( 'NONE', ( #25450 ), #2318, .T. ) ;
#9179 = DIRECTION ( 'NONE',  ( -0.9547931052914339078, -0.2972711322815266843, 0.000000000000000000 ) ) ;
#9180 = ORIENTED_EDGE ( 'NONE', *, *, #19676, .T. ) ;
#9181 = EDGE_CURVE ( 'NONE', #4023, #20845, #15779, .T. ) ;
#9182 = CARTESIAN_POINT ( 'NONE',  ( -15.66719571743413120, 12.43196305300236659, 18.47531940416306284 ) ) ;
#9183 = LINE ( 'NONE', #18244, #15474 ) ;
#9184 = ORIENTED_EDGE ( 'NONE', *, *, #30735, .T. ) ;
#9185 = LINE ( 'NONE', #14160, #28755 ) ;
#9186 = AXIS2_PLACEMENT_3D ( 'NONE', #27420, #18204, #6347 ) ;
#9187 = ORIENTED_EDGE ( 'NONE', *, *, #14304, .F. ) ;
#9188 = CARTESIAN_POINT ( 'NONE',  ( -4.163336342344337027E-14, 1.387778780781445676E-14, -1.500000000000000000 ) ) ;
#9189 = ADVANCED_FACE ( 'NONE', ( #16222 ), #23231, .F. ) ;
#9190 = ORIENTED_EDGE ( 'NONE', *, *, #414, .F. ) ;
#9191 = ORIENTED_EDGE ( 'NONE', *, *, #18906, .F. ) ;
#9192 = EDGE_CURVE ( 'NONE', #2008, #30491, #15768, .T. ) ;
#9193 = ADVANCED_FACE ( 'NONE', ( #10787 ), #30424, .T. ) ;
#9194 = DIRECTION ( 'NONE',  ( -0.000000000000000000, -0.000000000000000000, -1.000000000000000000 ) ) ;
#9195 = CARTESIAN_POINT ( 'NONE',  ( -17.98413878735053117, -8.751483025296225904, 5.652912763329821288 ) ) ;
#9196 = EDGE_CURVE ( 'NONE', #26952, #12085, #20306, .T. ) ;
#9197 = DIRECTION ( 'NONE',  ( 1.000000000000000000, 0.000000000000000000, 0.000000000000000000 ) ) ;
#9198 = CARTESIAN_POINT ( 'NONE',  ( 0.000000000000000000, 1.699320956058915452E-16, -1.500000000000001776 ) ) ;
#9199 = CARTESIAN_POINT ( 'NONE',  ( 16.84421249428843126, 2.491431357970652183, 18.63641924841378028 ) ) ;
#9200 = ORIENTED_EDGE ( 'NONE', *, *, #9245, .T. ) ;
#9201 = CARTESIAN_POINT ( 'NONE',  ( 15.79886199502269761, -6.395730384537285040, 5.651989602109219746 ) ) ;
#9202 = CARTESIAN_POINT ( 'NONE',  ( -13.38159811071079552, 10.55828946507379307, 5.652196082364323360 ) ) ;
#9203 = LINE ( 'NONE', #28227, #4823 ) ;
#9204 = ORIENTED_EDGE ( 'NONE', *, *, #455, .T. ) ;
#9205 = ORIENTED_EDGE ( 'NONE', *, *, #20023, .F. ) ;
#9206 = VECTOR ( 'NONE', #17193, 1000.000000000000000 ) ;
#9207 = CARTESIAN_POINT ( 'NONE',  ( -4.776122516674677878E-15, -42.50000000000000000, 1.500000000000001332 ) ) ;
#9208 = DIRECTION ( 'NONE',  ( 0.000000000000000000, -1.000000000000000000, 0.000000000000000000 ) ) ;
#9209 = CARTESIAN_POINT ( 'NONE',  ( 15.28831480992544201, 12.89481865072259303, 20.14992337338001960 ) ) ;
#9210 = CARTESIAN_POINT ( 'NONE',  ( -5.141690706682822132, 7.488956955540452931, 13.22130136205108819 ) ) ;
#9211 = CARTESIAN_POINT ( 'NONE',  ( -25.47847050916411504, 26.57182937991348481, 26.54355021145562787 ) ) ;
#9212 = CARTESIAN_POINT ( 'NONE',  ( -15.45157863257330533, 35.69925327167838702, 27.50000000000000711 ) ) ;
#9213 = EDGE_CURVE ( 'NONE', #13938, #11031, #19776, .T. ) ;
#9214 = DIRECTION ( 'NONE',  ( 1.000000000000000000, 0.000000000000000000, 0.000000000000000000 ) ) ;
#9215 = VERTEX_POINT ( 'NONE', #27793 ) ;
#9216 = ADVANCED_FACE ( 'NONE', ( #1440, #4072 ), #6708, .F. ) ;
#9217 = CARTESIAN_POINT ( 'NONE',  ( -19.93005420669540584, 1.873390432278239315, 7.441806358946449151 ) ) ;
#9218 = DIRECTION ( 'NONE',  ( 0.000000000000000000, 0.000000000000000000, 1.000000000000000000 ) ) ;
#9219 = ADVANCED_FACE ( 'NONE', ( #4372 ), #13455, .T. ) ;
#9220 = CARTESIAN_POINT ( 'NONE',  ( 19.86476987328768118, 2.322391784566624207, 18.84056766331482180 ) ) ;
#9221 = EDGE_LOOP ( 'NONE', ( #20868, #29223, #1693, #10615 ) ) ;
#9222 = CARTESIAN_POINT ( 'NONE',  ( 3.221450758838616757, -1.621276839356792454, 1.500000000000000000 ) ) ;
#9223 = ORIENTED_EDGE ( 'NONE', *, *, #22532, .F. ) ;
#9224 = CARTESIAN_POINT ( 'NONE',  ( 18.68320837179354044, -7.186693706611501753, 6.131018562779544823 ) ) ;
#9225 = CARTESIAN_POINT ( 'NONE',  ( -5.729465025513086419E-13, 44.07656359094158915, -16.50000000000000000 ) ) ;
#9226 = VERTEX_POINT ( 'NONE', #27480 ) ;
#9227 = CARTESIAN_POINT ( 'NONE',  ( 35.56916886408897938, 6.214436617257074857, 27.50000000000000355 ) ) ;
#9228 = CIRCLE ( 'NONE', #10227, 0.6002263538043630664 ) ;
#9229 = CARTESIAN_POINT ( 'NONE',  ( -7.500000000000000000, 0.000000000000000000, 63.50000000000000000 ) ) ;
#9230 = B_SPLINE_CURVE_WITH_KNOTS ( 'NONE', 3,
 ( #10769, #22305, #8279, #948, #5634, #20281, #17638, #15130, #27308, #5475, #14976, #15434, #5938, #22455 ),
 .UNSPECIFIED., .F., .F.,
 ( 4, 2, 2, 2, 2, 2, 4 ),
 ( 2.111077618454142872E-07, 0.0004668847438969844690, 0.0009335583800321235227, 0.001400232016167262577, 0.001866905652302401630, 0.002800252924572683641, 0.003733600196842966085 ),
 .UNSPECIFIED. ) ;
#9231 = FACE_OUTER_BOUND ( 'NONE', #8727, .T. ) ;
#9232 = DIRECTION ( 'NONE',  ( -0.000000000000000000, 0.000000000000000000, 1.000000000000000000 ) ) ;
#9233 = CARTESIAN_POINT ( 'NONE',  ( -6.889674169070711507, 18.79461648230378401, 19.03762469184452755 ) ) ;
#9234 = DIRECTION ( 'NONE',  ( -0.000000000000000000, -0.000000000000000000, 1.000000000000000000 ) ) ;
#9235 = DIRECTION ( 'NONE',  ( -0.000000000000000000, -0.000000000000000000, 1.000000000000000000 ) ) ;
#9236 = ORIENTED_EDGE ( 'NONE', *, *, #11998, .T. ) ;
#9237 = CARTESIAN_POINT ( 'NONE',  ( 49.99999999999998579, 50.00000000000000000, 62.49999999999999289 ) ) ;
#9238 = CARTESIAN_POINT ( 'NONE',  ( -37.99999999999999289, 209.2686044187655909, -87.50000000000000000 ) ) ;
#9239 = AXIS2_PLACEMENT_3D ( 'NONE', #24926, #5899, #29609 ) ;
#9240 = CYLINDRICAL_SURFACE ( 'NONE', #28725, 15.00000000000000000 ) ;
#9241 = EDGE_LOOP ( 'NONE', ( #21328, #9561, #13650, #21153 ) ) ;
#9242 = CYLINDRICAL_SURFACE ( 'NONE', #19522, 0.7500000000000006661 ) ;
#9243 = LINE ( 'NONE', #25783, #6317 ) ;
#9244 = CARTESIAN_POINT ( 'NONE',  ( -20.00000000000004263, 1.387778780781445676E-14, 1.500000000000000000 ) ) ;
#9245 = EDGE_CURVE ( 'NONE', #24522, #27352, #15611, .T. ) ;
#9246 = CARTESIAN_POINT ( 'NONE',  ( -31.18700685316050780, 26.11823559932051353, -1.500000000000000000 ) ) ;
#9247 = EDGE_CURVE ( 'NONE', #23441, #23754, #3934, .T. ) ;
#9248 = LINE ( 'NONE', #14390, #20080 ) ;
#9249 = VERTEX_POINT ( 'NONE', #23079 ) ;
#9250 = DIRECTION ( 'NONE',  ( -0.000000000000000000, -0.000000000000000000, -1.000000000000000000 ) ) ;
#9251 = CIRCLE ( 'NONE', #18232, 9.084132297865673777 ) ;
#9252 = DIRECTION ( 'NONE',  ( -0.000000000000000000, -0.000000000000000000, 1.000000000000000000 ) ) ;
#9253 = CARTESIAN_POINT ( 'NONE',  ( 33.47974733229618494, -16.94066219419696750, 37.49999999993178079 ) ) ;
#9254 = DIRECTION ( 'NONE',  ( -0.000000000000000000, -0.000000000000000000, 1.000000000000000000 ) ) ;
#9255 = EDGE_LOOP ( 'NONE', ( #17915, #25671, #16416, #8067 ) ) ;
#9256 = VECTOR ( 'NONE', #30244, 1000.000000000000000 ) ;
#9257 = CARTESIAN_POINT ( 'NONE',  ( -13.71336669122886853, 10.15199454957378578, 5.759928666072749337 ) ) ;
#9258 = CARTESIAN_POINT ( 'NONE',  ( -10.11202017158235833, -41.14070756921188377, -1.500000000000000000 ) ) ;
#9259 = LINE ( 'NONE', #18627, #6471 ) ;
#9260 = EDGE_LOOP ( 'NONE', ( #10277, #2016, #7450, #26967, #7699, #24982, #6335 ) ) ;
#9261 = ORIENTED_EDGE ( 'NONE', *, *, #12043, .F. ) ;
#9262 = CARTESIAN_POINT ( 'NONE',  ( -31.79204601741444236, -14.90874471747207686, 35.64345580000767200 ) ) ;
#9263 = CIRCLE ( 'NONE', #12252, 4.999999999999997335 ) ;
#9264 = EDGE_LOOP ( 'NONE', ( #1708, #12108, #30352, #16185 ) ) ;
#9265 = CARTESIAN_POINT ( 'NONE',  ( -0.08542884365699984772, -20.01766063302414622, 18.44501272782439827 ) ) ;
#9266 = CARTESIAN_POINT ( 'NONE',  ( -7.692543755867215616, -15.24678548464671479, 6.892848776733236704 ) ) ;
#9267 = DIRECTION ( 'NONE',  ( 0.000000000000000000, 0.000000000000000000, 1.000000000000000000 ) ) ;
#9268 = CARTESIAN_POINT ( 'NONE',  ( 1.082887659287351312, -19.98847979319446821, 18.64703902303423178 ) ) ;
#9269 = ORIENTED_EDGE ( 'NONE', *, *, #3767, .T. ) ;
#9270 = TOROIDAL_SURFACE ( 'NONE', #7317, 17.00000000000000000, 3.000000000000000000 ) ;
#9271 = CARTESIAN_POINT ( 'NONE',  ( 16.56213591300094379, 4.162091996070008904, 6.392658652357122939 ) ) ;
#9272 = CARTESIAN_POINT ( 'NONE',  ( -32.60829997825918980, -13.18983524832147936, 39.84356070656660620 ) ) ;
#9273 = CARTESIAN_POINT ( 'NONE',  ( -2.662523238938575343, -12.47340865698848056, 24.50000000000000000 ) ) ;
#9274 = VERTEX_POINT ( 'NONE', #22787 ) ;
#9275 = CIRCLE ( 'NONE', #15754, 0.7500000000000006661 ) ;
#9276 = CARTESIAN_POINT ( 'NONE',  ( -15.22000698778095540, -7.667275871987174973, 18.34727598691068096 ) ) ;
#9277 = DIRECTION ( 'NONE',  ( 0.9096319953545183301, 0.4154150130018864906, 0.000000000000000000 ) ) ;
#9278 = DIRECTION ( 'NONE',  ( 0.000000000000000000, 1.000000000000000000, 0.000000000000000000 ) ) ;
#9279 = DIRECTION ( 'NONE',  ( -0.000000000000000000, -0.000000000000000000, -1.000000000000000000 ) ) ;
#9280 = DIRECTION ( 'NONE',  ( 0.000000000000000000, 0.000000000000000000, -1.000000000000000000 ) ) ;
#9281 = CARTESIAN_POINT ( 'NONE',  ( -4.163336342344337027E-14, 1.387778780781445676E-14, 34.49999999999999289 ) ) ;
#9282 = CARTESIAN_POINT ( 'NONE',  ( -11.40980092660686829, 6.310027164379044429, 24.50000000000000000 ) ) ;
#9283 = AXIS2_PLACEMENT_3D ( 'NONE', #26467, #10230, #2455 ) ;
#9284 = EDGE_LOOP ( 'NONE', ( #18288, #22447, #27001 ) ) ;
#9285 = VERTEX_POINT ( 'NONE', #22937 ) ;
#9286 = DIRECTION ( 'NONE',  ( -0.000000000000000000, -0.000000000000000000, -1.000000000000000000 ) ) ;
#9287 = PRESENTATION_LAYER_ASSIGNMENT (  '', '', ( #18749 ) ) ;
#9288 = CARTESIAN_POINT ( 'NONE',  ( -31.18700685316100163, -26.11823559932341610, -1.500000000000000000 ) ) ;
#9289 = DIRECTION ( 'NONE',  ( 0.000000000000000000, -1.132880637372608986E-16, 1.000000000000000000 ) ) ;
#9290 = EDGE_LOOP ( 'NONE', ( #22075, #18250, #20237, #22957 ) ) ;
#9291 = CARTESIAN_POINT ( 'NONE',  ( 18.01689225005682005, -8.724154469992756233, 19.96783386855779341 ) ) ;
#9292 = CARTESIAN_POINT ( 'NONE',  ( 4.994189150946234612, 16.27260345083324822, 6.864725433338323413 ) ) ;
#9293 = CIRCLE ( 'NONE', #4810, 6.000000000000005329 ) ;
#9294 = EDGE_LOOP ( 'NONE', ( #11241, #9324, #7427, #17158 ) ) ;
#9295 = CIRCLE ( 'NONE', #12289, 0.7500000000000006661 ) ;
#9296 = CARTESIAN_POINT ( 'NONE',  ( 12.25849595087226973, 11.84990609407551077, 7.643931100913408550 ) ) ;
#9297 = CIRCLE ( 'NONE', #14772, 10.00000000000000178 ) ;
#9298 = CARTESIAN_POINT ( 'NONE',  ( -16.40045772880338859, -40.31754624252415198, -16.50000000000000000 ) ) ;
#9299 = CARTESIAN_POINT ( 'NONE',  ( -14.12911150912318803, 34.74147843573596361, 37.49999999997172040 ) ) ;
#9300 = ORIENTED_EDGE ( 'NONE', *, *, #16599, .T. ) ;
#9301 = PLANE ( 'NONE',  #30289 ) ;
#9302 = PLANE ( 'NONE',  #13559 ) ;
#9303 = LINE ( 'NONE', #13546, #4859 ) ;
#9304 = AXIS2_PLACEMENT_3D ( 'NONE', #5990, #22367, #10362 ) ;
#9305 = ORIENTED_EDGE ( 'NONE', *, *, #2427, .T. ) ;
#9306 =( BOUNDED_CURVE ( )  B_SPLINE_CURVE ( 3, ( #15060, #3689, #1041, #27234 ),
 .UNSPECIFIED., .F., .T. ) 
 B_SPLINE_CURVE_WITH_KNOTS ( ( 4, 4 ),
 ( 0.8137667884748612801, 2.327825865114931947 ),
 .UNSPECIFIED. ) 
 CURVE ( )  GEOMETRIC_REPRESENTATION_ITEM ( )  RATIONAL_B_SPLINE_CURVE ( ( 1.000000000000000000, 0.8179194830933627092, 0.8179194830933627092, 1.000000000000000000 ) ) 
 REPRESENTATION_ITEM ( '' )  );
#9307 = LINE ( 'NONE', #2601, #11333 ) ;
#9308 = CARTESIAN_POINT ( 'NONE',  ( 16.76361099856289982, 3.068725842123817493, 18.34727598691067740 ) ) ;
#9309 =( LENGTH_UNIT ( ) NAMED_UNIT ( * ) SI_UNIT ( .MILLI., .METRE. ) );
#9310 = CARTESIAN_POINT ( 'NONE',  ( 0.1262659238204208167, 8.999114229549594057, -3.621320343559650379 ) ) ;
#9311 = CARTESIAN_POINT ( 'NONE',  ( 19.76130184095197606, 3.194145055459935101, 7.652108011868850035 ) ) ;
#9312 = AXIS2_PLACEMENT_3D ( 'NONE', #20611, #22223, #22386 ) ;
#9313 = DIRECTION ( 'NONE',  ( -1.000000000000000000, 0.000000000000000000, 0.000000000000000000 ) ) ;
#9314 = CIRCLE ( 'NONE', #25746, 1.447898107987198646 ) ;
#9315 = DIRECTION ( 'NONE',  ( 0.4495526574063634095, -0.8932538319083086487, 0.000000000000000000 ) ) ;
#9316 = CARTESIAN_POINT ( 'NONE',  ( -6.187077094091591789, 11.47693674426096955, 1.500000000000001332 ) ) ;
#9317 = CARTESIAN_POINT ( 'NONE',  ( -8.999114229549592281, 0.1262659238205133538, -3.621320343559650379 ) ) ;
#9318 = ORIENTED_EDGE ( 'NONE', *, *, #4812, .T. ) ;
#9319 = CIRCLE ( 'NONE', #25751, 1.447898107987198646 ) ;
#9320 = CARTESIAN_POINT ( 'NONE',  ( 10.56600709331201315, -13.41035981659391751, 19.89182036555910571 ) ) ;
#9321 = B_SPLINE_CURVE_WITH_KNOTS ( 'NONE', 3,
 ( #11723, #21214, #30744, #26218, #14203, #23712, #16869, #2362, #11889, #21384, #19051, #28567, #14372, #23880, #2523, #12038 ),
 .UNSPECIFIED., .F., .F.,
 ( 4, 2, 2, 2, 2, 2, 2, 4 ),
 ( 0.4999999999999997224, 0.6250000000000018874, 0.6875000000000026645, 0.7187500000000028866, 0.7500000000000031086, 0.8125000000000019984, 0.8750000000000006661, 1.000000000000000000 ),
 .UNSPECIFIED. ) ;
#9322 = AXIS2_PLACEMENT_3D ( 'NONE', #15729, #15899, #22593 ) ;
#9323 = DIRECTION ( 'NONE',  ( -1.000000000000000000, 0.000000000000000000, 0.000000000000000000 ) ) ;
#9324 = ORIENTED_EDGE ( 'NONE', *, *, #24003, .T. ) ;
#9325 = VERTEX_POINT ( 'NONE', #1589 ) ;
#9326 = CARTESIAN_POINT ( 'NONE',  ( -15.85201432996392867, 12.19518096057846179, 6.037995405461184184 ) ) ;
#9327 = ADVANCED_FACE ( 'NONE', ( #10955 ), #11099, .F. ) ;
#9328 = AXIS2_PLACEMENT_3D ( 'NONE', #1757, #8776, #18605 ) ;
#9329 = ORIENTED_EDGE ( 'NONE', *, *, #26648, .F. ) ;
#9330 = AXIS2_PLACEMENT_3D ( 'NONE', #19667, #29189, #17338 ) ;
#9331 = CARTESIAN_POINT ( 'NONE',  ( -4.163336342344337027E-14, 1.387778780781445676E-14, 62.49999999999999289 ) ) ;
#9332 = CIRCLE ( 'NONE', #26272, 28.20443790117963800 ) ;
#9333 = EDGE_LOOP ( 'NONE', ( #19781, #6206 ) ) ;
#9334 = DIRECTION ( 'NONE',  ( 0.000000000000000000, 0.000000000000000000, 1.000000000000000000 ) ) ;
#9335 = VECTOR ( 'NONE', #10763, 1000.000000000000000 ) ;
#9336 = DIRECTION ( 'NONE',  ( 0.06975647374412530244, 0.000000000000000000, -0.9975640502598241977 ) ) ;
#9337 = ORIENTED_EDGE ( 'NONE', *, *, #18628, .F. ) ;
#9338 = AXIS2_PLACEMENT_3D ( 'NONE', #26140, #29104, #4937 ) ;
#9339 = DIRECTION ( 'NONE',  ( -0.000000000000000000, -0.000000000000000000, 1.000000000000000000 ) ) ;
#9340 = ORIENTED_EDGE ( 'NONE', *, *, #15862, .F. ) ;
#9341 = AXIS2_PLACEMENT_3D ( 'NONE', #6128, #18298, #8944 ) ;
#9342 = VERTEX_POINT ( 'NONE', #4987 ) ;
#9343 = ORIENTED_EDGE ( 'NONE', *, *, #20455, .F. ) ;
#9344 = VECTOR ( 'NONE', #16477, 1000.000000000000114 ) ;
#9345 = LINE ( 'NONE', #16206, #17127 ) ;
#9346 = B_SPLINE_CURVE_WITH_KNOTS ( 'NONE', 3,
 ( #2097, #4594, #11620, #27699, #3993, #23000, #6325, #20819, #30341, #21111, #14096, #13961, #4284, #4139, #30631, #15840, #25820, #13813, #9276, #25516 ),
 .UNSPECIFIED., .F., .F.,
 ( 4, 2, 2, 2, 2, 2, 2, 2, 2, 4 ),
 ( 0.000000000000000000, 0.06250000000000184575, 0.1250000000000036915, 0.1875000000000055511, 0.2187500000000056621, 0.2500000000000057732, 0.3125000000000043299, 0.3750000000000028866, 0.4375000000000013878, 0.4999999999999999445 ),
 .UNSPECIFIED. ) ;
#9347 = CARTESIAN_POINT ( 'NONE',  ( 39.99999999999998579, 80.00000000000001421, 22.49999999999999289 ) ) ;
#9348 = AXIS2_PLACEMENT_3D ( 'NONE', #23390, #1723, #25736 ) ;
#9349 = ADVANCED_FACE ( 'NONE', ( #19338 ), #21188, .F. ) ;
#9350 = CARTESIAN_POINT ( 'NONE',  ( -22.58267429318971864, 26.57182937991348481, 24.50000000000000000 ) ) ;
#9351 = DIRECTION ( 'NONE',  ( 0.000000000000000000, 0.000000000000000000, 1.000000000000000000 ) ) ;
#9352 = LINE ( 'NONE', #23386, #12888 ) ;
#9353 = ADVANCED_FACE ( 'NONE', ( #16688 ), #3937, .F. ) ;
#9354 = ORIENTED_EDGE ( 'NONE', *, *, #23258, .F. ) ;
#9355 = CARTESIAN_POINT ( 'NONE',  ( -19.74686063004096326, 3.283826233409515183, 18.71435384576123440 ) ) ;
#9356 = CARTESIAN_POINT ( 'NONE',  ( 9.494436928264741837, -38.10466040143803212, 34.50000000000000000 ) ) ;
#9357 = AXIS2_PLACEMENT_3D ( 'NONE', #17246, #22070, #864 ) ;
#9358 = DIRECTION ( 'NONE',  ( 0.000000000000000000, 0.000000000000000000, 1.000000000000000000 ) ) ;
#9359 = CARTESIAN_POINT ( 'NONE',  ( 0.000000000000000000, 0.000000000000000000, 1.500000000000001332 ) ) ;
#9360 = VERTEX_POINT ( 'NONE', #26360 ) ;
#9361 = ORIENTED_EDGE ( 'NONE', *, *, #29930, .T. ) ;
#9362 = CIRCLE ( 'NONE', #23722, 0.7500000000000006661 ) ;
#9363 = DIRECTION ( 'NONE',  ( 1.000000000000000000, 0.000000000000000000, -0.000000000000000000 ) ) ;
#9364 = ADVANCED_FACE ( 'NONE', ( #16529 ), #9824, .F. ) ;
#9365 = CARTESIAN_POINT ( 'NONE',  ( 7.067645071111839705, -41.84023411754124311, 20.26730379392047610 ) ) ;
#9366 = CARTESIAN_POINT ( 'NONE',  ( -5.512483845762027102, 16.12829592175436133, 18.34777357837151968 ) ) ;
#9367 = DIRECTION ( 'NONE',  ( 0.000000000000000000, 0.000000000000000000, -1.000000000000000000 ) ) ;
#9368 = CARTESIAN_POINT ( 'NONE',  ( -35.89597485276235034, 3.063380141105419341, 27.49999999999999645 ) ) ;
#9369 = CARTESIAN_POINT ( 'NONE',  ( -5.849168665050585858, 19.12602664087013693, 5.651480102388686255 ) ) ;
#9370 = CIRCLE ( 'NONE', #4379, 6.000000000000005329 ) ;
#9371 = EDGE_CURVE ( 'NONE', #15207, #3753, #8868, .T. ) ;
#9372 = ORIENTED_EDGE ( 'NONE', *, *, #9162, .T. ) ;
#9373 = CIRCLE ( 'NONE', #24832, 5.000000000000004441 ) ;
#9374 = CARTESIAN_POINT ( 'NONE',  ( -19.95549607358725908, 1.576375212833063921, 6.233981582756856987 ) ) ;
#9375 = ADVANCED_FACE ( 'NONE', ( #23686 ), #6863, .T. ) ;
#9376 = AXIS2_PLACEMENT_3D ( 'NONE', #20102, #12940, #3415 ) ;
#9377 = CARTESIAN_POINT ( 'NONE',  ( 14.18307372309187109, 14.10107868313152224, 19.21940439362673914 ) ) ;
#9378 = CARTESIAN_POINT ( 'NONE',  ( -26.80246859415415273, 7.028748154183637631, -6.500000000000000888 ) ) ;
#9379 = ORIENTED_EDGE ( 'NONE', *, *, #29953, .T. ) ;
#9380 = ADVANCED_FACE ( 'NONE', ( #16988 ), #21664, .T. ) ;
#9381 = CARTESIAN_POINT ( 'NONE',  ( 8.480328572437745294, -4.608906612435629491, 1.500000000000001332 ) ) ;
#9382 = ORIENTED_EDGE ( 'NONE', *, *, #13036, .F. ) ;
#9383 = DIRECTION ( 'NONE',  ( 0.8412535328311813165, -0.5406408174555974444, 0.000000000000000000 ) ) ;
#9384 = AXIS2_PLACEMENT_3D ( 'NONE', #20361, #6010, #3677 ) ;
#9385 = CARTESIAN_POINT ( 'NONE',  ( -4.102102735472399786, 8.549050687778207092, 1.500000000000001332 ) ) ;
#9386 = ORIENTED_EDGE ( 'NONE', *, *, #26582, .T. ) ;
#9387 = CARTESIAN_POINT ( 'NONE',  ( 21.64339062281885973, -31.56738424159307499, 27.50000000000000711 ) ) ;
#9388 = DIRECTION ( 'NONE',  ( -0.000000000000000000, -0.000000000000000000, -1.000000000000000000 ) ) ;
#9389 = DIRECTION ( 'NONE',  ( 1.000000000000000000, 0.000000000000000000, 4.565061778886335400E-17 ) ) ;
#9390 = CARTESIAN_POINT ( 'NONE',  ( 33.78553947564427773, -24.40792753551981775, -16.50000000000000000 ) ) ;
#9391 = DIRECTION ( 'NONE',  ( -0.000000000000000000, -0.000000000000000000, -1.000000000000000000 ) ) ;
#9392 = LINE ( 'NONE', #19367, #11821 ) ;
#9393 = CARTESIAN_POINT ( 'NONE',  ( -31.57687401261850013, 15.10620312102103568, 39.99603010801635605 ) ) ;
#9394 = ADVANCED_FACE ( 'NONE', ( #2032, #11556 ), #25253, .F. ) ;
#9395 =( GEOMETRIC_REPRESENTATION_CONTEXT ( 3 ) GLOBAL_UNCERTAINTY_ASSIGNED_CONTEXT ( ( #24168 ) ) GLOBAL_UNIT_ASSIGNED_CONTEXT ( ( #1361, #1054, #17726 ) ) REPRESENTATION_CONTEXT ( 'NONE', 'WORKASPACE' ) );
#9396 = ORIENTED_EDGE ( 'NONE', *, *, #25397, .T. ) ;
#9397 = EDGE_CURVE ( 'NONE', #6758, #17047, #24282, .T. ) ;
#9398 = CARTESIAN_POINT ( 'NONE',  ( 15.38611090871063070, -7.279566334535291894, 6.519181285484530797 ) ) ;
#9399 = VECTOR ( 'NONE', #12233, 1000.000000000000000 ) ;
#9400 = AXIS2_PLACEMENT_3D ( 'NONE', #7598, #7917, #12743 ) ;
#9401 = CARTESIAN_POINT ( 'NONE',  ( -39.83602371821034183, 11.57901747687032490, -19.50000000000000355 ) ) ;
#9402 = CIRCLE ( 'NONE', #13405, 0.7499999999999997780 ) ;
#9403 = CARTESIAN_POINT ( 'NONE',  ( 49.99999999999998579, -50.00000000000000000, 12.49999999999999112 ) ) ;
#9404 = EDGE_CURVE ( 'NONE', #4276, #3697, #23539, .T. ) ;
#9405 = VERTEX_POINT ( 'NONE', #11701 ) ;
#9406 = B_SPLINE_CURVE_WITH_KNOTS ( 'NONE', 3,
 ( #28159, #11951, #30640, #28328, #20829, #30803, #14255, #21442, #1812, #25525 ),
 .UNSPECIFIED., .F., .F.,
 ( 4, 3, 3, 4 ),
 ( 3.702578198638058010E-17, 0.005033946524314943105, 0.01006789357361646473, 0.01510156516273209251 ),
 .UNSPECIFIED. ) ;
#9407 = DIRECTION ( 'NONE',  ( 1.000000000000000000, 0.000000000000000000, 0.000000000000000000 ) ) ;
#9408 = DIRECTION ( 'NONE',  ( 1.000000000000000000, 0.000000000000000000, 0.000000000000000000 ) ) ;
#9409 = ADVANCED_FACE ( 'NONE', ( #14343 ), #21359, .F. ) ;
#9410 = CARTESIAN_POINT ( 'NONE',  ( 37.98493438989863336, -11.12428508576153341, -1.500000000000000000 ) ) ;
#9411 = FACE_OUTER_BOUND ( 'NONE', #27646, .T. ) ;
#9412 = CIRCLE ( 'NONE', #5914, 20.00000000000000000 ) ;
#9413 = ORIENTED_EDGE ( 'NONE', *, *, #4641, .T. ) ;
#9414 = CARTESIAN_POINT ( 'NONE',  ( 0.2207535014603100587, -19.99921160563567568, 20.34789198813115618 ) ) ;
#9415 = CARTESIAN_POINT ( 'NONE',  ( -7.663215745754974328, 3.196529495465474380, -3.621320343559650379 ) ) ;
#9416 = CARTESIAN_POINT ( 'NONE',  ( 37.42187249122466142, 2.505710565345217855, 37.50000000001962519 ) ) ;
#9417 = EDGE_CURVE ( 'NONE', #13589, #12796, #147, .T. ) ;
#9418 = CARTESIAN_POINT ( 'NONE',  ( -5.687793815610304726, 6.974883619896852238, -3.621320343559650379 ) ) ;
#9419 = ORIENTED_EDGE ( 'NONE', *, *, #17393, .F. ) ;
#9420 = CARTESIAN_POINT ( 'NONE',  ( -13.38160118231794549, 10.55829203257430038, 5.652196082368482699 ) ) ;
#9421 = FACE_OUTER_BOUND ( 'NONE', #13709, .T. ) ;
#9422 = DIRECTION ( 'NONE',  ( -0.000000000000000000, 1.132880637372608986E-16, -1.000000000000000000 ) ) ;
#9423 = VERTEX_POINT ( 'NONE', #29001 ) ;
#9424 = ORIENTED_EDGE ( 'NONE', *, *, #27118, .F. ) ;
#9425 = LINE ( 'NONE', #7701, #14244 ) ;
#9426 = AXIS2_PLACEMENT_3D ( 'NONE', #4911, #2421, #5375 ) ;
#9427 = VERTEX_POINT ( 'NONE', #12637 ) ;
#9428 = VERTEX_POINT ( 'NONE', #5614 ) ;
#9429 = CARTESIAN_POINT ( 'NONE',  ( 0.2775250113394547857, -20.01590685155468563, 18.34969686940295830 ) ) ;
#9430 = EDGE_CURVE ( 'NONE', #5262, #10442, #8357, .T. ) ;
#9431 = EDGE_CURVE ( 'NONE', #1292, #8044, #2343, .T. ) ;
#9432 = CARTESIAN_POINT ( 'NONE',  ( 4.967306913969569138, 16.28142803849144826, 19.66962785902261146 ) ) ;
#9433 = AXIS2_PLACEMENT_3D ( 'NONE', #18549, #25567, #28053 ) ;
#9434 = CARTESIAN_POINT ( 'NONE',  ( 1.350727940147186334, -19.97202376558939818, 19.14333282897057842 ) ) ;
#9435 = ORIENTED_EDGE ( 'NONE', *, *, #27469, .F. ) ;
#9436 = DIRECTION ( 'NONE',  ( 0.000000000000000000, 0.000000000000000000, 1.000000000000000000 ) ) ;
#9437 = CARTESIAN_POINT ( 'NONE',  ( 1.224646799147357990E-15, -10.00000000000006395, 157.4999999999999716 ) ) ;
#9438 = CARTESIAN_POINT ( 'NONE',  ( 26.36764545593177544, -31.31467416275353344, 1.500000000000000000 ) ) ;
#9439 = CARTESIAN_POINT ( 'NONE',  ( -6.812559277181930106, 5.881244434206302607, 21.50000000000000000 ) ) ;
#9440 = ORIENTED_EDGE ( 'NONE', *, *, #9575, .F. ) ;
#9441 = AXIS2_PLACEMENT_3D ( 'NONE', #9188, #18248, #28208 ) ;
#9442 = B_SPLINE_CURVE_WITH_KNOTS ( 'NONE', 3,
 ( #3604, #25588, #18431, #1111, #6410, #4065 ),
 .UNSPECIFIED., .F., .F.,
 ( 4, 2, 4 ),
 ( 0.001913784325927354304, 0.008754285094829554470, 0.01400530011240105378 ),
 .UNSPECIFIED. ) ;
#9443 = CARTESIAN_POINT ( 'NONE',  ( -14.92167319134950887, -8.273715889511855437, 5.810767894563978686 ) ) ;
#9444 = DIRECTION ( 'NONE',  ( -0.000000000000000000, -0.000000000000000000, 1.000000000000000000 ) ) ;
#9445 = DIRECTION ( 'NONE',  ( -0.000000000000000000, -0.000000000000000000, -1.000000000000000000 ) ) ;
#9446 = CARTESIAN_POINT ( 'NONE',  ( -23.07950435457408034, -11.39185397358521001, 49.26234194702450964 ) ) ;
#9447 = CARTESIAN_POINT ( 'NONE',  ( -18.10021843967229316, -8.508777197197408881, 20.34789198813115974 ) ) ;
#9448 = CARTESIAN_POINT ( 'NONE',  ( -15.21426671708081457, -7.679208962302482178, 20.34789198813115263 ) ) ;
#9449 = CARTESIAN_POINT ( 'NONE',  ( 33.56327786402390245, -10.34181101807379477, 35.63689980405263924 ) ) ;
#9450 = VERTEX_POINT ( 'NONE', #15250 ) ;
#9451 = ORIENTED_EDGE ( 'NONE', *, *, #21750, .T. ) ;
#9452 = LINE ( 'NONE', #26122, #15436 ) ;
#9453 = CARTESIAN_POINT ( 'NONE',  ( -2.552544030762004645, -42.50000000000000000, -1.500000000000000000 ) ) ;
#9454 = DIRECTION ( 'NONE',  ( -0.000000000000000000, -0.000000000000000000, -1.000000000000000000 ) ) ;
#9455 = CARTESIAN_POINT ( 'NONE',  ( 11.62196639741666004, -16.27693748946513708, 18.54958172136248606 ) ) ;
#9456 = ORIENTED_EDGE ( 'NONE', *, *, #22321, .F. ) ;
#9457 = DIRECTION ( 'NONE',  ( 0.000000000000000000, 0.000000000000000000, 1.000000000000000000 ) ) ;
#9458 = AXIS2_PLACEMENT_3D ( 'NONE', #7219, #19540, #14402 ) ;
#9459 = CARTESIAN_POINT ( 'NONE',  ( -6.476765594713846497, 15.80122980073391936, 19.08844262864050023 ) ) ;
#9460 = CARTESIAN_POINT ( 'NONE',  ( 4.467866064779363988, 16.43745301482979926, 5.749228751562096562 ) ) ;
#9461 = VERTEX_POINT ( 'NONE', #1084 ) ;
#9462 = CARTESIAN_POINT ( 'NONE',  ( 0.3518703668723790479, -19.99690444156084013, 7.652108011868850035 ) ) ;
#9463 = AXIS2_PLACEMENT_3D ( 'NONE', #30046, #15540, #18197 ) ;
#9464 = CARTESIAN_POINT ( 'NONE',  ( -11.64054540341807353, 16.26338533980436907, 24.50000000000000000 ) ) ;
#9465 = CARTESIAN_POINT ( 'NONE',  ( -17.50822840077841747, 37.98520514636454948, 34.52714558546959012 ) ) ;
#9466 = ORIENTED_EDGE ( 'NONE', *, *, #14365, .F. ) ;
#9467 = FACE_OUTER_BOUND ( 'NONE', #14620, .T. ) ;
#9468 = DIRECTION ( 'NONE',  ( -1.000000000000000000, 0.000000000000000000, 0.000000000000000000 ) ) ;
#9469 = CARTESIAN_POINT ( 'NONE',  ( 24.03057240117691862, 26.57182937991349903, 1.500000000000000000 ) ) ;
#9470 = EDGE_CURVE ( 'NONE', #15693, #2154, #10124, .T. ) ;
#9471 = ORIENTED_EDGE ( 'NONE', *, *, #21960, .F. ) ;
#9472 = CARTESIAN_POINT ( 'NONE',  ( -18.29014699721056303, -8.135908015825709327, 7.500898271101006820 ) ) ;
#9473 = CARTESIAN_POINT ( 'NONE',  ( 9.755064781586030520, 13.32952022457704544, 1.500000000000000000 ) ) ;
#9474 = CARTESIAN_POINT ( 'NONE',  ( -0.1864951924744762124, -20.01724188655222747, 5.796888747622817029 ) ) ;
#9475 = AXIS2_PLACEMENT_3D ( 'NONE', #24519, #12689, #29844 ) ;
#9476 = DIRECTION ( 'NONE',  ( -0.000000000000000000, -0.000000000000000000, 1.000000000000000000 ) ) ;
#9477 = DIRECTION ( 'NONE',  ( -0.000000000000000000, 0.000000000000000000, 1.000000000000000000 ) ) ;
#9478 = CARTESIAN_POINT ( 'NONE',  ( -19.93005420669540584, 1.873390432278237983, 20.13759033520874908 ) ) ;
#9479 = DIRECTION ( 'NONE',  ( 1.000000000000000000, 0.000000000000000000, 0.000000000000000000 ) ) ;
#9480 = ORIENTED_EDGE ( 'NONE', *, *, #21985, .T. ) ;
#9481 = DIRECTION ( 'NONE',  ( -0.2817325568414296710, 0.9594929736144973687, 0.000000000000000000 ) ) ;
#9482 = CARTESIAN_POINT ( 'NONE',  ( 8.159193615868399974, -3.993622308618911099, 13.22130136205108819 ) ) ;
#9483 = VERTEX_POINT ( 'NONE', #7961 ) ;
#9484 = ORIENTED_EDGE ( 'NONE', *, *, #22202, .T. ) ;
#9485 = CARTESIAN_POINT ( 'NONE',  ( 4.507962051892417499, 19.48556068265256513, 18.73377938172347612 ) ) ;
#9486 = CARTESIAN_POINT ( 'NONE',  ( 0.000000000000000000, 0.000000000000000000, 0.000000000000000000 ) ) ;
#9487 = EDGE_LOOP ( 'NONE', ( #4656, #23510, #4493, #3129 ) ) ;
#9488 = CARTESIAN_POINT ( 'NONE',  ( -27.03074382657074537, -6.449748410230988327, -16.55003854064094426 ) ) ;
#9489 = CARTESIAN_POINT ( 'NONE',  ( -4.163336342344337027E-14, -1.387778780781445676E-14, -1.500000000000000000 ) ) ;
#9490 = EDGE_LOOP ( 'NONE', ( #3561, #355, #20410, #19809 ) ) ;
#9491 = CARTESIAN_POINT ( 'NONE',  ( 18.73355814148580833, -7.053980495653730642, 19.36813350477385143 ) ) ;
#9492 = CARTESIAN_POINT ( 'NONE',  ( 19.57830992477560272, 4.170884463584000557, 19.58863275299554019 ) ) ;
#9493 = CIRCLE ( 'NONE', #532, 4.999999999999997335 ) ;
#9494 = DIRECTION ( 'NONE',  ( -1.000000000000000000, 0.000000000000000000, 0.000000000000000000 ) ) ;
#9495 = ORIENTED_EDGE ( 'NONE', *, *, #214, .F. ) ;
#9496 = CARTESIAN_POINT ( 'NONE',  ( 15.44332723073812907, -7.163653983989226148, 18.83976166372256245 ) ) ;
#9497 = ORIENTED_EDGE ( 'NONE', *, *, #23837, .T. ) ;
#9498 = EDGE_LOOP ( 'NONE', ( #18079, #8690, #23484, #21796 ) ) ;
#9499 = LINE ( 'NONE', #23381, #5114 ) ;
#9500 = CARTESIAN_POINT ( 'NONE',  ( -0.2303554413151768232, -17.01973167556347377, 19.41069149716888020 ) ) ;
#9501 = CARTESIAN_POINT ( 'NONE',  ( 1.709141304117140825, -16.98942507101831367, 6.233981582756856987 ) ) ;
#9502 = CARTESIAN_POINT ( 'NONE',  ( -23.27838111883973227, 36.10018642694448943, -16.50000600000000262 ) ) ;
#9503 = LINE ( 'NONE', #28534, #10852 ) ;
#9504 = CARTESIAN_POINT ( 'NONE',  ( 16.75466217413941905, 3.123260753354262231, 18.34969686940296185 ) ) ;
#9505 = ORIENTED_EDGE ( 'NONE', *, *, #2510, .T. ) ;
#9506 = CIRCLE ( 'NONE', #50, 29.99999999999928946 ) ;
#9507 = CARTESIAN_POINT ( 'NONE',  ( 9.326937650406421199, -14.24778824691897761, 7.429667576816606278 ) ) ;
#9508 = DIRECTION ( 'NONE',  ( -0.000000000000000000, 1.132880637372608986E-16, -1.000000000000000000 ) ) ;
#9509 = AXIS2_PLACEMENT_3D ( 'NONE', #12312, #15240, #26656 ) ;
#9510 = CARTESIAN_POINT ( 'NONE',  ( 25.23756106473024730, -11.43858098102957577, -11.49999999999999645 ) ) ;
#9511 = ORIENTED_EDGE ( 'NONE', *, *, #10956, .T. ) ;
#9512 = ORIENTED_EDGE ( 'NONE', *, *, #865, .F. ) ;
#9513 = CARTESIAN_POINT ( 'NONE',  ( 0.000000000000000000, 42.50000000000000000, 1.500000000000001332 ) ) ;
#9514 = CARTESIAN_POINT ( 'NONE',  ( -9.958038337755702685, 17.34466697471556529, 24.50000000000000000 ) ) ;
#9515 = CARTESIAN_POINT ( 'NONE',  ( 5.687793815610356241, -6.974883619896809606, 21.50000000000000000 ) ) ;
#9516 = CARTESIAN_POINT ( 'NONE',  ( 52.16608720827707657, -51.86186943028246787, 57.49999999999999289 ) ) ;
#9517 = DIRECTION ( 'NONE',  ( 0.000000000000000000, -0.000000000000000000, -1.000000000000000000 ) ) ;
#9518 = CARTESIAN_POINT ( 'NONE',  ( 28.37932450449293853, 10.51822134874671022, -1.500000000000000000 ) ) ;
#9519 = CARTESIAN_POINT ( 'NONE',  ( 0.5612050131688016696, 4.355613924421565919, -9.000000000000003553 ) ) ;
#9520 = ORIENTED_EDGE ( 'NONE', *, *, #16757, .T. ) ;
#9521 = CARTESIAN_POINT ( 'NONE',  ( -8.824744466605359605, -8.513189541288717521, 1.500000000000001332 ) ) ;
#9522 = CARTESIAN_POINT ( 'NONE',  ( 8.860628911697515875, 8.184276679720483116, 1.500000000000000000 ) ) ;
#9523 = CARTESIAN_POINT ( 'NONE',  ( -0.1262659238204836554, -8.999114229549588728, 21.50000000000000000 ) ) ;
#9524 = ORIENTED_EDGE ( 'NONE', *, *, #12819, .F. ) ;
#9525 = CARTESIAN_POINT ( 'NONE',  ( 12.24063095261064404, 4.490763173670002217, 1.500000000000001332 ) ) ;
#9526 = ORIENTED_EDGE ( 'NONE', *, *, #3733, .F. ) ;
#9527 = LINE ( 'NONE', #4092, #30367 ) ;
#9528 = CIRCLE ( 'NONE', #11036, 15.00000000000000000 ) ;
#9529 = CARTESIAN_POINT ( 'NONE',  ( -8.809276947023224835, 43.02645599243116692, -16.50000000000000000 ) ) ;
#9530 = EDGE_CURVE ( 'NONE', #10675, #19313, #28546, .T. ) ;
#9531 = EDGE_LOOP ( 'NONE', ( #27762, #2614, #14193, #10948 ) ) ;
#9532 = CARTESIAN_POINT ( 'NONE',  ( 15.46896137236496216, 35.67159706264204999, 27.50000000000000711 ) ) ;
#9533 = CARTESIAN_POINT ( 'NONE',  ( 8.752233641273210907, 49.22975159878511420, -42.80828904653874645 ) ) ;
#9534 = EDGE_CURVE ( 'NONE', #30279, #25497, #29769, .T. ) ;
#9535 = CARTESIAN_POINT ( 'NONE',  ( -7.075845757273814415E-16, 65.00000000000000000, 15.49999999999998757 ) ) ;
#9536 = VECTOR ( 'NONE', #1161, 1000.000000000000000 ) ;
#9537 = CYLINDRICAL_SURFACE ( 'NONE', #6334, 9.084132297865673777 ) ;
#9538 = CARTESIAN_POINT ( 'NONE',  ( 17.22181377297005866, 14.41708049311048789, -1.500000000000000000 ) ) ;
#9539 = CARTESIAN_POINT ( 'NONE',  ( 10.88769261259305132, -16.77715788799338981, 20.32243167357988867 ) ) ;
#9540 = VERTEX_POINT ( 'NONE', #7790 ) ;
#9541 = AXIS2_PLACEMENT_3D ( 'NONE', #13998, #9164, #14139 ) ;
#9542 = LINE ( 'NONE', #16715, #16288 ) ;
#9543 = EDGE_CURVE ( 'NONE', #29733, #23863, #5854, .T. ) ;
#9544 = CARTESIAN_POINT ( 'NONE',  ( 5.374868878254059013, -44.10336124695543703, -19.50000000000000355 ) ) ;
#9545 = LINE ( 'NONE', #497, #24235 ) ;
#9546 = ORIENTED_EDGE ( 'NONE', *, *, #5401, .F. ) ;
#9547 = DIRECTION ( 'NONE',  ( 1.000000000000000000, 0.000000000000000000, 0.000000000000000000 ) ) ;
#9548 = EDGE_CURVE ( 'NONE', #228, #9013, #24320, .T. ) ;
#9549 = CARTESIAN_POINT ( 'NONE',  ( -15.01939917408024527, -8.081071717223313300, 20.29915277494337644 ) ) ;
#9550 = CARTESIAN_POINT ( 'NONE',  ( -9.131494062835631809, -2.555255504830934221, 21.50000000000000000 ) ) ;
#9551 = DIRECTION ( 'NONE',  ( 0.000000000000000000, 0.000000000000000000, 1.000000000000000000 ) ) ;
#9552 = VECTOR ( 'NONE', #17161, 1000.000000000000000 ) ;
#9553 = CARTESIAN_POINT ( 'NONE',  ( 42.49999999999998579, 50.00000000000000000, 52.07879600563550326 ) ) ;
#9554 = ORIENTED_EDGE ( 'NONE', *, *, #29982, .T. ) ;
#9555 = CYLINDRICAL_SURFACE ( 'NONE', #17385, 9.482273699623480212 ) ;
#9556 = CARTESIAN_POINT ( 'NONE',  ( -17.84153987719600920, 14.83584055149731284, -1.500000000000000000 ) ) ;
#9557 = CARTESIAN_POINT ( 'NONE',  ( 35.66659450230903161, 17.24746242023032394, 34.79915034189033918 ) ) ;
#9558 = DIRECTION ( 'NONE',  ( -0.000000000000000000, 0.000000000000000000, 1.000000000000000000 ) ) ;
#9559 = ORIENTED_EDGE ( 'NONE', *, *, #22685, .F. ) ;
#9560 = LINE ( 'NONE', #4263, #25072 ) ;
#9561 = ORIENTED_EDGE ( 'NONE', *, *, #14735, .T. ) ;
#9562 = CARTESIAN_POINT ( 'NONE',  ( 23.96732207938043402, -33.98584080152387088, -1.500000000000000000 ) ) ;
#9563 = DIRECTION ( 'NONE',  ( 1.000000000000000000, 0.000000000000000000, 0.000000000000000000 ) ) ;
#9564 = ORIENTED_EDGE ( 'NONE', *, *, #1798, .T. ) ;
#9565 = EDGE_CURVE ( 'NONE', #22425, #4276, #26701, .T. ) ;
#9566 = ORIENTED_EDGE ( 'NONE', *, *, #1395, .F. ) ;
#9567 = ADVANCED_FACE ( 'NONE', ( #24155 ), #2803, .F. ) ;
#9568 = DIRECTION ( 'NONE',  ( 1.000000000000000000, 0.000000000000000000, 0.000000000000000000 ) ) ;
#9569 = CIRCLE ( 'NONE', #12566, 9.482273699623480212 ) ;
#9570 = ORIENTED_EDGE ( 'NONE', *, *, #3310, .T. ) ;
#9571 = ADVANCED_FACE ( 'NONE', ( #24624 ), #468, .F. ) ;
#9572 = ORIENTED_EDGE ( 'NONE', *, *, #2848, .T. ) ;
#9573 = VERTEX_POINT ( 'NONE', #12486 ) ;
#9574 = CARTESIAN_POINT ( 'NONE',  ( 0.1486850733125462121, -17.02875910996195685, 18.55820869691756769 ) ) ;
#9575 = EDGE_CURVE ( 'NONE', #28301, #29154, #22764, .T. ) ;
#9576 = CARTESIAN_POINT ( 'NONE',  ( -10.24254388992508602, -17.19919274694469280, 7.603368798681074736 ) ) ;
#9577 = CIRCLE ( 'NONE', #9034, 2.898871837527149609 ) ;
#9578 = CARTESIAN_POINT ( 'NONE',  ( -5.881244434206279514, -6.812559277181949646, 21.50000000000000000 ) ) ;
#9579 = CARTESIAN_POINT ( 'NONE',  ( 1.111517487559788409, -17.01912455222412035, 20.29915277494337644 ) ) ;
#9580 = VERTEX_POINT ( 'NONE', #25095 ) ;
#9581 = EDGE_CURVE ( 'NONE', #24152, #11965, #30073, .T. ) ;
#9582 = CARTESIAN_POINT ( 'NONE',  ( 0.000000000000000000, 0.000000000000000000, 92.49999999999998579 ) ) ;
#9583 = FACE_OUTER_BOUND ( 'NONE', #8089, .T. ) ;
#9584 = CARTESIAN_POINT ( 'NONE',  ( 11.77016209912415690, 12.36695356451125249, 19.89182036555910571 ) ) ;
#9585 = CARTESIAN_POINT ( 'NONE',  ( 32.98805937973593672, -80.00000000000000000, 18.00000000000000000 ) ) ;
#9586 = ADVANCED_FACE ( 'NONE', ( #27753 ), #25414, .F. ) ;
#9587 = EDGE_LOOP ( 'NONE', ( #13873, #19029, #14727, #5676 ) ) ;
#9588 = PLANE ( 'NONE',  #29330 ) ;
#9589 = CARTESIAN_POINT ( 'NONE',  ( 3.896869771148438577, -16.82098518409776489, -0.6213203435596476032 ) ) ;
#9590 = CYLINDRICAL_SURFACE ( 'NONE', #15831, 7.500000000000000000 ) ;
#9591 = VECTOR ( 'NONE', #27381, 1000.000000000000114 ) ;
#9592 = CARTESIAN_POINT ( 'NONE',  ( -19.91153203745396993, 1.881428233485404666, 7.454606537396340826 ) ) ;
#9593 = DIRECTION ( 'NONE',  ( -1.000000000000000000, -0.000000000000000000, -0.000000000000000000 ) ) ;
#9594 = AXIS2_PLACEMENT_3D ( 'NONE', #17575, #8072, #5716 ) ;
#9595 = CARTESIAN_POINT ( 'NONE',  ( -15.19605639364643324, -7.717080560943919032, 18.34969686940295830 ) ) ;
#9596 = B_SPLINE_CURVE_WITH_KNOTS ( 'NONE', 3,
 ( #2410, #7403, #21727, #11936, #9727, #12081 ),
 .UNSPECIFIED., .F., .F.,
 ( 4, 2, 4 ),
 ( 2.108697328626194806E-07, 0.0003800081648695531069, 0.0007598054600062436074 ),
 .UNSPECIFIED. ) ;
#9597 = DIRECTION ( 'NONE',  ( -0.6707505147970090897, -0.7416830501633074890, 0.000000000000000000 ) ) ;
#9598 = VERTEX_POINT ( 'NONE', #29939 ) ;
#9599 = ORIENTED_EDGE ( 'NONE', *, *, #11109, .F. ) ;
#9600 =( NAMED_UNIT ( * ) SI_UNIT ( $, .STERADIAN. ) SOLID_ANGLE_UNIT ( ) );
#9601 = LINE ( 'NONE', #20970, #29095 ) ;
#9602 = EDGE_CURVE ( 'NONE', #20079, #25485, #11813, .T. ) ;
#9603 = CARTESIAN_POINT ( 'NONE',  ( -24.44496207165490276, 7.595930209050158588, 49.40206402021040333 ) ) ;
#9604 = CARTESIAN_POINT ( 'NONE',  ( 11.33091155972627462, -16.48105488812121067, 18.37545668562167123 ) ) ;
#9605 = ORIENTED_EDGE ( 'NONE', *, *, #21926, .T. ) ;
#9606 = PRODUCT_CONTEXT ( 'NONE', #26509, 'mechanical' ) ;
#9607 = CARTESIAN_POINT ( 'NONE',  ( 17.99235278053350839, -8.774603096602955787, 18.80699882434806369 ) ) ;
#9608 = CARTESIAN_POINT ( 'NONE',  ( 5.303645853345009265, 19.30241027580586177, 7.652108011868850035 ) ) ;
#9609 = EDGE_CURVE ( 'NONE', #15949, #14253, #15799, .T. ) ;
#9610 = ORIENTED_EDGE ( 'NONE', *, *, #6527, .T. ) ;
#9611 = CARTESIAN_POINT ( 'NONE',  ( 5.413395986729065079, 19.27227163692344902, 20.34789198813115263 ) ) ;
#9612 = EDGE_CURVE ( 'NONE', #7103, #479, #10323, .T. ) ;
#9613 = CARTESIAN_POINT ( 'NONE',  ( 11.81884104268967839, 12.31686436340674895, 7.280727868105637768 ) ) ;
#9614 = CARTESIAN_POINT ( 'NONE',  ( -11.40980092660686829, 6.310027164379044429, 1.500000000000001332 ) ) ;
#9615 = CARTESIAN_POINT ( 'NONE',  ( -21.33648105846517495, 35.69619395329613099, 29.46852146853187193 ) ) ;
#9616 = ORIENTED_EDGE ( 'NONE', *, *, #17172, .F. ) ;
#9617 = DIRECTION ( 'NONE',  ( 1.000000000000000000, 0.000000000000000000, 0.000000000000000000 ) ) ;
#9618 = AXIS2_PLACEMENT_3D ( 'NONE', #22727, #10897, #20403 ) ;
#9619 = CARTESIAN_POINT ( 'NONE',  ( 33.21383100183306425, 9.208170138131603011, 36.29077426434711384 ) ) ;
#9620 = CARTESIAN_POINT ( 'NONE',  ( 22.43462709106480091, 36.72607276382733943, -16.50000000000000000 ) ) ;
#9621 = VERTEX_POINT ( 'NONE', #5552 ) ;
#9622 = CARTESIAN_POINT ( 'NONE',  ( -15.56928374346769850, -6.880100827600172941, 6.420335371522007506 ) ) ;
#9623 = CARTESIAN_POINT ( 'NONE',  ( 33.56327786402390245, -10.34181101807379655, -16.55003854064094426 ) ) ;
#9624 = CARTESIAN_POINT ( 'NONE',  ( 14.18379620663259288, 14.10035196125401313, 6.788986777570696241 ) ) ;
#9625 = CARTESIAN_POINT ( 'NONE',  ( -0.4401303402703778955, -20.01320326077421186, 6.018569869498933578 ) ) ;
#9626 = APPLICATION_CONTEXT ( 'automotive_design' ) ;
#9627 = CARTESIAN_POINT ( 'NONE',  ( 22.95669091611928181, 27.54300778121952575, -1.500000000000000000 ) ) ;
#9628 = FACE_BOUND ( 'NONE', #16581, .T. ) ;
#9629 = CARTESIAN_POINT ( 'NONE',  ( -19.94392260440443110, 1.716525891962610961, 19.97651184436794125 ) ) ;
#9630 = DIRECTION ( 'NONE',  ( 0.000000000000000000, 0.000000000000000000, 1.000000000000000000 ) ) ;
#9631 = EDGE_LOOP ( 'NONE', ( #30102, #30694, #23612, #22766 ) ) ;
#9632 = CARTESIAN_POINT ( 'NONE',  ( 11.29839223038184848, -16.52442514205455737, 20.32367522806703874 ) ) ;
#9633 = CARTESIAN_POINT ( 'NONE',  ( 9.056208293496307959, -2.810445847081888715, 13.00000000000000178 ) ) ;
#9634 = ORIENTED_EDGE ( 'NONE', *, *, #7969, .T. ) ;
#9635 = ORIENTED_EDGE ( 'NONE', *, *, #22101, .F. ) ;
#9636 = AXIS2_PLACEMENT_3D ( 'NONE', #18722, #302, #19339 ) ;
#9637 = CARTESIAN_POINT ( 'NONE',  ( 4.805983152666241764, 19.41435796516023515, 20.22386025856690139 ) ) ;
#9638 = EDGE_CURVE ( 'NONE', #24939, #12796, #29105, .T. ) ;
#9639 = CARTESIAN_POINT ( 'NONE',  ( -13.44924491617056539, 48.15781802575228454, -61.66015067657107807 ) ) ;
#9640 =( LENGTH_UNIT ( ) NAMED_UNIT ( * ) SI_UNIT ( .MILLI., .METRE. ) );
#9641 = ORIENTED_EDGE ( 'NONE', *, *, #4026, .F. ) ;
#9642 = EDGE_CURVE ( 'NONE', #25532, #9360, #20774, .T. ) ;
#9643 = CARTESIAN_POINT ( 'NONE',  ( -30.33183837007556249, 13.53414739637282516, -16.55003854064094426 ) ) ;
#9644 = ORIENTED_EDGE ( 'NONE', *, *, #20586, .F. ) ;
#9645 = CYLINDRICAL_SURFACE ( 'NONE', #5328, 20.00000000000000000 ) ;
#9646 = CARTESIAN_POINT ( 'NONE',  ( -15.51115086193519055, 12.62612245312785575, 20.32200205377524327 ) ) ;
#9647 = CARTESIAN_POINT ( 'NONE',  ( 0.000000000000000000, 0.000000000000000000, 21.50000000000000000 ) ) ;
#9648 = ORIENTED_EDGE ( 'NONE', *, *, #6693, .F. ) ;
#9649 = CYLINDRICAL_SURFACE ( 'NONE', #5354, 20.00000000000000355 ) ;
#9650 = ORIENTED_EDGE ( 'NONE', *, *, #20841, .F. ) ;
#9651 = VECTOR ( 'NONE', #18070, 1000.000000000000000 ) ;
#9652 = ORIENTED_EDGE ( 'NONE', *, *, #5062, .T. ) ;
#9653 = CIRCLE ( 'NONE', #10655, 9.482273699623480212 ) ;
#9654 = FACE_OUTER_BOUND ( 'NONE', #30462, .T. ) ;
#9655 = CARTESIAN_POINT ( 'NONE',  ( -14.78913018809137192, 13.49064936509565982, 19.87181966307587544 ) ) ;
#9656 = CARTESIAN_POINT ( 'NONE',  ( -10.05618025891932277, -17.30842068227157071, 18.50655187082627862 ) ) ;
#9657 = DIRECTION ( 'NONE',  ( -0.000000000000000000, 1.000000000000000000, -0.000000000000000000 ) ) ;
#9658 = CARTESIAN_POINT ( 'NONE',  ( 1.043163081497040290, -17.02278858106077308, 20.34789198813115263 ) ) ;
#9659 = CARTESIAN_POINT ( 'NONE',  ( 16.80805182381674712, 2.764250834391621225, 18.44501272782439827 ) ) ;
#9660 = EDGE_LOOP ( 'NONE', ( #19748, #13634, #3232, #15468 ) ) ;
#9661 = FACE_OUTER_BOUND ( 'NONE', #6682, .T. ) ;
#9662 = DIRECTION ( 'NONE',  ( 0.4495526574063634095, 0.8932538319083086487, 0.000000000000000000 ) ) ;
#9663 = CARTESIAN_POINT ( 'NONE',  ( -15.63429437150528756, 12.50148542865848356, 7.559636331181775581 ) ) ;
#9664 = CARTESIAN_POINT ( 'NONE',  ( -2.703030265324078307, -12.75514121382991384, 1.500000000000001332 ) ) ;
#9665 = EDGE_LOOP ( 'NONE', ( #16469, #8914 ) ) ;
#9666 = VERTEX_POINT ( 'NONE', #5406 ) ;
#9667 = DIRECTION ( 'NONE',  ( 0.000000000000000000, 0.000000000000000000, -1.000000000000000000 ) ) ;
#9668 = DIRECTION ( 'NONE',  ( -0.000000000000000000, -0.000000000000000000, -1.000000000000000000 ) ) ;
#9669 = CARTESIAN_POINT ( 'NONE',  ( -40.05104235265675783, -2.353288714459718989, -6.500000000000000888 ) ) ;
#9670 = PRODUCT_DEFINITION_SHAPE ( 'NONE', 'NONE',  #30864 ) ;
#9671 = CARTESIAN_POINT ( 'NONE',  ( 18.44250036706183593, -7.738792361249054785, 18.37545668562167123 ) ) ;
#9672 = DIRECTION ( 'NONE',  ( 0.000000000000000000, 1.000000000000000000, 0.000000000000000000 ) ) ;
#9673 = DIRECTION ( 'NONE',  ( -0.000000000000000000, 1.000000000000000000, 0.000000000000000000 ) ) ;
#9674 = CARTESIAN_POINT ( 'NONE',  ( -5.723804255145592101, 19.16384832744316213, 5.676722608126686609 ) ) ;
#9675 = ORIENTED_EDGE ( 'NONE', *, *, #8275, .T. ) ;
#9676 = CARTESIAN_POINT ( 'NONE',  ( -33.53465676216265479, -14.39878183770549214, 34.49999999999997868 ) ) ;
#9677 = CARTESIAN_POINT ( 'NONE',  ( -67.00000000000000000, -50.00000000000000000, 62.49999999999999289 ) ) ;
#9678 = ORIENTED_EDGE ( 'NONE', *, *, #13983, .F. ) ;
#9679 = DIRECTION ( 'NONE',  ( -0.000000000000000000, -0.000000000000000000, 1.000000000000000000 ) ) ;
#9680 = ORIENTED_EDGE ( 'NONE', *, *, #6561, .F. ) ;
#9681 = CARTESIAN_POINT ( 'NONE',  ( 18.65245237681030588, -7.265846841151808455, 7.280727868105637768 ) ) ;
#9682 = DIRECTION ( 'NONE',  ( -1.000000000000000000, 0.000000000000000000, 0.000000000000000000 ) ) ;
#9683 = CARTESIAN_POINT ( 'NONE',  ( -2.616297575292053423, 43.98845571999485315, -16.50000000000000000 ) ) ;
#9684 = ORIENTED_EDGE ( 'NONE', *, *, #20469, .T. ) ;
#9685 = CARTESIAN_POINT ( 'NONE',  ( 34.30746359002519341, 12.22650445617505355, 27.50000000000000711 ) ) ;
#9686 = DIRECTION ( 'NONE',  ( 1.000000000000000000, 0.000000000000000000, 0.000000000000000000 ) ) ;
#9687 = CARTESIAN_POINT ( 'NONE',  ( -1.438332125858111432, 8.884323311075791096, 21.50000000000000000 ) ) ;
#9688 = DIRECTION ( 'NONE',  ( -1.000000000000000000, 0.000000000000000000, 0.000000000000000000 ) ) ;
#9689 = CIRCLE ( 'NONE', #27140, 0.7500000000000006661 ) ;
#9690 = FACE_BOUND ( 'NONE', #28964, .T. ) ;
#9691 = CARTESIAN_POINT ( 'NONE',  ( -22.94541271838176755, -35.03073867844241818, -6.500000000000000888 ) ) ;
#9692 = DIRECTION ( 'NONE',  ( -0.000000000000000000, -0.000000000000000000, 1.000000000000000000 ) ) ;
#9693 = ORIENTED_EDGE ( 'NONE', *, *, #4662, .T. ) ;
#9694 = CARTESIAN_POINT ( 'NONE',  ( 19.54426622602689179, 37.07991288358296345, -1.499999999999999778 ) ) ;
#9695 = CARTESIAN_POINT ( 'NONE',  ( -35.76344986165604212, -22.29344514668547461, -19.50000000000000355 ) ) ;
#9696 = DIRECTION ( 'NONE',  ( -1.000000000000000000, -0.000000000000000000, -0.000000000000000000 ) ) ;
#9697 = ADVANCED_FACE ( 'NONE', ( #19737 ), #24893, .F. ) ;
#9698 = ORIENTED_EDGE ( 'NONE', *, *, #8042, .T. ) ;
#9699 = LINE ( 'NONE', #12049, #8585 ) ;
#9700 = LINE ( 'NONE', #9860, #9811 ) ;
#9701 = DIRECTION ( 'NONE',  ( 0.000000000000000000, 0.000000000000000000, 1.000000000000000000 ) ) ;
#9702 = PLANE ( 'NONE',  #4295 ) ;
#9703 = CARTESIAN_POINT ( 'NONE',  ( 31.18700685317242716, 26.11823559933198879, -1.500000000000000000 ) ) ;
#9704 = ORIENTED_EDGE ( 'NONE', *, *, #17818, .T. ) ;
#9705 = CARTESIAN_POINT ( 'NONE',  ( 27.20641111072948348, 30.48549905497583978, 34.52784944976806258 ) ) ;
#9706 = EDGE_CURVE ( 'NONE', #22374, #15944, #7346, .T. ) ;
#9707 = DIRECTION ( 'NONE',  ( 0.9096319953545185522, -0.4154150130018860465, 0.000000000000000000 ) ) ;
#9708 = ORIENTED_EDGE ( 'NONE', *, *, #25458, .F. ) ;
#9709 = CARTESIAN_POINT ( 'NONE',  ( 14.41708049311143469, -17.22181377297010130, 1.500000000000000000 ) ) ;
#9710 = EDGE_LOOP ( 'NONE', ( #23807, #18422, #23240, #19469 ) ) ;
#9711 = CARTESIAN_POINT ( 'NONE',  ( 8.430595340551260364, -4.340342926364983533, 21.50000000000000000 ) ) ;
#9712 = CARTESIAN_POINT ( 'NONE',  ( 11.82521593960875173, 5.400395169024529984, 1.500000000000001332 ) ) ;
#9713 = ORIENTED_EDGE ( 'NONE', *, *, #9031, .F. ) ;
#9714 = VECTOR ( 'NONE', #1128, 1000.000000000000000 ) ;
#9715 = ORIENTED_EDGE ( 'NONE', *, *, #7117, .T. ) ;
#9716 = CARTESIAN_POINT ( 'NONE',  ( -9.819201815016004531, -17.42389611976319941, 7.272192800924331735 ) ) ;
#9717 = ORIENTED_EDGE ( 'NONE', *, *, #16616, .T. ) ;
#9718 = ORIENTED_EDGE ( 'NONE', *, *, #26543, .F. ) ;
#9719 = ORIENTED_EDGE ( 'NONE', *, *, #19268, .T. ) ;
#9720 = CARTESIAN_POINT ( 'NONE',  ( 0.000000000000000000, 9.084132297865672001, 21.50000000000000355 ) ) ;
#9721 = ADVANCED_FACE ( 'NONE', ( #555 ), #3210, .T. ) ;
#9722 = CARTESIAN_POINT ( 'NONE',  ( -9.846411740200883500, -17.42855948811278566, 7.280727868105637768 ) ) ;
#9723 = CARTESIAN_POINT ( 'NONE',  ( -9.471281197126605989, -0.4564504349074042788, 1.500000000000001332 ) ) ;
#9724 = CARTESIAN_POINT ( 'NONE',  ( 1.224038712338731072, -19.98030457043141084, 18.82680253904184298 ) ) ;
#9725 = ORIENTED_EDGE ( 'NONE', *, *, #14601, .F. ) ;
#9726 = CARTESIAN_POINT ( 'NONE',  ( -15.57266529552203416, -38.96488032230103471, -1.500000000000000000 ) ) ;
#9727 = CARTESIAN_POINT ( 'NONE',  ( -23.07950435457408034, -11.39185397358521001, 45.01970125990521865 ) ) ;
#9728 = CARTESIAN_POINT ( 'NONE',  ( 14.66647055262615318, 13.62412221374329846, 18.39992786714538298 ) ) ;
#9729 = DIRECTION ( 'NONE',  ( 0.000000000000000000, 0.000000000000000000, 1.000000000000000000 ) ) ;
#9730 = EDGE_LOOP ( 'NONE', ( #26321, #1823, #10106, #23870 ) ) ;
#9731 = EDGE_CURVE ( 'NONE', #5896, #6583, #3273, .T. ) ;
#9732 = DIRECTION ( 'NONE',  ( 0.000000000000000000, 0.000000000000000000, 1.000000000000000000 ) ) ;
#9733 = CARTESIAN_POINT ( 'NONE',  ( -17.86170306354900816, -9.037578821739909785, 5.749491821935610147 ) ) ;
#9734 = CARTESIAN_POINT ( 'NONE',  ( -6.403603917672690216, 18.96607824920917551, 5.749491821935610147 ) ) ;
#9735 = CARTESIAN_POINT ( 'NONE',  ( 2.555255504830965751, -9.131494062835621150, 1.500000000000001332 ) ) ;
#9736 = LINE ( 'NONE', #2420, #24350 ) ;
#9737 = EDGE_CURVE ( 'NONE', #18512, #16129, #10689, .T. ) ;
#9738 = EDGE_CURVE ( 'NONE', #7027, #16799, #15823, .T. ) ;
#9739 = CARTESIAN_POINT ( 'NONE',  ( -18.43314756787627928, -7.806103702558631952, 18.90679857307105749 ) ) ;
#9740 = CARTESIAN_POINT ( 'NONE',  ( 0.000000000000000000, -8.043452525345523162E-15, -16.50000000000000000 ) ) ;
#9741 = VERTEX_POINT ( 'NONE', #1032 ) ;
#9742 = ORIENTED_EDGE ( 'NONE', *, *, #19805, .T. ) ;
#9743 = ADVANCED_FACE ( 'NONE', ( #15522 ), #29571, .T. ) ;
#9744 = CARTESIAN_POINT ( 'NONE',  ( 35.76344986165623396, 22.29344514668041199, -19.50000000000000355 ) ) ;
#9745 = CARTESIAN_POINT ( 'NONE',  ( -13.30548897721377699, 10.64932510079500538, 7.652108011868850035 ) ) ;
#9746 = ADVANCED_FACE ( 'NONE', ( #8364 ), #12432, .F. ) ;
#9747 = DIRECTION ( 'NONE',  ( 0.000000000000000000, 0.000000000000000000, 1.000000000000000000 ) ) ;
#9748 = ORIENTED_EDGE ( 'NONE', *, *, #17781, .F. ) ;
#9749 = APPLICATION_PROTOCOL_DEFINITION ( 'draft international standard', 'automotive_design', 1998, #9626 ) ;
#9750 = CARTESIAN_POINT ( 'NONE',  ( 15.72291199960844743, -6.567794255929246816, 18.36582235739946611 ) ) ;
#9751 = CIRCLE ( 'NONE', #24184, 19.49999999999996447 ) ;
#9752 = CARTESIAN_POINT ( 'NONE',  ( 5.016833900951458425, 16.26516650762553695, 6.755862304746362845 ) ) ;
#9753 = ADVANCED_FACE ( 'NONE', ( #10542 ), #10224, .F. ) ;
#9754 = ORIENTED_EDGE ( 'NONE', *, *, #20037, .T. ) ;
#9755 = DIRECTION ( 'NONE',  ( 0.000000000000000000, 0.000000000000000000, -1.000000000000000000 ) ) ;
#9756 = CARTESIAN_POINT ( 'NONE',  ( 14.35775550668713407, 13.94852561378611533, 7.280727868105637768 ) ) ;
#9757 = EDGE_CURVE ( 'NONE', #21725, #25705, #5702, .T. ) ;
#9758 = CYLINDRICAL_SURFACE ( 'NONE', #21792, 9.482273699623480212 ) ;
#9759 = CARTESIAN_POINT ( 'NONE',  ( -38.60694528318246199, 6.056885966054946557, 35.03813756351178199 ) ) ;
#9760 = VERTEX_POINT ( 'NONE', #25183 ) ;
#9761 = DIRECTION ( 'NONE',  ( 0.000000000000000000, 1.132880637372608986E-16, -1.000000000000000000 ) ) ;
#9763 = EDGE_CURVE ( 'NONE', #13217, #28109, #27820, .T. ) ;
#9762 = AXIS2_PLACEMENT_3D ( 'NONE', #23358, #9027, #9481 ) ;
#9764 = CARTESIAN_POINT ( 'NONE',  ( 25.47847050916411504, 26.57182937991349903, 1.500000000000001332 ) ) ;
#9765 = AXIS2_PLACEMENT_3D ( 'NONE', #13595, #1272, #3607 ) ;
#9766 = CARTESIAN_POINT ( 'NONE',  ( 23.07173088127199279, 36.25735992984930789, -16.49999999999999645 ) ) ;
#9767 = ORIENTED_EDGE ( 'NONE', *, *, #18702, .F. ) ;
#9768 = DIRECTION ( 'NONE',  ( 0.6707505147970127535, 0.7416830501633041584, 0.000000000000000000 ) ) ;
#9769 = CARTESIAN_POINT ( 'NONE',  ( -4.163336342344337027E-14, 1.387778780781445676E-14, 21.50000000000000000 ) ) ;
#9770 = CARTESIAN_POINT ( 'NONE',  ( 14.33033395197103843, 13.95171706641510490, 7.272192800924335288 ) ) ;
#9771 = DIRECTION ( 'NONE',  ( 1.000000000000000000, 0.000000000000000000, 0.000000000000000000 ) ) ;
#9772 = AXIS2_PLACEMENT_3D ( 'NONE', #2139, #16181, #30666 ) ;
#9773 = DIRECTION ( 'NONE',  ( 0.9096319953545185522, -0.4154150130018859910, -0.000000000000000000 ) ) ;
#9774 = DIRECTION ( 'NONE',  ( -0.000000000000000000, -0.000000000000000000, 1.000000000000000000 ) ) ;
#9775 = CARTESIAN_POINT ( 'NONE',  ( 37.14925617980244255, -12.95022789879826419, 10.21045242721227275 ) ) ;
#9776 = AXIS2_PLACEMENT_3D ( 'NONE', #19838, #12984, #1122 ) ;
#9777 = CARTESIAN_POINT ( 'NONE',  ( 0.000000000000000000, -1.307826893540337417E-14, 27.94260272410217638 ) ) ;
#9778 = ORIENTED_EDGE ( 'NONE', *, *, #5768, .F. ) ;
#9779 = ADVANCED_FACE ( 'NONE', ( #20509, #6478 ), #1335, .F. ) ;
#9780 = EDGE_CURVE ( 'NONE', #11004, #191, #20810, .T. ) ;
#9781 = LINE ( 'NONE', #424, #28193 ) ;
#9782 = CARTESIAN_POINT ( 'NONE',  ( 0.000000000000000000, 0.000000000000000000, 21.50000000000000000 ) ) ;
#9783 = ORIENTED_EDGE ( 'NONE', *, *, #14133, .T. ) ;
#9784 = EDGE_CURVE ( 'NONE', #1286, #18512, #30473, .T. ) ;
#9785 = VERTEX_POINT ( 'NONE', #9115 ) ;
#9786 = AXIS2_PLACEMENT_3D ( 'NONE', #11054, #8572, #15414 ) ;
#9787 = CARTESIAN_POINT ( 'NONE',  ( -18.25679605800083749, 37.59630342716597795, 23.77315958162180465 ) ) ;
#9788 = CARTESIAN_POINT ( 'NONE',  ( -8.751508360190436875, 49.22988072648480795, -42.80776806924027511 ) ) ;
#9789 = VECTOR ( 'NONE', #5559, 1000.000000000000000 ) ;
#9790 = ADVANCED_FACE ( 'NONE', ( #13663 ), #11314, .F. ) ;
#9791 = ORIENTED_EDGE ( 'NONE', *, *, #15663, .F. ) ;
#9792 = AXIS2_PLACEMENT_3D ( 'NONE', #21248, #27572, #30778 ) ;
#9793 = CARTESIAN_POINT ( 'NONE',  ( 12.35846532919128116, 11.73919094318043399, 20.34789198813115263 ) ) ;
#9794 = FACE_OUTER_BOUND ( 'NONE', #30531, .T. ) ;
#9795 = EDGE_CURVE ( 'NONE', #11295, #11064, #16293, .T. ) ;
#9796 = ORIENTED_EDGE ( 'NONE', *, *, #6379, .F. ) ;
#9797 = CARTESIAN_POINT ( 'NONE',  ( 16.11353791281286973, -5.634185590772404773, 19.97651184436794125 ) ) ;
#9798 = CARTESIAN_POINT ( 'NONE',  ( 19.57381806301096105, 4.191719245021452878, 19.47783254395485031 ) ) ;
#9799 = AXIS2_PLACEMENT_3D ( 'NONE', #29232, #3337, #12869 ) ;
#9800 = CARTESIAN_POINT ( 'NONE',  ( 7.392982946727082449, -5.278755796068694828, 13.22130136205108819 ) ) ;
#9801 = ORIENTED_EDGE ( 'NONE', *, *, #6854, .F. ) ;
#9802 = CARTESIAN_POINT ( 'NONE',  ( 15.81223572262636878, -6.365019322297388094, 20.34789198813115263 ) ) ;
#9803=STYLED_ITEM('',(#30879),#2927);
#9804 = VECTOR ( 'NONE', #14938, 1000.000000000000000 ) ;
#9805 = EDGE_LOOP ( 'NONE', ( #5898, #25141, #6827, #24175 ) ) ;
#9806 = CIRCLE ( 'NONE', #6796, 0.7500000000000002220 ) ;
#9807 = ADVANCED_FACE ( 'NONE', ( #22994 ), #27994, .F. ) ;
#9808 = CARTESIAN_POINT ( 'NONE',  ( 38.85099238961694823, 3.925783015303134338, 32.18467226953571725 ) ) ;
#9809 = CARTESIAN_POINT ( 'NONE',  ( -12.78170796079387017, 11.24374406685325489, 18.90679857307105749 ) ) ;
#9810 = ADVANCED_FACE ( 'NONE', ( #3683 ), #5651, .T. ) ;
#9811 = VECTOR ( 'NONE', #26400, 1000.000000000000000 ) ;
#9812 = CARTESIAN_POINT ( 'NONE',  ( -9.833673822381070906, -17.43574673801737873, 18.73743063545763121 ) ) ;
#9813 = DIRECTION ( 'NONE',  ( -0.000000000000000000, 0.000000000000000000, 1.000000000000000000 ) ) ;
#9814 = CARTESIAN_POINT ( 'NONE',  ( 9.755064781586030520, 13.32952022457704544, -0.6213203435596476032 ) ) ;
#9815 = CARTESIAN_POINT ( 'NONE',  ( 0.000000000000000000, 0.000000000000000000, -52.50000000000000000 ) ) ;
#9816 = ORIENTED_EDGE ( 'NONE', *, *, #12500, .T. ) ;
#9817 = CARTESIAN_POINT ( 'NONE',  ( 0.000000000000000000, 90.00000000000001421, -55.00000000000000711 ) ) ;
#9818 = CARTESIAN_POINT ( 'NONE',  ( -31.32177610871843854, 25.32617988875603032, 8.278890997040555533 ) ) ;
#9819 = CARTESIAN_POINT ( 'NONE',  ( 14.96983285839274380, 13.26353275515934449, 20.34789198813115263 ) ) ;
#9820 = AXIS2_PLACEMENT_3D ( 'NONE', #7489, #23536, #11697 ) ;
#9821 = DIRECTION ( 'NONE',  ( 1.000000000000000000, 0.000000000000000000, 0.000000000000000000 ) ) ;
#9822 = EDGE_LOOP ( 'NONE', ( #10659, #27977, #6308, #24137 ) ) ;
#9823 = ORIENTED_EDGE ( 'NONE', *, *, #16067, .F. ) ;
#9824 = CYLINDRICAL_SURFACE ( 'NONE', #13323, 7.500000000000013323 ) ;
#9825 = DIRECTION ( 'NONE',  ( 0.000000000000000000, -0.000000000000000000, -1.000000000000000000 ) ) ;
#9826 = CARTESIAN_POINT ( 'NONE',  ( 27.03074382657074537, 6.449748410230991880, -16.55003854064094426 ) ) ;
#9827 = CARTESIAN_POINT ( 'NONE',  ( 18.70942253818555656, -7.068249826530433211, 19.08830981656266346 ) ) ;
#9828 = CARTESIAN_POINT ( 'NONE',  ( 15.81416692036122917, -6.360574302898113430, 5.652196082368483587 ) ) ;
#9829 = AXIS2_PLACEMENT_3D ( 'NONE', #9222, #18737, #28251 ) ;
#9830 = CARTESIAN_POINT ( 'NONE',  ( -3.395021109945014270, 30.50000000000000355, 24.50000000000000000 ) ) ;
#9831 = ORIENTED_EDGE ( 'NONE', *, *, #16230, .F. ) ;
#9832 = ORIENTED_EDGE ( 'NONE', *, *, #13347, .F. ) ;
#9833 = DIRECTION ( 'NONE',  ( 1.000000000000000000, 0.000000000000000000, 0.000000000000000000 ) ) ;
#9834 = FACE_BOUND ( 'NONE', #29948, .T. ) ;
#9835 = DIRECTION ( 'NONE',  ( 1.000000000000000000, 0.000000000000000000, 0.000000000000000000 ) ) ;
#9836 = ORIENTED_EDGE ( 'NONE', *, *, #18202, .T. ) ;
#9837 = PLANE ( 'NONE',  #21276 ) ;
#9838 = EDGE_LOOP ( 'NONE', ( #23531, #30792, #18632, #9742, #9180, #9144, #6400, #30670, #10594, #7654 ) ) ;
#9839 = CIRCLE ( 'NONE', #24802, 9.482273699623480212 ) ;
#9840 = CARTESIAN_POINT ( 'NONE',  ( 18.67779315278252383, -7.200759110456479206, 7.196036389296800451 ) ) ;
#9841 = AXIS2_PLACEMENT_3D ( 'NONE', #16211, #18710, #6851 ) ;
#9842 = CARTESIAN_POINT ( 'NONE',  ( -32.82330813384395185, 22.94799032727105370, -1.500000000000000000 ) ) ;
#9843 = DIRECTION ( 'NONE',  ( 0.000000000000000000, 0.000000000000000000, 1.000000000000000000 ) ) ;
#9844 = CIRCLE ( 'NONE', #28768, 15.00000000000000000 ) ;
#9845 = ORIENTED_EDGE ( 'NONE', *, *, #19075, .T. ) ;
#9846 = B_SPLINE_CURVE_WITH_KNOTS ( 'NONE', 3,
 ( #24055, #12068, #29059, #24523, #9877, #16901, #17046, #200, #15009, #28911, #3017, #19854, #9716, #8014, #17516, #12214, #26417, #354 ),
 .UNSPECIFIED., .F., .F.,
 ( 4, 2, 2, 2, 2, 2, 2, 2, 4 ),
 ( 0.000000000000000000, 0.0003967869494442862583, 0.0007935738988885725166, 0.001190360848332858721, 0.001587147797777145033, 0.001983934747221431129, 0.002380721696665717441, 0.002777508646110003754, 0.003174295595554290066 ),
 .UNSPECIFIED. ) ;
#9847 = DIRECTION ( 'NONE',  ( -0.000000000000000000, -0.000000000000000000, 1.000000000000000000 ) ) ;
#9848 = FACE_OUTER_BOUND ( 'NONE', #12640, .T. ) ;
#9849 = CARTESIAN_POINT ( 'NONE',  ( -33.13218612630368654, -7.028748154183637631, -1.942616967526160643 ) ) ;
#9850 = CARTESIAN_POINT ( 'NONE',  ( 0.9307681286968549905, -9.436481611552757442, 21.50000000000000000 ) ) ;
#9851 = CIRCLE ( 'NONE', #13342, 9.084132297865673777 ) ;
#9852 = CARTESIAN_POINT ( 'NONE',  ( -10.51100883930069863, -17.01524884273342053, 5.652196082369965069 ) ) ;
#9853 = CARTESIAN_POINT ( 'NONE',  ( -4.272706734768118686, -37.25579118954082247, 37.50000000000000000 ) ) ;
#9854 = CARTESIAN_POINT ( 'NONE',  ( 0.09252763182292195188, 6.914127053141852386, -6.024380653971844524 ) ) ;
#9855 = ORIENTED_EDGE ( 'NONE', *, *, #3106, .T. ) ;
#9856 = CARTESIAN_POINT ( 'NONE',  ( 15.44249669564394267, -7.165351778271005223, 7.156916968540301127 ) ) ;
#9857 = CARTESIAN_POINT ( 'NONE',  ( -5.374868878256215510, -44.10336124695545124, -19.50000000000000355 ) ) ;
#9858 = CARTESIAN_POINT ( 'NONE',  ( -8.249114229549590505, 0.1262659238205133538, -3.621320343559650379 ) ) ;
#9859 = ORIENTED_EDGE ( 'NONE', *, *, #20240, .T. ) ;
#9860 = CARTESIAN_POINT ( 'NONE',  ( 64.99999999999998579, -70.00000000000000000, 57.49999999999999289 ) ) ;
#9861 = VECTOR ( 'NONE', #24102, 1000.000000000000000 ) ;
#9862 = CARTESIAN_POINT ( 'NONE',  ( -6.414842543015754295, 17.06554576617236307, 1.500000000000000000 ) ) ;
#9863 = DIRECTION ( 'NONE',  ( 1.000000000000000000, 0.000000000000000000, 0.000000000000000000 ) ) ;
#9864 = VECTOR ( 'NONE', #28806, 1000.000000000000000 ) ;
#9865 = CARTESIAN_POINT ( 'NONE',  ( 2.552544031601107211, 42.49999999998228617, -1.500000000000000000 ) ) ;
#9866 = VECTOR ( 'NONE', #10587, 1000.000000000000000 ) ;
#9867 = DIRECTION ( 'NONE',  ( 1.000000000000000000, 0.000000000000000000, 0.000000000000000000 ) ) ;
#9868 = CARTESIAN_POINT ( 'NONE',  ( 38.96687411310632854, 1.873333295377571650, 35.07604622541821726 ) ) ;
#9869 = DIRECTION ( 'NONE',  ( -0.000000000000000000, -1.000000000000000000, -0.000000000000000000 ) ) ;
#9870 = CARTESIAN_POINT ( 'NONE',  ( 33.57242512144424751, -24.08458161880252035, -13.16663720046962638 ) ) ;
#9872 = VERTEX_POINT ( 'NONE', #28608 ) ;
#9871 = AXIS2_PLACEMENT_3D ( 'NONE', #20127, #12962, #27154 ) ;
#9873 = CARTESIAN_POINT ( 'NONE',  ( -32.24119442679361214, -26.76047168400493703, -16.50000600000000262 ) ) ;
#9874 = CARTESIAN_POINT ( 'NONE',  ( 7.856594496258195726, 4.390207617113981442, 1.500000000000001332 ) ) ;
#9875 = ORIENTED_EDGE ( 'NONE', *, *, #13975, .F. ) ;
#9876 = ORIENTED_EDGE ( 'NONE', *, *, #20952, .F. ) ;
#9877 = CARTESIAN_POINT ( 'NONE',  ( -9.978083804712657212, -17.33339668284229163, 5.853797745100183469 ) ) ;
#9878 = ORIENTED_EDGE ( 'NONE', *, *, #24637, .T. ) ;
#9879 = ORIENTED_EDGE ( 'NONE', *, *, #20040, .F. ) ;
#9880 = CARTESIAN_POINT ( 'NONE',  ( 0.1201197967225753199, -20.01774464624826777, 20.32842677360128292 ) ) ;
#9881 = CARTESIAN_POINT ( 'NONE',  ( 0.000000000000000000, 39.50000000000000000, 34.49999999999999289 ) ) ;
#9882 = CARTESIAN_POINT ( 'NONE',  ( -9.772441304892778291, -17.47026709695450464, 6.131018562779544823 ) ) ;
#9883 = AXIS2_PLACEMENT_3D ( 'NONE', #12272, #28650, #411 ) ;
#9884 = CARTESIAN_POINT ( 'NONE',  ( 4.644508076436818733, 16.38413139296123688, 20.14907003336613300 ) ) ;
#9885 = CARTESIAN_POINT ( 'NONE',  ( 1.208994807697891138, -19.98122169387827896, 19.89182036555910571 ) ) ;
#9886 = AXIS2_PLACEMENT_3D ( 'NONE', #21313, #30523, #21003 ) ;
#9887 = ORIENTED_EDGE ( 'NONE', *, *, #28796, .T. ) ;
#9888 = CARTESIAN_POINT ( 'NONE',  ( 2.552544031601107211, 42.49999999998228617, -1.500000000000003997 ) ) ;
#9889 = FACE_OUTER_BOUND ( 'NONE', #24882, .T. ) ;
#9890 = DIRECTION ( 'NONE',  ( 1.000000000000000000, 0.000000000000000000, 0.000000000000000000 ) ) ;
#9891 = CARTESIAN_POINT ( 'NONE',  ( -22.95669091611927826, -27.54300778121952220, 1.500000000000000000 ) ) ;
#9892 = LINE ( 'NONE', #30791, #174 ) ;
#9893 = ORIENTED_EDGE ( 'NONE', *, *, #3494, .F. ) ;
#9894 = CIRCLE ( 'NONE', #4416, 14.52510309069108807 ) ;
#9895 = CARTESIAN_POINT ( 'NONE',  ( -37.99999999999999289, 209.2686044187655909, -87.50000000000000000 ) ) ;
#9896 = CARTESIAN_POINT ( 'NONE',  ( -17.91073422896667466, -8.940227287121103927, 5.704143890883081269 ) ) ;
#9897 = CARTESIAN_POINT ( 'NONE',  ( -6.359874605901117306, 15.84393421166759097, 7.196036389296800451 ) ) ;
#9898 = CARTESIAN_POINT ( 'NONE',  ( 57.49999999999998579, -50.00000000000000000, 12.49999999999999112 ) ) ;
#9899 = CARTESIAN_POINT ( 'NONE',  ( -37.50000000000005684, 9.285362311011880811E-15, 37.50000000000000000 ) ) ;
#9900 = CARTESIAN_POINT ( 'NONE',  ( -7.869584159753960861, 10.39565510934976977, 24.50000000000000000 ) ) ;
#9901 = CARTESIAN_POINT ( 'NONE',  ( 4.102102735472459294, -8.549050687778176894, 21.50000000000000000 ) ) ;
#9902 = ORIENTED_EDGE ( 'NONE', *, *, #23266, .T. ) ;
#9903 = ORIENTED_EDGE ( 'NONE', *, *, #12895, .T. ) ;
#9904 = DIRECTION ( 'NONE',  ( 0.000000000000000000, 0.000000000000000000, -1.000000000000000000 ) ) ;
#9905 = DIRECTION ( 'NONE',  ( -0.000000000000000000, 1.000000000000000000, -0.000000000000000000 ) ) ;
#9906 = PRODUCT_DEFINITION_FORMATION_WITH_SPECIFIED_SOURCE ( 'ANY', '', #23591, .NOT_KNOWN. ) ;
#9907 = CARTESIAN_POINT ( 'NONE',  ( -57.50000000000001421, 50.00000000000000000, 62.49999999999999289 ) ) ;
#9908 = CARTESIAN_POINT ( 'NONE',  ( 0.6479391102675158276, -17.02974303764478137, 7.652108011868854476 ) ) ;
#9909 = EDGE_LOOP ( 'NONE', ( #7350, #7394, #21128, #28372 ) ) ;
#9910 = CARTESIAN_POINT ( 'NONE',  ( 0.000000000000000000, -2.435693370351110282E-15, 21.50000000000000355 ) ) ;
#9911 = AXIS2_PLACEMENT_3D ( 'NONE', #19414, #19249, #5796 ) ;
#9912 = CIRCLE ( 'NONE', #19865, 9.482273699623480212 ) ;
#9913 = DIRECTION ( 'NONE',  ( 0.000000000000000000, 1.000000000000000000, -0.000000000000000000 ) ) ;
#9914 = ORIENTED_EDGE ( 'NONE', *, *, #27287, .T. ) ;
#9915 = CARTESIAN_POINT ( 'NONE',  ( 4.817555027346758223, 16.32979927342787718, 19.96783386855779341 ) ) ;
#9916 = DIRECTION ( 'NONE',  ( 0.000000000000000000, 0.000000000000000000, 1.000000000000000000 ) ) ;
#9917 = VECTOR ( 'NONE', #656, 1000.000000000000000 ) ;
#9918 = CARTESIAN_POINT ( 'NONE',  ( -44.99999999999955236, -4.926614671774132148E-13, 82.49999999999998579 ) ) ;
#9919 = CARTESIAN_POINT ( 'NONE',  ( -22.70739019994807251, -29.86753719045417910, 37.49999999998765077 ) ) ;
#9920 = VERTEX_POINT ( 'NONE', #7229 ) ;
#9921 = DIRECTION ( 'NONE',  ( -0.000000000000000000, -0.000000000000000000, 1.000000000000000000 ) ) ;
#9922 = EDGE_CURVE ( 'NONE', #7456, #17335, #13519, .T. ) ;
#9923 = EDGE_CURVE ( 'NONE', #1827, #23138, #23705, .T. ) ;
#9924 = CARTESIAN_POINT ( 'NONE',  ( -22.58267429318971864, 26.57182937991348481, 26.54355021145563143 ) ) ;
#9925 = AXIS2_PLACEMENT_3D ( 'NONE', #19381, #17348, #3007 ) ;
#9926 = CARTESIAN_POINT ( 'NONE',  ( 20.26334714462845099, 38.18989983590572024, -16.50000000000000355 ) ) ;
#9927 = VERTEX_POINT ( 'NONE', #29222 ) ;
#9928 = CARTESIAN_POINT ( 'NONE',  ( -15.55662731361435469, -6.910399801605406012, 6.310736198168394928 ) ) ;
#9929 = ADVANCED_FACE ( 'NONE', ( #7861 ), #21891, .F. ) ;
#9930 = DIRECTION ( 'NONE',  ( 1.000000000000000000, 0.000000000000000000, 0.000000000000000000 ) ) ;
#9931 = FACE_OUTER_BOUND ( 'NONE', #10255, .T. ) ;
#9932 = EDGE_CURVE ( 'NONE', #24994, #22249, #2296, .T. ) ;
#9933 = CARTESIAN_POINT ( 'NONE',  ( 0.3541519782205873601, -20.01464289576668065, 5.652196082367002994 ) ) ;
#9934 = AXIS2_PLACEMENT_3D ( 'NONE', #23932, #14884, #2732 ) ;
#9935 = CYLINDRICAL_SURFACE ( 'NONE', #7794, 0.7500000000000002220 ) ;
#9936 = FACE_OUTER_BOUND ( 'NONE', #7012, .T. ) ;
#9937 = CARTESIAN_POINT ( 'NONE',  ( 33.16313691975489064, 7.028748154183637631, -1.500000000000000000 ) ) ;
#9938 = FACE_BOUND ( 'NONE', #20612, .T. ) ;
#9939 = ORIENTED_EDGE ( 'NONE', *, *, #28839, .F. ) ;
#9940 = ADVANCED_FACE ( 'NONE', ( #10654 ), #24684, .F. ) ;
#9941 = DIRECTION ( 'NONE',  ( 0.000000000000000000, 0.000000000000000000, -1.000000000000000000 ) ) ;
#9942 = AXIS2_PLACEMENT_3D ( 'NONE', #15979, #30775, #3980 ) ;
#9943 = CARTESIAN_POINT ( 'NONE',  ( 5.169584817211991812, 19.32078214751396317, 7.652108011868850923 ) ) ;
#9944 = EDGE_CURVE ( 'NONE', #7727, #30552, #22229, .T. ) ;
#9945 = ORIENTED_EDGE ( 'NONE', *, *, #13800, .T. ) ;
#9946 = EDGE_LOOP ( 'NONE', ( #2581, #9190, #27744, #25880 ) ) ;
#9947 = EDGE_CURVE ( 'NONE', #30435, #11497, #15167, .T. ) ;
#9948 = DIRECTION ( 'NONE',  ( -0.000000000000000000, -0.000000000000000000, 1.000000000000000000 ) ) ;
#9949 = DIRECTION ( 'NONE',  ( 0.000000000000000000, 0.000000000000000000, 1.000000000000000000 ) ) ;
#9950 = VERTEX_POINT ( 'NONE', #29068 ) ;
#9951 = AXIS2_PLACEMENT_3D ( 'NONE', #21522, #21678, #14666 ) ;
#9952 = CARTESIAN_POINT ( 'NONE',  ( 15.45804667738991967, 12.71867858434618093, 19.87181966307587544 ) ) ;
#9953 = CARTESIAN_POINT ( 'NONE',  ( -11.24586906513001416, -16.56046035145272555, 6.111214848085761986 ) ) ;
#9954 = ORIENTED_EDGE ( 'NONE', *, *, #16616, .F. ) ;
#9955 = CARTESIAN_POINT ( 'NONE',  ( 16.05603743463488797, -5.780788835868658992, 20.13759033520874908 ) ) ;
#9956 = FACE_OUTER_BOUND ( 'NONE', #722, .T. ) ;
#9957 = CARTESIAN_POINT ( 'NONE',  ( -26.58597676761596063, 6.321098805557480382, 47.67294373134352270 ) ) ;
#9958 = ORIENTED_EDGE ( 'NONE', *, *, #4028, .F. ) ;
#9959 = DIRECTION ( 'NONE',  ( -0.8412535328311804284, 0.5406408174555987767, 0.000000000000000000 ) ) ;
#9960 = EDGE_CURVE ( 'NONE', #14341, #7065, #19802, .T. ) ;
#9961 = ORIENTED_EDGE ( 'NONE', *, *, #22707, .T. ) ;
#9962 = EDGE_CURVE ( 'NONE', #16597, #17742, #15017, .T. ) ;
#9963 = EDGE_CURVE ( 'NONE', #28104, #19006, #6207, .T. ) ;
#9964 = AXIS2_PLACEMENT_3D ( 'NONE', #19041, #12177, #26057 ) ;
#9965 = EDGE_CURVE ( 'NONE', #17954, #12796, #14243, .T. ) ;
#9966 = ORIENTED_EDGE ( 'NONE', *, *, #15253, .T. ) ;
#9967 = B_SPLINE_CURVE_WITH_KNOTS ( 'NONE', 3,
 ( #26746, #5068, #2251, #30798, #9446, #16603 ),
 .UNSPECIFIED., .F., .F.,
 ( 4, 2, 4 ),
 ( 2.108697328626194806E-07, 0.0003800081648695531611, 0.0007598054600062437158 ),
 .UNSPECIFIED. ) ;
#9968 = EDGE_CURVE ( 'NONE', #8546, #28303, #13007, .T. ) ;
#9969 = CARTESIAN_POINT ( 'NONE',  ( -7.856594496258223259, -4.390207617113929039, -1.500000000000002220 ) ) ;
#9970 = CARTESIAN_POINT ( 'NONE',  ( -6.485253725360694332, 18.93805017237212951, 20.19593175699879595 ) ) ;
#9971 = CARTESIAN_POINT ( 'NONE',  ( -15.06643696584252190, 13.18059642443756907, 20.25336174263950184 ) ) ;
#9972 = VECTOR ( 'NONE', #8994, 1000.000000000000000 ) ;
#9973 = CARTESIAN_POINT ( 'NONE',  ( -8.257638164125266300, -14.92340941578111035, 18.39992786714538298 ) ) ;
#9974 = EDGE_CURVE ( 'NONE', #28528, #17576, #27721, .T. ) ;
#9975 = CARTESIAN_POINT ( 'NONE',  ( -24.57665676473017413, -33.00632471879952590, 29.73950062350330725 ) ) ;
#9976 = CARTESIAN_POINT ( 'NONE',  ( -15.75094665830067697, -12.32508334119358828, 24.50000000000000000 ) ) ;
#9977 = CARTESIAN_POINT ( 'NONE',  ( 7.856594496258195726, 4.390207617113981442, 21.50000000000000000 ) ) ;
#9978 = ORIENTED_EDGE ( 'NONE', *, *, #2777, .T. ) ;
#9979 = EDGE_CURVE ( 'NONE', #16888, #477, #17747, .T. ) ;
#9980 = CARTESIAN_POINT ( 'NONE',  ( -16.96555893289282935, 1.647560171710579002, 5.652196082364320695 ) ) ;
#9981 = DIRECTION ( 'NONE',  ( -0.000000000000000000, 1.132880637372608986E-16, -1.000000000000000000 ) ) ;
#9982 = DIRECTION ( 'NONE',  ( 1.000000000000000000, 0.000000000000000000, 0.000000000000000000 ) ) ;
#9983 = CARTESIAN_POINT ( 'NONE',  ( 19.87646685382696177, 2.220054991963873903, 6.913388067999417963 ) ) ;
#9984 = VERTEX_POINT ( 'NONE', #8773 ) ;
#9985 = ORIENTED_EDGE ( 'NONE', *, *, #5345, .T. ) ;
#9986 = CARTESIAN_POINT ( 'NONE',  ( 10.58781394000596165, -16.96782583993082483, 7.454139397117725885 ) ) ;
#9987 = CARTESIAN_POINT ( 'NONE',  ( -5.279695238918636235, 19.30927203514150747, 7.359006845440219102 ) ) ;
#9988 = CARTESIAN_POINT ( 'NONE',  ( 12.18183868330171826, 11.93592587879421174, 7.652108011868850923 ) ) ;
#9989 = AXIS2_PLACEMENT_3D ( 'NONE', #30730, #28873, #9835 ) ;
#9990 = LINE ( 'NONE', #4532, #11438 ) ;
#9991 = EDGE_CURVE ( 'NONE', #10311, #9122, #7298, .T. ) ;
#9992 = ORIENTED_EDGE ( 'NONE', *, *, #192, .T. ) ;
#9993 = EDGE_CURVE ( 'NONE', #24284, #26415, #18254, .T. ) ;
#9994 = DIRECTION ( 'NONE',  ( -0.000000000000000000, -0.000000000000000000, -1.000000000000000000 ) ) ;
#9995 = CARTESIAN_POINT ( 'NONE',  ( -1.687027447297492211, -8.840471615930066918, 21.50000000000000000 ) ) ;
#9996 = DIRECTION ( 'NONE',  ( 1.000000000000000000, 0.000000000000000000, 0.000000000000000000 ) ) ;
#9997 = EDGE_LOOP ( 'NONE', ( #15122, #4034, #26431, #16626 ) ) ;
#9998 = DIRECTION ( 'NONE',  ( 0.9547931052914340189, -0.2972711322815261292, 0.000000000000000000 ) ) ;
#9999 = ADVANCED_FACE ( 'NONE', ( #23108 ), #15959, .F. ) ;
#10000 = ORIENTED_EDGE ( 'NONE', *, *, #22171, .T. ) ;
#10001 = CARTESIAN_POINT ( 'NONE',  ( 15.98415658701447839, -5.958736450466536105, 7.559636331181775581 ) ) ;
#10002 = CARTESIAN_POINT ( 'NONE',  ( 16.58213327075252863, 4.067275193330053717, 18.84329447212444109 ) ) ;
#10003 = DIRECTION ( 'NONE',  ( 0.000000000000000000, 0.000000000000000000, 1.000000000000000000 ) ) ;
#10004 = EDGE_LOOP ( 'NONE', ( #22747, #22989, #16695, #270 ) ) ;
#10005 = CARTESIAN_POINT ( 'NONE',  ( 3.613053539807239645, 16.67204840528144061, 5.749491821935610147 ) ) ;
#10006 = CARTESIAN_POINT ( 'NONE',  ( 1.073881485057758711, -0.9711784013061475207, 1.500000000000000000 ) ) ;
#10007 = CARTESIAN_POINT ( 'NONE',  ( 69.99999999999998579, 50.00000000000000000, -92.50000000000000000 ) ) ;
#10008 = CARTESIAN_POINT ( 'NONE',  ( 33.42925964089140933, 11.06161099612213405, 39.78814634291935448 ) ) ;
#10009 = CIRCLE ( 'NONE', #29429, 9.482273699623480212 ) ;
#10010 = DIRECTION ( 'NONE',  ( -0.000000000000000000, 1.132880637372608986E-16, -1.000000000000000000 ) ) ;
#10011 = CARTESIAN_POINT ( 'NONE',  ( 9.860909911264737815, -13.90333503211346944, 20.34789198813115263 ) ) ;
#10012 = CARTESIAN_POINT ( 'NONE',  ( 33.47438960496221227, 10.94461781313380477, 39.78205384324066074 ) ) ;
#10013 = ORIENTED_EDGE ( 'NONE', *, *, #25981, .F. ) ;
#10014 = PLANE ( 'NONE',  #30186 ) ;
#10015 = B_SPLINE_CURVE_WITH_KNOTS ( 'NONE', 3,
 ( #30135, #18290, #10648, #11262 ),
 .UNSPECIFIED., .F., .F.,
 ( 4, 4 ),
 ( 3.022186913359086288E-07, 0.007932103869840194041 ),
 .UNSPECIFIED. ) ;
#10016 = CARTESIAN_POINT ( 'NONE',  ( 31.18700685317242716, 26.11823559933198879, -1.500000000000000000 ) ) ;
#10017 = DIRECTION ( 'NONE',  ( -1.000000000000000000, -0.000000000000000000, -0.000000000000000000 ) ) ;
#10018 = ORIENTED_EDGE ( 'NONE', *, *, #26131, .T. ) ;
#10019 = CARTESIAN_POINT ( 'NONE',  ( -14.88329716083760346, -8.348731837201613715, 20.13759033520874908 ) ) ;
#10020 = CYLINDRICAL_SURFACE ( 'NONE', #805, 1.000000000000007772 ) ;
#10021 = CARTESIAN_POINT ( 'NONE',  ( -15.01328179936713880, 13.21424408877643941, 20.22277707861862339 ) ) ;
#10022 = CARTESIAN_POINT ( 'NONE',  ( 4.299378382534376541, 16.48726736029815143, 5.676815824193227833 ) ) ;
#10023 = CARTESIAN_POINT ( 'NONE',  ( -2.552544031601109875, 42.50000000001772094, -1.500000000000000000 ) ) ;
#10024 = LINE ( 'NONE', #7689, #17454 ) ;
#10025 = CARTESIAN_POINT ( 'NONE',  ( 28.00167021653412291, 24.95069493026310070, 37.49999999999567990 ) ) ;
#10026 = EDGE_CURVE ( 'NONE', #15180, #27348, #30678, .T. ) ;
#10027 = DIRECTION ( 'NONE',  ( 1.000000000000000000, 0.000000000000000000, 0.000000000000000000 ) ) ;
#10028 = ORIENTED_EDGE ( 'NONE', *, *, #3704, .T. ) ;
#10029 = VECTOR ( 'NONE', #10908, 1000.000000000000114 ) ;
#10030 = CARTESIAN_POINT ( 'NONE',  ( -2.959227181723746547, 8.499586724479465616, -1.500000000000000888 ) ) ;
#10031 = EDGE_LOOP ( 'NONE', ( #25902, #22592, #17073, #23545, #5974, #6725, #8022, #12333, #8900 ) ) ;
#10032 = CARTESIAN_POINT ( 'NONE',  ( -6.301234758012549619, 6.543385983536412098, 13.22130136205108819 ) ) ;
#10033 = FACE_OUTER_BOUND ( 'NONE', #29993, .T. ) ;
#10034 = ORIENTED_EDGE ( 'NONE', *, *, #7655, .F. ) ;
#10035 = VERTEX_POINT ( 'NONE', #25315 ) ;
#10036 = CYLINDRICAL_SURFACE ( 'NONE', #28718, 20.00000000000000000 ) ;
#10037 = ORIENTED_EDGE ( 'NONE', *, *, #21785, .T. ) ;
#10038 = ORIENTED_EDGE ( 'NONE', *, *, #24867, .T. ) ;
#10039 = CARTESIAN_POINT ( 'NONE',  ( 24.03057240117691862, 26.57182937991349903, 24.50000000000000000 ) ) ;
#10040 = CARTESIAN_POINT ( 'NONE',  ( -29.55190575096636607, 22.57725177722917920, 34.50000000000000711 ) ) ;
#10041 = DIRECTION ( 'NONE',  ( 1.000000000000000000, 0.000000000000000000, 0.000000000000000000 ) ) ;
#10042 = CARTESIAN_POINT ( 'NONE',  ( -7.667077102831937552, 13.77986170986486592, -0.6213203435596476032 ) ) ;
#10043 = DIRECTION ( 'NONE',  ( 1.000000000000000000, 0.000000000000000000, 0.000000000000000000 ) ) ;
#10044 = EDGE_LOOP ( 'NONE', ( #10488, #23598, #27969, #8163 ) ) ;
#10045 = LINE ( 'NONE', #5365, #5396 ) ;
#10046 = DIRECTION ( 'NONE',  ( 0.000000000000000000, 0.000000000000000000, 1.000000000000000000 ) ) ;
#10047 = CARTESIAN_POINT ( 'NONE',  ( 11.65981318837298453, 12.47865322263302446, 19.36813350477385143 ) ) ;
#10048 = FACE_BOUND ( 'NONE', #13149, .T. ) ;
#10049 = ORIENTED_EDGE ( 'NONE', *, *, #7106, .T. ) ;
#10050 = AXIS2_PLACEMENT_3D ( 'NONE', #4141, #16303, #18501 ) ;
#10051 = DIRECTION ( 'NONE',  ( 1.000000000000000000, 0.000000000000000000, 0.000000000000000000 ) ) ;
#10052 = CARTESIAN_POINT ( 'NONE',  ( -17.96015518819250545, -8.839856506746546216, 5.678370764302467677 ) ) ;
#10053 = CARTESIAN_POINT ( 'NONE',  ( -5.621668343899179909, 16.09410144477765314, 5.652605728828373977 ) ) ;
#10054 = DIRECTION ( 'NONE',  ( 1.000000000000000000, 0.000000000000000000, 0.000000000000000000 ) ) ;
#10055 = LINE ( 'NONE', #5530, #6630 ) ;
#10056 = VERTEX_POINT ( 'NONE', #20329 ) ;
#10057 = ORIENTED_EDGE ( 'NONE', *, *, #21373, .T. ) ;
#10058 = DIRECTION ( 'NONE',  ( -0.7557495743542581579, -0.6548607339452852116, 0.000000000000000000 ) ) ;
#10059 = CARTESIAN_POINT ( 'NONE',  ( 0.000000000000000000, 44.39187623478217404, -19.50000000000000355 ) ) ;
#10060 = CARTESIAN_POINT ( 'NONE',  ( -12.77302042131097792, 11.25334833650868838, 7.080843742048788414 ) ) ;
#10061 = DIRECTION ( 'NONE',  ( 1.000000000000000000, 0.000000000000000000, 0.000000000000000000 ) ) ;
#10062 = ORIENTED_EDGE ( 'NONE', *, *, #13390, .T. ) ;
#10063 = APPLICATION_PROTOCOL_DEFINITION ( 'draft international standard', 'automotive_design', 1998, #25330 ) ;
#10064 = CARTESIAN_POINT ( 'NONE',  ( 15.91946090815430104, -6.118695897821246454, 18.34938820207545263 ) ) ;
#10065 = DIRECTION ( 'NONE',  ( -0.000000000000000000, -0.000000000000000000, 1.000000000000000000 ) ) ;
#10066 = VERTEX_POINT ( 'NONE', #25478 ) ;
#10067 = CARTESIAN_POINT ( 'NONE',  ( -24.03448224033878944, -8.660042335149837456, 45.23564988763774863 ) ) ;
#10068 = CARTESIAN_POINT ( 'NONE',  ( -33.67904611720921793, -24.24635140548038237, -14.83330431372253777 ) ) ;
#10069 = AXIS2_PLACEMENT_3D ( 'NONE', #5314, #2986, #26384 ) ;
#10070 = DIRECTION ( 'NONE',  ( 0.000000000000000000, 0.000000000000000000, 1.000000000000000000 ) ) ;
#10071 = CARTESIAN_POINT ( 'NONE',  ( -29.86178407246424626, -27.47635996432160255, 34.56532846876351073 ) ) ;
#10072 = EDGE_LOOP ( 'NONE', ( #5280, #23065, #30610 ) ) ;
#10073 = DIRECTION ( 'NONE',  ( 0.000000000000000000, 1.000000000000000000, 1.193512090021232842E-16 ) ) ;
#10074 = CARTESIAN_POINT ( 'NONE',  ( -19.64114023396299302, -37.13592150529018454, -1.500000000000000000 ) ) ;
#10075 = CARTESIAN_POINT ( 'NONE',  ( -19.69223482763159083, 3.495123391383816447, 19.21471108562415253 ) ) ;
#10076 = ORIENTED_EDGE ( 'NONE', *, *, #16826, .F. ) ;
#10077 = DIRECTION ( 'NONE',  ( 0.000000000000000000, 1.000000000000000000, 0.000000000000000000 ) ) ;
#10078 = PLANE ( 'NONE',  #1892 ) ;
#10079 = FACE_BOUND ( 'NONE', #434, .T. ) ;
#10080 = CARTESIAN_POINT ( 'NONE',  ( -0.5073662589470756545, -20.01152162034081883, 6.111214848085761986 ) ) ;
#10081 = CARTESIAN_POINT ( 'NONE',  ( 0.1262659238204208167, 8.999114229549594057, 1.500000000000001332 ) ) ;
#10082 = DIRECTION ( 'NONE',  ( 0.000000000000000000, 0.000000000000000000, -1.000000000000000000 ) ) ;
#10083 = CARTESIAN_POINT ( 'NONE',  ( -6.812559277181930106, 5.881244434206302607, 21.50000000000000000 ) ) ;
#10084 = DIRECTION ( 'NONE',  ( 0.000000000000000000, 1.000000000000000000, 0.000000000000000000 ) ) ;
#10085 = ORIENTED_EDGE ( 'NONE', *, *, #17938, .F. ) ;
#10086 = DIRECTION ( 'NONE',  ( 1.000000000000000000, 0.000000000000000000, 0.000000000000000000 ) ) ;
#10087 = DIRECTION ( 'NONE',  ( 0.000000000000000000, 0.000000000000000000, -1.000000000000000000 ) ) ;
#10088 = ORIENTED_EDGE ( 'NONE', *, *, #15880, .T. ) ;
#10089 = ORIENTED_EDGE ( 'NONE', *, *, #24457, .F. ) ;
#10090 = EDGE_CURVE ( 'NONE', #26641, #5849, #16749, .T. ) ;
#10091 = CARTESIAN_POINT ( 'NONE',  ( -0.8974428369466271871, 42.49999999999999289, 19.72227980406326253 ) ) ;
#10092 = FACE_BOUND ( 'NONE', #28857, .T. ) ;
#10093 = ORIENTED_EDGE ( 'NONE', *, *, #27152, .F. ) ;
#10094 = CARTESIAN_POINT ( 'NONE',  ( 12.95659581195170773, 11.04149104205339427, 19.77662771831109367 ) ) ;
#10095 = AXIS2_PLACEMENT_3D ( 'NONE', #28745, #11915, #23583 ) ;
#10096 = VECTOR ( 'NONE', #21030, 1000.000000000000000 ) ;
#10097 = DIRECTION ( 'NONE',  ( -0.000000000000000000, -0.000000000000000000, -1.000000000000000000 ) ) ;
#10098 = ORIENTED_EDGE ( 'NONE', *, *, #14304, .T. ) ;
#10099 = EDGE_CURVE ( 'NONE', #2298, #29282, #25002, .T. ) ;
#10100 = VECTOR ( 'NONE', #23279, 1000.000000000000000 ) ;
#10101 = CARTESIAN_POINT ( 'NONE',  ( 18.73275811567551230, -7.056106374802665115, 19.47783254395485031 ) ) ;
#10102 = CARTESIAN_POINT ( 'NONE',  ( 16.63005575832078975, 3.830191698062870742, 18.56793045041961321 ) ) ;
#10103 = CARTESIAN_POINT ( 'NONE',  ( 8.268028093133366951, 3.763133143576461670, 21.50000000000000000 ) ) ;
#10104 = ORIENTED_EDGE ( 'NONE', *, *, #25557, .T. ) ;
#10105 = DIRECTION ( 'NONE',  ( -1.000000000000000000, 0.000000000000000000, 0.000000000000000000 ) ) ;
#10106 = ORIENTED_EDGE ( 'NONE', *, *, #15231, .T. ) ;
#10107 = B_SPLINE_CURVE_WITH_KNOTS ( 'NONE', 3,
 ( #11249, #30429, #1734, #13898 ),
 .UNSPECIFIED., .F., .F.,
 ( 4, 4 ),
 ( 3.022186913382060468E-07, 0.007932103869840216592 ),
 .UNSPECIFIED. ) ;
#10108 = EDGE_CURVE ( 'NONE', #12149, #4214, #25217, .T. ) ;
#10109 = CARTESIAN_POINT ( 'NONE',  ( 35.53662292511247500, 17.55688491361479819, 31.31080097343302171 ) ) ;
#10110 = CARTESIAN_POINT ( 'NONE',  ( -6.055745631507631899, 15.95075576291064223, 20.19593175699879595 ) ) ;
#10111 = CARTESIAN_POINT ( 'NONE',  ( -12.96319695304515207, 11.04295072071645656, 20.12545155307891065 ) ) ;
#10112 = CARTESIAN_POINT ( 'NONE',  ( -25.47847050916411504, 26.57182937991348481, 24.50000000000000000 ) ) ;
#10113 = CARTESIAN_POINT ( 'NONE',  ( -25.05233252773468422, -32.57872576663409347, 29.78309721723623582 ) ) ;
#10114 = VECTOR ( 'NONE', #19773, 1000.000000000000227 ) ;
#10115 = FACE_OUTER_BOUND ( 'NONE', #25680, .T. ) ;
#10116 = CARTESIAN_POINT ( 'NONE',  ( -13.00999358272542494, -0.8602714556717691030, 1.500000000000001332 ) ) ;
#10117 = VERTEX_POINT ( 'NONE', #1755 ) ;
#10118 = VECTOR ( 'NONE', #8787, 999.9999999999998863 ) ;
#10119 = CARTESIAN_POINT ( 'NONE',  ( -16.98411243466784271, 1.496360031252973233, 5.661398277488801867 ) ) ;
#10120 = CARTESIAN_POINT ( 'NONE',  ( 28.69771818040356237, -23.84998595875660499, 34.50000000000000711 ) ) ;
#10121 = CARTESIAN_POINT ( 'NONE',  ( 19.81826808356698422, 2.692791747024147142, 7.526993102356318133 ) ) ;
#10122 = ORIENTED_EDGE ( 'NONE', *, *, #22358, .F. ) ;
#10123 = ORIENTED_EDGE ( 'NONE', *, *, #6675, .T. ) ;
#10124 = LINE ( 'NONE', #10444, #25777 ) ;
#10125 = EDGE_CURVE ( 'NONE', #4914, #4107, #4702, .T. ) ;
#10126 = CIRCLE ( 'NONE', #9130, 7.500000000000013323 ) ;
#10127 = CARTESIAN_POINT ( 'NONE',  ( -10.47960520055065636, -7.757439966934454034, 1.500000000000001332 ) ) ;
#10128 = ADVANCED_FACE ( 'NONE', ( #18146 ), #15484, .F. ) ;
#10129 = CARTESIAN_POINT ( 'NONE',  ( 18.38841581631819011, -7.866599884335181869, 20.34789198813115263 ) ) ;
#10130 = CARTESIAN_POINT ( 'NONE',  ( -15.56507824124772554, -6.890134373246081800, 6.910395520694542881 ) ) ;
#10131 = CARTESIAN_POINT ( 'NONE',  ( 5.881244434206234217, 6.812559277181991391, 21.50000000000000000 ) ) ;
#10132 = CARTESIAN_POINT ( 'NONE',  ( 5.291489565152560637, 19.28730510418394317, 5.652196082369965069 ) ) ;
#10133 = ORIENTED_EDGE ( 'NONE', *, *, #20391, .F. ) ;
#10134 = ADVANCED_FACE ( 'NONE', ( #6280 ), #3641, .F. ) ;
#10135 = AXIS2_PLACEMENT_3D ( 'NONE', #29767, #8409, #17921 ) ;
#10136 = CARTESIAN_POINT ( 'NONE',  ( 0.3518703668723787148, -19.99690444156084723, 7.652108011868850035 ) ) ;
#10137 = CARTESIAN_POINT ( 'NONE',  ( -17.58129253318381657, -9.534052292972814868, 19.21940439362674624 ) ) ;
#10138 = CARTESIAN_POINT ( 'NONE',  ( 16.76050819728945385, 3.085824932809442700, 5.657991946698900598 ) ) ;
#10139 = EDGE_CURVE ( 'NONE', #19771, #28210, #1617, .T. ) ;
#10140 = ORIENTED_EDGE ( 'NONE', *, *, #18356, .F. ) ;
#10141 = CARTESIAN_POINT ( 'NONE',  ( 12.99901289864995668, 10.98932263627886563, 6.864725433338323413 ) ) ;
#10142 = ORIENTED_EDGE ( 'NONE', *, *, #27792, .T. ) ;
#10143 = EDGE_CURVE ( 'NONE', #14016, #4505, #26793, .T. ) ;
#10144 = CARTESIAN_POINT ( 'NONE',  ( 18.73437065802030332, -7.051821425362959417, 6.560937769032974209 ) ) ;
#10145 = CARTESIAN_POINT ( 'NONE',  ( 25.07950435457407323, 11.50806656539753270, -16.55003854064094426 ) ) ;
#10146 = CARTESIAN_POINT ( 'NONE',  ( -24.44496207165490276, 7.595930209050158588, 45.15942333309111945 ) ) ;
#10147 = ORIENTED_EDGE ( 'NONE', *, *, #10940, .F. ) ;
#10148 = EDGE_CURVE ( 'NONE', #13827, #27530, #15793, .T. ) ;
#10149 = DIRECTION ( 'NONE',  ( -0.000000000000000000, 0.000000000000000000, 1.000000000000000000 ) ) ;
#10150 = CARTESIAN_POINT ( 'NONE',  ( -27.03074382657074537, -6.449748410230988327, 42.96778633356042576 ) ) ;
#10151 = DIRECTION ( 'NONE',  ( -1.000000000000000000, 0.000000000000000000, 0.000000000000000000 ) ) ;
#10152 = DIRECTION ( 'NONE',  ( 0.000000000000000000, 0.000000000000000000, 1.000000000000000000 ) ) ;
#10153 = CARTESIAN_POINT ( 'NONE',  ( -2.338573377552018773, 39.50000000000000711, 34.80090346875804386 ) ) ;
#10154 = CARTESIAN_POINT ( 'NONE',  ( 11.01999061743883956, -16.71182566173002471, 20.34789198813115263 ) ) ;
#10155 = CARTESIAN_POINT ( 'NONE',  ( 32.14095006730908466, 14.40137518142634043, 39.78046893946842744 ) ) ;
#10156 = ORIENTED_EDGE ( 'NONE', *, *, #18537, .T. ) ;
#10157 = DIRECTION ( 'NONE',  ( -0.8412535328311804284, 0.5406408174555987767, 0.000000000000000000 ) ) ;
#10158 = AXIS2_PLACEMENT_3D ( 'NONE', #4244, #10821, #23112 ) ;
#10159 = CARTESIAN_POINT ( 'NONE',  ( -15.95709955354365484, 12.08619843917607817, 19.03762469184452755 ) ) ;
#10160 = DIRECTION ( 'NONE',  ( 1.000000000000000000, 0.000000000000000000, 0.000000000000000000 ) ) ;
#10161 = VECTOR ( 'NONE', #22056, 1000.000000000000000 ) ;
#10162 = CARTESIAN_POINT ( 'NONE',  ( 31.05675150279763130, -25.71074496668444098, 17.62049765687706682 ) ) ;
#10163 = ADVANCED_FACE ( 'NONE', ( #30297 ), #8920, .T. ) ;
#10164 = CARTESIAN_POINT ( 'NONE',  ( -47.14142842854255377, 69.79466010243307039, 59.50000000000029843 ) ) ;
#10165 = EDGE_CURVE ( 'NONE', #12790, #10393, #16405, .T. ) ;
#10166 = CARTESIAN_POINT ( 'NONE',  ( -25.10445388623454477, 25.60065097860747585, 1.500000000000000000 ) ) ;
#10167 = PLANE ( 'NONE',  #2808 ) ;
#10168 = CARTESIAN_POINT ( 'NONE',  ( -35.76344986165608475, 22.29344514668535027, -19.50000000000000355 ) ) ;
#10169 = ADVANCED_FACE ( 'NONE', ( #26494 ), #14056, .F. ) ;
#10170 = SURFACE_STYLE_FILL_AREA ( #5337 ) ;
#10171 = CARTESIAN_POINT ( 'NONE',  ( 12.18627938514990383, 35.48392282099285211, 37.50000000002605560 ) ) ;
#10172 = CARTESIAN_POINT ( 'NONE',  ( -2.185336383880142730, 8.817355867515834333, 13.22130136205108997 ) ) ;
#10173 = EDGE_LOOP ( 'NONE', ( #10576, #4623, #30126, #19213 ) ) ;
#10174 = FACE_OUTER_BOUND ( 'NONE', #12818, .T. ) ;
#10175 = ORIENTED_EDGE ( 'NONE', *, *, #28970, .F. ) ;
#10176 = CARTESIAN_POINT ( 'NONE',  ( -33.53985809055312473, -24.80926221883534311, -16.50000000000000355 ) ) ;
#10177 = CYLINDRICAL_SURFACE ( 'NONE', #9458, 9.482273699623480212 ) ;
#10178 = ORIENTED_EDGE ( 'NONE', *, *, #28576, .T. ) ;
#10179 = ORIENTED_EDGE ( 'NONE', *, *, #11860, .F. ) ;
#10180 = EDGE_CURVE ( 'NONE', #20533, #6221, #27434, .T. ) ;
#10181 = FACE_OUTER_BOUND ( 'NONE', #16828, .T. ) ;
#10182 = VERTEX_POINT ( 'NONE', #19944 ) ;
#10183 = ORIENTED_EDGE ( 'NONE', *, *, #7846, .F. ) ;
#10184 = ORIENTED_EDGE ( 'NONE', *, *, #2891, .F. ) ;
#10185 = DIRECTION ( 'NONE',  ( 1.000000000000000000, 0.000000000000000000, 0.000000000000000000 ) ) ;
#10186 = AXIS2_PLACEMENT_3D ( 'NONE', #15258, #29482, #24629 ) ;
#10187 = DIRECTION ( 'NONE',  ( 1.000000000000000000, 0.000000000000000000, 0.000000000000000000 ) ) ;
#10188 = CARTESIAN_POINT ( 'NONE',  ( 26.31094384852241319, -8.315730187098496984, -16.55003854064094426 ) ) ;
#10189 = CARTESIAN_POINT ( 'NONE',  ( -34.70577939417217550, -10.49309206032214270, 34.49999999999999289 ) ) ;
#10190 = DIRECTION ( 'NONE',  ( -0.000000000000000000, 0.000000000000000000, 1.000000000000000000 ) ) ;
#10191 = VERTEX_POINT ( 'NONE', #22576 ) ;
#10192 = CARTESIAN_POINT ( 'NONE',  ( -10.94312936609102849, -16.74105124841231529, 7.526993102356320797 ) ) ;
#10193 = FACE_OUTER_BOUND ( 'NONE', #26296, .T. ) ;
#10194 = SURFACE_SIDE_STYLE ('',( #15170 ) ) ;
#10195 = DIRECTION ( 'NONE',  ( 1.000000000000000000, 0.000000000000000000, 0.000000000000000000 ) ) ;
#10196 = ORIENTED_EDGE ( 'NONE', *, *, #17435, .T. ) ;
#10197 = EDGE_CURVE ( 'NONE', #23409, #18996, #6054, .T. ) ;
#10198 = ADVANCED_FACE ( 'NONE', ( #25233 ), #29561, .T. ) ;
#10199 = CARTESIAN_POINT ( 'NONE',  ( -3.763133143576374628, 8.268028093133407808, -1.500000000000000888 ) ) ;
#10200 = CARTESIAN_POINT ( 'NONE',  ( 18.33793066653144876, -7.982499537706464920, 18.34798005863226678 ) ) ;
#10201 = CARTESIAN_POINT ( 'NONE',  ( -6.507320782993285313, 15.78995902672676976, 6.672349528511551497 ) ) ;
#10202 = CARTESIAN_POINT ( 'NONE',  ( 11.11866356627124297, -16.64591798801203737, 5.652196082364323360 ) ) ;
#10203 = LINE ( 'NONE', #21438, #17399 ) ;
#10204 = LINE ( 'NONE', #5070, #27549 ) ;
#10205 = VERTEX_POINT ( 'NONE', #11363 ) ;
#10206 = ORIENTED_EDGE ( 'NONE', *, *, #25564, .T. ) ;
#10207 = CARTESIAN_POINT ( 'NONE',  ( 11.23874228076938842, -11.06161525231356713, 1.500000000000001332 ) ) ;
#10208 = CIRCLE ( 'NONE', #27652, 0.7500000000000006661 ) ;
#10209 = CARTESIAN_POINT ( 'NONE',  ( -50.00000000000000000, -50.00000000000000000, 12.49999999999999112 ) ) ;
#10210 = CARTESIAN_POINT ( 'NONE',  ( -13.33237335330699302, 10.61702797731129877, 5.653912893140659257 ) ) ;
#10211 = CARTESIAN_POINT ( 'NONE',  ( -0.2303554413151975844, -17.01973167556347377, 6.714907520933423690 ) ) ;
#10212 = VERTEX_POINT ( 'NONE', #18221 ) ;
#10213 = CARTESIAN_POINT ( 'NONE',  ( 16.14871318123685384, -5.543368461271793279, 18.84329447212444464 ) ) ;
#10214 = CARTESIAN_POINT ( 'NONE',  ( 37.16608720827707657, 65.00000000000000000, 97.07879600563551037 ) ) ;
#10215 = ORIENTED_EDGE ( 'NONE', *, *, #11824, .F. ) ;
#10216 = B_SPLINE_CURVE_WITH_KNOTS ( 'NONE', 3,
 ( #22752, #4341, #18089, #17943, #13867, #25102, #1558, #8435, #23369, #30242, #25419, #10756, #3745, #13570 ),
 .UNSPECIFIED., .F., .F.,
 ( 4, 2, 2, 2, 2, 2, 4 ),
 ( 2.108697328626194806E-07, 0.0004867403590529696938, 0.0009732698483730767812, 0.001459799337693183652, 0.001946328827013290956, 0.002919387805653491253, 0.003892446784293692418 ),
 .UNSPECIFIED. ) ;
#10217 = CARTESIAN_POINT ( 'NONE',  ( 7.483314773547865784, 80.00000000000000000, 50.49999999999998579 ) ) ;
#10218 = DIRECTION ( 'NONE',  ( -0.000000000000000000, -0.000000000000000000, 1.000000000000000000 ) ) ;
#10219 = CYLINDRICAL_SURFACE ( 'NONE', #16321, 15.00000000000000000 ) ;
#10220 = CARTESIAN_POINT ( 'NONE',  ( -39.02702558981775383, 2.049152216486670230, 32.23957365480787729 ) ) ;
#10221 = VERTEX_POINT ( 'NONE', #23351 ) ;
#10222 = DIRECTION ( 'NONE',  ( 0.000000000000000000, 1.000000000000000000, 0.000000000000000000 ) ) ;
#10223 = CARTESIAN_POINT ( 'NONE',  ( -37.16608720827707657, 65.00000000000000000, 97.07879600563551037 ) ) ;
#10224 = CYLINDRICAL_SURFACE ( 'NONE', #6371, 1.000000000000007772 ) ;
#10225 = EDGE_LOOP ( 'NONE', ( #18262, #24873, #20468, #2399 ) ) ;
#10226 = DIRECTION ( 'NONE',  ( -0.000000000000000000, -1.000000000000000000, -0.000000000000000000 ) ) ;
#10227 = AXIS2_PLACEMENT_3D ( 'NONE', #12991, #17985, #29986 ) ;
#10228 = CARTESIAN_POINT ( 'NONE',  ( 30.03792366816883330, 15.52577997660843145, 36.94438844912271946 ) ) ;
#10229 = ADVANCED_FACE ( 'NONE', ( #21144 ), #13700, .F. ) ;
#10230 = DIRECTION ( 'NONE',  ( 0.000000000000000000, -1.132880637372608986E-16, 1.000000000000000000 ) ) ;
#10232 = EDGE_CURVE ( 'NONE', #21461, #3179, #7320, .T. ) ;
#10231 = CARTESIAN_POINT ( 'NONE',  ( 0.000000000000000000, 0.000000000000000000, -1.500000000000000000 ) ) ;
#10233 = CARTESIAN_POINT ( 'NONE',  ( 26.36764545593177544, -31.31467416275353344, -1.500000000000000000 ) ) ;
#10234 = FACE_OUTER_BOUND ( 'NONE', #12497, .T. ) ;
#10235 = VERTEX_POINT ( 'NONE', #16340 ) ;
#10236 = DIRECTION ( 'NONE',  ( -0.000000000000000000, -0.000000000000000000, 1.000000000000000000 ) ) ;
#10237 = CARTESIAN_POINT ( 'NONE',  ( 20.71335220384823472, 27.86167394782616924, -16.50000000000000000 ) ) ;
#10238 = AXIS2_PLACEMENT_3D ( 'NONE', #25042, #19913, #10694 ) ;
#10239 = ORIENTED_EDGE ( 'NONE', *, *, #30854, .T. ) ;
#10240 = ORIENTED_EDGE ( 'NONE', *, *, #12253, .F. ) ;
#10241 = CARTESIAN_POINT ( 'NONE',  ( -4.468018643628994369, 42.23132757233521772, 19.94422659213416082 ) ) ;
#10242 = FACE_BOUND ( 'NONE', #19083, .T. ) ;
#10243 = ORIENTED_EDGE ( 'NONE', *, *, #8603, .T. ) ;
#10244 = DIRECTION ( 'NONE',  ( 1.000000000000000000, 0.000000000000000000, -0.000000000000000000 ) ) ;
#10245 = CARTESIAN_POINT ( 'NONE',  ( 14.91976180470934743, 13.34593040386456586, 18.34777357837152323 ) ) ;
#10246 = AXIS2_PLACEMENT_3D ( 'NONE', #12422, #24560, #12726 ) ;
#10247 = ORIENTED_EDGE ( 'NONE', *, *, #17534, .T. ) ;
#10248 = CARTESIAN_POINT ( 'NONE',  ( -19.77136997667518159, 3.131761183015793648, 7.429667576816606278 ) ) ;
#10249 = DIRECTION ( 'NONE',  ( 0.000000000000000000, 0.000000000000000000, 1.000000000000000000 ) ) ;
#10250 = VECTOR ( 'NONE', #7347, 1000.000000000000000 ) ;
#10251 = CARTESIAN_POINT ( 'NONE',  ( 40.22845766574619830, 5.865279063056531683, -16.50000000000000000 ) ) ;
#10252 = VERTEX_POINT ( 'NONE', #18675 ) ;
#10253 = DIRECTION ( 'NONE',  ( 0.000000000000000000, 0.000000000000000000, 1.000000000000000000 ) ) ;
#10254 = AXIS2_PLACEMENT_3D ( 'NONE', #30020, #5850, #13498 ) ;
#10255 = EDGE_LOOP ( 'NONE', ( #30776, #427, #10416, #6337, #25171, #18383 ) ) ;
#10256 = CARTESIAN_POINT ( 'NONE',  ( 0.000000000000000000, 1.699320956058915452E-16, -1.500000000000001776 ) ) ;
#10257 = AXIS2_PLACEMENT_3D ( 'NONE', #18641, #6773, #8820 ) ;
#10258 = VERTEX_POINT ( 'NONE', #22887 ) ;
#10259 = CARTESIAN_POINT ( 'NONE',  ( 37.60443094512424977, -11.34029379291156836, 31.81961544519251106 ) ) ;
#10260 = CARTESIAN_POINT ( 'NONE',  ( 16.56029649016585026, 4.170884463583997892, 6.892848776733236704 ) ) ;
#10261 = LINE ( 'NONE', #28844, #6159 ) ;
#10262 = CARTESIAN_POINT ( 'NONE',  ( -26.36764545593177900, 31.31467416275353344, 1.500000000000000000 ) ) ;
#10263 = VECTOR ( 'NONE', #18682, 1000.000000000000000 ) ;
#10264 = CARTESIAN_POINT ( 'NONE',  ( -39.07074351764322984, -0.08311056096719925124, 32.25448628877133217 ) ) ;
#10265 = CARTESIAN_POINT ( 'NONE',  ( 0.000000000000000000, 42.50000000000000000, 32.26246401786215046 ) ) ;
#10266 = EDGE_CURVE ( 'NONE', #9621, #28625, #30070, .T. ) ;
#10267 = DIRECTION ( 'NONE',  ( 0.000000000000000000, -0.000000000000000000, 1.000000000000000000 ) ) ;
#10268 = ORIENTED_EDGE ( 'NONE', *, *, #25874, .T. ) ;
#10269 = EDGE_CURVE ( 'NONE', #26065, #2425, #8866, .T. ) ;
#10271 = AXIS2_PLACEMENT_3D ( 'NONE', #26258, #5514, #14868 ) ;
#10270 = CARTESIAN_POINT ( 'NONE',  ( -19.88823125026085492, 2.273432466552572695, 5.678370764302467677 ) ) ;
#10272 = FACE_OUTER_BOUND ( 'NONE', #6904, .T. ) ;
#10273 = AXIS2_PLACEMENT_3D ( 'NONE', #5891, #10571, #29135 ) ;
#10274 = CARTESIAN_POINT ( 'NONE',  ( 9.216505592218814158, -7.781333699927420966, 1.500000000000000000 ) ) ;
#10275 = CARTESIAN_POINT ( 'NONE',  ( 0.000000000000000000, 90.00000000000001421, 0.000000000000000000 ) ) ;
#10276 = ORIENTED_EDGE ( 'NONE', *, *, #10523, .T. ) ;
#10277 = ORIENTED_EDGE ( 'NONE', *, *, #20457, .F. ) ;
#10278 = CARTESIAN_POINT ( 'NONE',  ( 47.00000000000044764, -4.926614671774132148E-13, 79.49999999999998579 ) ) ;
#10279 = CARTESIAN_POINT ( 'NONE',  ( 43.34097750826428097, 11.89502811014149763, 1.500000000000000444 ) ) ;
#10280 = LINE ( 'NONE', #15111, #18360 ) ;
#10281 = ORIENTED_EDGE ( 'NONE', *, *, #27310, .T. ) ;
#10282 = CARTESIAN_POINT ( 'NONE',  ( -15.57728904105047718, -6.860944617588216943, 6.519181285484531685 ) ) ;
#10283 = AXIS2_PLACEMENT_3D ( 'NONE', #28036, #11655, #25697 ) ;
#10284 = DIRECTION ( 'NONE',  ( 0.000000000000000000, 0.000000000000000000, 1.000000000000000000 ) ) ;
#10285 = AXIS2_PLACEMENT_3D ( 'NONE', #26403, #5029, #22015 ) ;
#10286 = CARTESIAN_POINT ( 'NONE',  ( -31.92585768968024595, -26.59981599184672518, -13.16665969293629423 ) ) ;
#10287 = ORIENTED_EDGE ( 'NONE', *, *, #24013, .F. ) ;
#10288 = CARTESIAN_POINT ( 'NONE',  ( -9.660978277356432997, -17.51194513905170069, 19.61564845152805248 ) ) ;
#10289 = AXIS2_PLACEMENT_3D ( 'NONE', #16292, #30621, #9267 ) ;
#10290 = LINE ( 'NONE', #310, #1749 ) ;
#10291 = CARTESIAN_POINT ( 'NONE',  ( 16.77888236039448344, 2.967719242317201633, 7.632642797338977658 ) ) ;
#10292 = VERTEX_POINT ( 'NONE', #30519 ) ;
#10293 = CIRCLE ( 'NONE', #2817, 15.00000000000000000 ) ;
#10294 = CARTESIAN_POINT ( 'NONE',  ( 12.98391214946238748, 11.00790965981589586, 6.974106381145714018 ) ) ;
#10295 = ORIENTED_EDGE ( 'NONE', *, *, #14370, .T. ) ;
#10296 = CARTESIAN_POINT ( 'NONE',  ( 18.69797757513550351, -7.147916136757723748, 7.098451512883313441 ) ) ;
#10297 = VECTOR ( 'NONE', #15677, 1000.000000000000227 ) ;
#10298 = DIRECTION ( 'NONE',  ( -0.000000000000000000, -0.000000000000000000, -1.000000000000000000 ) ) ;
#10299 = CIRCLE ( 'NONE', #29742, 9.482273699623480212 ) ;
#10300 = ORIENTED_EDGE ( 'NONE', *, *, #23080, .F. ) ;
#10301 = ADVANCED_FACE ( 'NONE', ( #13552, #16180, #25855 ), #5311, .F. ) ;
#10302 = CARTESIAN_POINT ( 'NONE',  ( 9.755064781586030520, 13.32952022457704544, 24.50000000000000000 ) ) ;
#10303 = CARTESIAN_POINT ( 'NONE',  ( -4.776122516674677878E-15, -42.50000000000000000, 19.72227980406325543 ) ) ;
#10304 = EDGE_LOOP ( 'NONE', ( #944, #273, #18809, #13084 ) ) ;
#10305 = CARTESIAN_POINT ( 'NONE',  ( 31.29501345866090389, 26.27841684422296353, -6.500000000000000888 ) ) ;
#10306 = ADVANCED_FACE ( 'NONE', ( #18390 ), #30323, .T. ) ;
#10307 = SHAPE_REPRESENTATION ( 'hex bolt gradeab_iso_ISO 4014 - M12 x 120 x 30-N', ( #7396 ), #3935 ) ;
#10308 = LINE ( 'NONE', #27162, #8923 ) ;
#10309 = CARTESIAN_POINT ( 'NONE',  ( 0.000000000000000000, -2.435693370351110282E-15, 21.50000000000000355 ) ) ;
#10310 = CARTESIAN_POINT ( 'NONE',  ( 33.56327786402390245, 10.34181101807379299, 39.87954049117193023 ) ) ;
#10311 = VERTEX_POINT ( 'NONE', #2453 ) ;
#10312 = EDGE_CURVE ( 'NONE', #16079, #5009, #26148, .T. ) ;
#10313 = CARTESIAN_POINT ( 'NONE',  ( -26.12638453225887503, -6.310846377660610962, 48.12226976367811204 ) ) ;
#10314 = AXIS2_PLACEMENT_3D ( 'NONE', #27217, #19579, #30131 ) ;
#10315 = CARTESIAN_POINT ( 'NONE',  ( -12.56641067637752229, 40.32935944495016400, -1.500000000000000000 ) ) ;
#10316 = CARTESIAN_POINT ( 'NONE',  ( 47.14142842854284510, 69.79466010243311302, 59.49999999999998579 ) ) ;
#10317 = AXIS2_PLACEMENT_3D ( 'NONE', #2088, #28462, #14569 ) ;
#10318 = CARTESIAN_POINT ( 'NONE',  ( 29.06906351934491184, -28.33367601428275151, 9.889412824572042737 ) ) ;
#10320 = EDGE_CURVE ( 'NONE', #21915, #27180, #9295, .T. ) ;
#10319 = DIRECTION ( 'NONE',  ( -5.125319360840571077E-16, 1.000000000000000000, 0.000000000000000000 ) ) ;
#10321 = DIRECTION ( 'NONE',  ( -1.000000000000000000, 0.000000000000000000, 0.000000000000000000 ) ) ;
#10322 = DIRECTION ( 'NONE',  ( -0.000000000000000000, -0.000000000000000000, 1.000000000000000000 ) ) ;
#10323 = CIRCLE ( 'NONE', #22271, 12.66227964008302287 ) ;
#10324 = CARTESIAN_POINT ( 'NONE',  ( 39.00000000000000000, 5.563236990218597633, -1.500000000000000000 ) ) ;
#10325 = EDGE_CURVE ( 'NONE', #1559, #25155, #4778, .T. ) ;
#10326 = DIRECTION ( 'NONE',  ( 0.000000000000000000, 0.000000000000000000, 1.000000000000000000 ) ) ;
#10327 = EDGE_CURVE ( 'NONE', #1600, #20446, #16947, .T. ) ;
#10328 = CARTESIAN_POINT ( 'NONE',  ( 16.87925085231059441, 2.194398682741079298, 6.519181285484532573 ) ) ;
#10329 = AXIS2_PLACEMENT_3D ( 'NONE', #22877, #30369, #3714 ) ;
#10330 = CARTESIAN_POINT ( 'NONE',  ( 19.59736455876165806, 3.994007928088042281, 6.037995405461185072 ) ) ;
#10331 = ORIENTED_EDGE ( 'NONE', *, *, #96, .F. ) ;
#10332 = AXIS2_PLACEMENT_3D ( 'NONE', #1269, #11398, #27319 ) ;
#10333 = CARTESIAN_POINT ( 'NONE',  ( 26.31795596221988376, 10.51822134874671022, 1.500000000000000000 ) ) ;
#10334 = ORIENTED_EDGE ( 'NONE', *, *, #20800, .T. ) ;
#10335 = AXIS2_PLACEMENT_3D ( 'NONE', #16880, #28734, #5176 ) ;
#10336 = FACE_OUTER_BOUND ( 'NONE', #28192, .T. ) ;
#10337 = FACE_OUTER_BOUND ( 'NONE', #28602, .T. ) ;
#10338 = EDGE_LOOP ( 'NONE', ( #26731, #3758, #23380, #12548, #28552 ) ) ;
#10339 = ORIENTED_EDGE ( 'NONE', *, *, #10108, .T. ) ;
#10340 = CIRCLE ( 'NONE', #25280, 10.00000000000000000 ) ;
#10341 = DIRECTION ( 'NONE',  ( -0.000000000000000000, 0.000000000000000000, 1.000000000000000000 ) ) ;
#10342 = VECTOR ( 'NONE', #443, 1000.000000000000000 ) ;
#10343 = ORIENTED_EDGE ( 'NONE', *, *, #4835, .F. ) ;
#10344 = CARTESIAN_POINT ( 'NONE',  ( 2.959227181723801170, -8.499586724479446076, 21.50000000000000000 ) ) ;
#10345 = AXIS2_PLACEMENT_3D ( 'NONE', #26932, #3363, #1031 ) ;
#10346 = EDGE_CURVE ( 'NONE', #13230, #3110, #7808, .T. ) ;
#10347 = CARTESIAN_POINT ( 'NONE',  ( -32.99407928578143867, 15.80558523611060018, 34.49999999999998579 ) ) ;
#10348 = EDGE_CURVE ( 'NONE', #26161, #26600, #28808, .T. ) ;
#10349 = CARTESIAN_POINT ( 'NONE',  ( -14.41708049311053053, 17.22181377296911720, -1.500000000000000000 ) ) ;
#10350 = CARTESIAN_POINT ( 'NONE',  ( -37.68891294954676141, 10.93031833424447363, 14.71512993969763450 ) ) ;
#10351 = CARTESIAN_POINT ( 'NONE',  ( -20.58367780861512841, 27.52817754551177032, -16.50001200000000168 ) ) ;
#10352 = ORIENTED_EDGE ( 'NONE', *, *, #15708, .T. ) ;
#10353 = ADVANCED_FACE ( 'NONE', ( #12439, #4635 ), #14136, .T. ) ;
#10354 = CARTESIAN_POINT ( 'NONE',  ( 26.36764545593177544, -31.31467416275353344, 1.500000000000000000 ) ) ;
#10355 = CARTESIAN_POINT ( 'NONE',  ( -13.68208811019134785, -10.53240720452297374, -0.6213203435596476032 ) ) ;
#10356 = FACE_OUTER_BOUND ( 'NONE', #24128, .T. ) ;
#10357 = AXIS2_PLACEMENT_3D ( 'NONE', #1442, #30273, #20304 ) ;
#10358 = ORIENTED_EDGE ( 'NONE', *, *, #24207, .F. ) ;
#10359 = ADVANCED_FACE ( 'NONE', ( #21309 ), #27401, .T. ) ;
#10360 = AXIS2_PLACEMENT_3D ( 'NONE', #23682, #9358, #9982 ) ;
#10361 = AXIS2_PLACEMENT_3D ( 'NONE', #77, #4908, #23606 ) ;
#10362 = DIRECTION ( 'NONE',  ( -1.000000000000000000, 0.000000000000000000, 0.000000000000000000 ) ) ;
#10363 = CARTESIAN_POINT ( 'NONE',  ( -40.00000000000000000, 87.00000000000001421, 52.49999999999999289 ) ) ;
#10364 = CARTESIAN_POINT ( 'NONE',  ( 11.81973518349029284, -16.15564139912475028, 7.196036389296800451 ) ) ;
#10365 = EDGE_CURVE ( 'NONE', #1662, #24166, #17760, .T. ) ;
#10366 = CARTESIAN_POINT ( 'NONE',  ( -35.76344986165604212, -22.29344514668547461, -19.50000000000000355 ) ) ;
#10367 = DIRECTION ( 'NONE',  ( 1.000000000000000000, 0.000000000000000000, -0.000000000000000000 ) ) ;
#10368 = AXIS2_PLACEMENT_3D ( 'NONE', #17556, #27074, #15194 ) ;
#10369 = ORIENTED_EDGE ( 'NONE', *, *, #5973, .F. ) ;
#10370 = ORIENTED_EDGE ( 'NONE', *, *, #23180, .T. ) ;
#10371 = AXIS2_PLACEMENT_3D ( 'NONE', #23107, #13479, #6127 ) ;
#10372 = FACE_OUTER_BOUND ( 'NONE', #17669, .T. ) ;
#10373 = CARTESIAN_POINT ( 'NONE',  ( 8.606594496258196614, 4.390207617113981442, 1.500000000000001332 ) ) ;
#10374 = CARTESIAN_POINT ( 'NONE',  ( 2.161275096740449708, -37.44220553068277724, 37.50000000000981260 ) ) ;
#10375 = CARTESIAN_POINT ( 'NONE',  ( 0.2718907111903831053, -17.03030470364403470, 7.526951045817045660 ) ) ;
#10376 = ORIENTED_EDGE ( 'NONE', *, *, #21027, .F. ) ;
#10377 = CARTESIAN_POINT ( 'NONE',  ( -2.810445847081919357, -9.056208293496299078, 21.50000000000000000 ) ) ;
#10378 = DIRECTION ( 'NONE',  ( 1.000000000000000000, 0.000000000000000000, 0.000000000000000000 ) ) ;
#10379 = VECTOR ( 'NONE', #13711, 1000.000000000000000 ) ;
#10380 = EDGE_CURVE ( 'NONE', #16368, #9274, #21732, .T. ) ;
#10381 = ORIENTED_EDGE ( 'NONE', *, *, #27045, .F. ) ;
#10382 = CARTESIAN_POINT ( 'NONE',  ( 4.806943871629679066, 16.33324523791881688, 18.71435384576123440 ) ) ;
#10383 = B_SPLINE_SURFACE_WITH_KNOTS ( 'NONE', 3, 1, ( 
 ( #17288, #24460 ),
 ( #26346, #7623 ),
 ( #7778, #26821 ),
 ( #12309, #21811 ),
 ( #9971, #5446 ),
 ( #5283, #12153 ),
 ( #12769, #10111 ),
 ( #14949, #135 ),
 ( #3103, #7322 ),
 ( #9655, #21652 ),
 ( #19475, #16831 ),
 ( #17130, #19321 ),
 ( #12622, #7478 ),
 ( #26652, #14790 ),
 ( #22115, #19775 ),
 ( #24307, #16976 ),
 ( #29307, #19621 ),
 ( #7948, #4975 ),
 ( #286, #9809 ),
 ( #12475, #21965 ),
 ( #593, #27272 ),
 ( #8246, #29928 ),
 ( #15404, #13241 ),
 ( #5903, #6212 ),
 ( #914, #27121 ),
 ( #11473, #1386 ),
 ( #20095, #8566 ),
 ( #29463, #10431 ),
 ( #13088, #23311 ),
 ( #22729, #16298 ),
 ( #27586, #19945 ) ),
 .UNSPECIFIED., .F., .F., .F.,
 ( 4, 3, 3, 3, 3, 3, 3, 3, 3, 3, 4 ),
 ( 2, 2 ),
 ( 0.000000000000000000, 0.05425176834609614362, 0.1085332949128348518, 0.1623767749169379715, 0.2157504826133058717, 0.2688657508888169789, 0.3218907763505471364, 0.3749548578363334772, 0.4282048033836237666, 0.4818374082110496448, 0.4999999999131653494 ),
 ( 0.000000000000000000, 1.000000000000000000 ),
 .UNSPECIFIED. ) ;
#10384 = CIRCLE ( 'NONE', #4895, 0.7500000000000006661 ) ;
#10385 = EDGE_CURVE ( 'NONE', #3354, #16254, #22688, .T. ) ;
#10386 = CARTESIAN_POINT ( 'NONE',  ( -33.10232066993145139, -22.48641252920058164, 34.66925410237854521 ) ) ;
#10387 = ORIENTED_EDGE ( 'NONE', *, *, #26720, .F. ) ;
#10388 = DIRECTION ( 'NONE',  ( 0.000000000000000000, 0.000000000000000000, 1.000000000000000000 ) ) ;
#10389 = DIRECTION ( 'NONE',  ( 0.1423148382732889461, 0.9898214418809321291, 0.000000000000000000 ) ) ;
#10390 = LINE ( 'NONE', #29422, #17839 ) ;
#10391 = CIRCLE ( 'NONE', #8904, 7.500000000000000000 ) ;
#10392 = CARTESIAN_POINT ( 'NONE',  ( 0.000000000000000000, 0.000000000000000000, -52.50000000000000000 ) ) ;
#10393 = VERTEX_POINT ( 'NONE', #3216 ) ;
#10394 = APPLICATION_CONTEXT ( 'automotive_design' ) ;
#10395 = DIRECTION ( 'NONE',  ( 1.000000000000000000, 0.000000000000000000, 0.000000000000000000 ) ) ;
#10396 = LINE ( 'NONE', #8368, #27337 ) ;
#10397 = CARTESIAN_POINT ( 'NONE',  ( 16.01701959600647385, -5.879758784200290300, 7.545655578832112020 ) ) ;
#10398 = CARTESIAN_POINT ( 'NONE',  ( 8.413215745754998309, -3.196529495465417980, 1.500000000000001332 ) ) ;
#10399 = CARTESIAN_POINT ( 'NONE',  ( -40.48935727530044915, 2.936718089577218915, -16.50000000000000355 ) ) ;
#10400 = CARTESIAN_POINT ( 'NONE',  ( 3.637110358602582583, 19.99473753024312117, -1.500000000000000000 ) ) ;
#10401 = DIRECTION ( 'NONE',  ( -0.000000000000000000, 0.000000000000000000, -1.000000000000000000 ) ) ;
#10402 = PLANE ( 'NONE',  #2951 ) ;
#10403 = ORIENTED_EDGE ( 'NONE', *, *, #18176, .F. ) ;
#10404 =( GEOMETRIC_REPRESENTATION_CONTEXT ( 3 ) GLOBAL_UNCERTAINTY_ASSIGNED_CONTEXT ( ( #5157 ) ) GLOBAL_UNIT_ASSIGNED_CONTEXT ( ( #433, #29741, #20384 ) ) REPRESENTATION_CONTEXT ( 'NONE', 'WORKASPACE' ) );
#10405 = AXIS2_PLACEMENT_3D ( 'NONE', #24178, #18750, #28267 ) ;
#10406 = FACE_OUTER_BOUND ( 'NONE', #9631, .T. ) ;
#10407 = FACE_OUTER_BOUND ( 'NONE', #8883, .T. ) ;
#10408 = CIRCLE ( 'NONE', #13877, 20.00000000000000000 ) ;
#10409 = VERTEX_POINT ( 'NONE', #22543 ) ;
#10410 = AXIS2_PLACEMENT_3D ( 'NONE', #22944, #25295, #6263 ) ;
#10411 = ORIENTED_EDGE ( 'NONE', *, *, #14353, .F. ) ;
#10412 = CARTESIAN_POINT ( 'NONE',  ( 7.869584159753955532, 10.39565510934977333, 1.500000000000001332 ) ) ;
#10413 = DIRECTION ( 'NONE',  ( 0.000000000000000000, -1.132880637372608986E-16, 1.000000000000000000 ) ) ;
#10414 = DIRECTION ( 'NONE',  ( -0.000000000000000000, 0.000000000000000000, 1.000000000000000000 ) ) ;
#10415 = CARTESIAN_POINT ( 'NONE',  ( 15.49551216414738875, 12.67315350590407697, 19.77662771831109367 ) ) ;
#10416 = ORIENTED_EDGE ( 'NONE', *, *, #24566, .F. ) ;
#10417 = ORIENTED_EDGE ( 'NONE', *, *, #1909, .F. ) ;
#10418 = CARTESIAN_POINT ( 'NONE',  ( 12.50000000000000000, 1.530808498934191521E-15, -87.50000000000000000 ) ) ;
#10419 = CARTESIAN_POINT ( 'NONE',  ( 17.96625477203413723, -8.787278772463418264, 7.156831654632803463 ) ) ;
#10420 = DIRECTION ( 'NONE',  ( 1.000000000000000000, 0.000000000000000000, 0.000000000000000000 ) ) ;
#10421 = VERTEX_POINT ( 'NONE', #876 ) ;
#10422 = CARTESIAN_POINT ( 'NONE',  ( -5.738360882150000286, -7.548823014270624299, 21.50000000000000000 ) ) ;
#10423 = ORIENTED_EDGE ( 'NONE', *, *, #16806, .F. ) ;
#10424 = CARTESIAN_POINT ( 'NONE',  ( 0.000000000000000000, 0.000000000000000000, 1.500000000000001332 ) ) ;
#10425 = AXIS2_PLACEMENT_3D ( 'NONE', #1657, #25972, #4598 ) ;
#10426 = AXIS2_PLACEMENT_3D ( 'NONE', #13030, #6304, #27676 ) ;
#10427 = VERTEX_POINT ( 'NONE', #24728 ) ;
#10428 = CARTESIAN_POINT ( 'NONE',  ( -6.813581335325351596, 18.80366338534911463, 18.84486140012300126 ) ) ;
#10429 = DIRECTION ( 'NONE',  ( 0.000000000000000000, 1.000000000000000000, 0.000000000000000000 ) ) ;
#10430 = CARTESIAN_POINT ( 'NONE',  ( 19.60273500773784505, 4.055073576757204812, 6.131018562779544823 ) ) ;
#10431 = CARTESIAN_POINT ( 'NONE',  ( -13.30790957887532500, 10.64596135573642144, 18.35377592296120497 ) ) ;
#10432 = AXIS2_PLACEMENT_3D ( 'NONE', #24792, #3429, #29327 ) ;
#10433 = FACE_OUTER_BOUND ( 'NONE', #20773, .T. ) ;
#10434 = CARTESIAN_POINT ( 'NONE',  ( -5.145204076156935535, 42.13436674946195382, 28.87129565651644825 ) ) ;
#10435 = LINE ( 'NONE', #2962, #17992 ) ;
#10436 = CARTESIAN_POINT ( 'NONE',  ( -2.523760598493608232, -1.621922452366769907, 24.50000000000000000 ) ) ;
#10437 = ORIENTED_EDGE ( 'NONE', *, *, #6494, .T. ) ;
#10438 = CARTESIAN_POINT ( 'NONE',  ( 9.769531821641358249, -13.96399651007160791, 5.657991946698900598 ) ) ;
#10439 = CIRCLE ( 'NONE', #24891, 7.500000000000000000 ) ;
#10440 = CARTESIAN_POINT ( 'NONE',  ( 28.98606489759778881, -23.42647331253649412, 34.50000000000000000 ) ) ;
#10441 = CARTESIAN_POINT ( 'NONE',  ( -42.49999999999998579, -50.00000000000000000, 12.49999999999999112 ) ) ;
#10442 = VERTEX_POINT ( 'NONE', #12902 ) ;
#10443 = ORIENTED_EDGE ( 'NONE', *, *, #1622, .F. ) ;
#10444 = CARTESIAN_POINT ( 'NONE',  ( -11.40980092660686829, 6.310027164379044429, 1.500000000000001332 ) ) ;
#10445 = CARTESIAN_POINT ( 'NONE',  ( -22.58267429318971864, 26.57182937991348481, 1.500000000000001332 ) ) ;
#10446 = DIRECTION ( 'NONE',  ( 0.000000000000000000, 0.000000000000000000, 1.000000000000000000 ) ) ;
#10447 = ORIENTED_EDGE ( 'NONE', *, *, #25245, .F. ) ;
#10448 = LINE ( 'NONE', #20114, #12090 ) ;
#10449 = DIRECTION ( 'NONE',  ( -1.000000000000000000, 0.000000000000000000, 0.000000000000000000 ) ) ;
#10450 = DIRECTION ( 'NONE',  ( -1.000000000000000000, 0.000000000000000000, 0.000000000000000000 ) ) ;
#10451 = ORIENTED_EDGE ( 'NONE', *, *, #2165, .T. ) ;
#10452 = CARTESIAN_POINT ( 'NONE',  ( 49.99999999999998579, 50.00000000000000000, 62.49999999999999289 ) ) ;
#10453 = CIRCLE ( 'NONE', #17428, 32.32717498572574755 ) ;
#10454 = CARTESIAN_POINT ( 'NONE',  ( 14.89413573707701488, 13.37445272932972706, 5.652196082364320695 ) ) ;
#10455 = CARTESIAN_POINT ( 'NONE',  ( 19.89210292178043460, 2.240810012149825781, 6.974106381145714018 ) ) ;
#10456 = EDGE_LOOP ( 'NONE', ( #28585, #11923, #20364, #22868, #28157, #20973, #27645 ) ) ;
#10457 = CARTESIAN_POINT ( 'NONE',  ( 12.77210943289888334, 11.26383436979580921, 5.862424720655265098 ) ) ;
#10458 = ORIENTED_EDGE ( 'NONE', *, *, #20999, .F. ) ;
#10459 = CARTESIAN_POINT ( 'NONE',  ( 10.18506332983505303, 29.04537757311072710, 1.500000000000001332 ) ) ;
#10460 = CARTESIAN_POINT ( 'NONE',  ( 0.000000000000000000, 1.699320956058915452E-16, -1.500000000000001776 ) ) ;
#10461 = MECHANICAL_DESIGN_GEOMETRIC_PRESENTATION_REPRESENTATION (  '', ( #6476 ), #22412 ) ;
#10462 = ORIENTED_EDGE ( 'NONE', *, *, #20024, .T. ) ;
#10463 = CARTESIAN_POINT ( 'NONE',  ( 3.905960108394948449, 16.59621863701448419, 7.643931100913408550 ) ) ;
#10464 = FACE_OUTER_BOUND ( 'NONE', #14775, .T. ) ;
#10465 = DIRECTION ( 'NONE',  ( 0.000000000000000000, -0.000000000000000000, -1.000000000000000000 ) ) ;
#10466 = EDGE_CURVE ( 'NONE', #29559, #11919, #8812, .T. ) ;
#10467 = CARTESIAN_POINT ( 'NONE',  ( 13.79614740859419797, 36.49939583300671586, 34.49999999999999289 ) ) ;
#10468 = CARTESIAN_POINT ( 'NONE',  ( -27.03943647958860552, 26.20092231554396633, 27.50000000000001066 ) ) ;
#10469 = LINE ( 'NONE', #29348, #14797 ) ;
#10470 = CARTESIAN_POINT ( 'NONE',  ( 33.55235357430897380, 10.58403138555777900, 39.81808279656205229 ) ) ;
#10471 = ORIENTED_EDGE ( 'NONE', *, *, #214, .T. ) ;
#10472 = DIRECTION ( 'NONE',  ( 0.000000000000000000, 0.000000000000000000, 1.000000000000000000 ) ) ;
#10473 = AXIS2_PLACEMENT_3D ( 'NONE', #19502, #2347, #29013 ) ;
#10474 = CARTESIAN_POINT ( 'NONE',  ( -15.98738144660410931, 12.04609795553197671, 19.36813350477385143 ) ) ;
#10475 = CARTESIAN_POINT ( 'NONE',  ( 40.49651552764380114, 64.44451528374314364, 62.49999999999998579 ) ) ;
#10476 = DIRECTION ( 'NONE',  ( 1.000000000000000000, 0.000000000000000000, 0.000000000000000000 ) ) ;
#10477 = ORIENTED_EDGE ( 'NONE', *, *, #13222, .T. ) ;
#10478 = CARTESIAN_POINT ( 'NONE',  ( 28.55449552082023601, -28.94826332574320560, 15.31987994115628737 ) ) ;
#10479 = DIRECTION ( 'NONE',  ( 0.000000000000000000, -1.000000000000000000, 0.000000000000000000 ) ) ;
#10480 = CARTESIAN_POINT ( 'NONE',  ( -24.18511243334008043, -13.30669973338235401, 47.39588261142744585 ) ) ;
#10481 = DIRECTION ( 'NONE',  ( -0.000000000000000000, 0.000000000000000000, -1.000000000000000000 ) ) ;
#10482 = DIRECTION ( 'NONE',  ( 1.000000000000000000, 0.000000000000000000, 0.000000000000000000 ) ) ;
#10483 = VECTOR ( 'NONE', #2845, 1000.000000000000000 ) ;
#10484 = EDGE_CURVE ( 'NONE', #9423, #12881, #14917, .T. ) ;
#10485 = FACE_OUTER_BOUND ( 'NONE', #7798, .T. ) ;
#10486 = CARTESIAN_POINT ( 'NONE',  ( 4.216636297896264374, 37.26217892624189432, 37.50000000000000000 ) ) ;
#10487 = PRODUCT_DEFINITION ( 'UNKNOWN', '', #23347, #8896 ) ;
#10488 = ORIENTED_EDGE ( 'NONE', *, *, #30575, .F. ) ;
#10489 = CARTESIAN_POINT ( 'NONE',  ( 25.88640477275122365, 6.345529225273955021, 44.10491087709814906 ) ) ;
#10490 = CARTESIAN_POINT ( 'NONE',  ( -6.812559277181930106, 5.881244434206302607, -1.500000000000000888 ) ) ;
#10491 = CARTESIAN_POINT ( 'NONE',  ( 25.64627119138473432, -23.40052582045089480, -16.50000000000000000 ) ) ;
#10492 = ORIENTED_EDGE ( 'NONE', *, *, #10545, .T. ) ;
#10493 = ORIENTED_EDGE ( 'NONE', *, *, #19324, .T. ) ;
#10494 = DIRECTION ( 'NONE',  ( -0.000000000000000000, 0.000000000000000000, 1.000000000000000000 ) ) ;
#10495 = ADVANCED_FACE ( 'NONE', ( #20368 ), #27232, .F. ) ;
#10496 = AXIS2_PLACEMENT_3D ( 'NONE', #11675, #12298, #19312 ) ;
#10497 = SHAPE_REPRESENTATION ( 'Rotor', ( #7396 ), #26315 ) ;
#10498 = VERTEX_POINT ( 'NONE', #29428 ) ;
#10499 = DIRECTION ( 'NONE',  ( 0.000000000000000000, 0.000000000000000000, 1.000000000000000000 ) ) ;
#10500 = CARTESIAN_POINT ( 'NONE',  ( -34.45952885238020258, 11.47311510027356007, 34.50000000000000711 ) ) ;
#10501 = DIRECTION ( 'NONE',  ( 1.000000000000000000, 0.000000000000000000, 0.000000000000000000 ) ) ;
#10502 = CARTESIAN_POINT ( 'NONE',  ( -36.42579814062143129, 15.19756091628274319, 16.64139166720004326 ) ) ;
#10503 = EDGE_CURVE ( 'NONE', #15984, #20557, #22079, .T. ) ;
#10504 = DIRECTION ( 'NONE',  ( 1.000000000000000000, 0.000000000000000000, 0.000000000000000000 ) ) ;
#10505 = ADVANCED_FACE ( 'NONE', ( #3371 ), #15367, .F. ) ;
#10506 = DIRECTION ( 'NONE',  ( 0.000000000000000000, 0.000000000000000000, 1.000000000000000000 ) ) ;
#10507 = CARTESIAN_POINT ( 'NONE',  ( -52.16608720827707657, -36.86186943028246787, 97.07879600563551037 ) ) ;
#10508 =( NAMED_UNIT ( * ) PLANE_ANGLE_UNIT ( ) SI_UNIT ( $, .RADIAN. ) );
#10509 = DIRECTION ( 'NONE',  ( -1.000000000000000000, 0.000000000000000000, 0.000000000000000000 ) ) ;
#10510 = EDGE_LOOP ( 'NONE', ( #28794, #20341, #21478, #7944 ) ) ;
#10511 = DIRECTION ( 'NONE',  ( 0.000000000000000000, 1.132880637372608986E-16, -1.000000000000000000 ) ) ;
#10512 = CARTESIAN_POINT ( 'NONE',  ( -6.145639756558239242, 15.91995507688107736, 7.441806358946449151 ) ) ;
#10513 = CARTESIAN_POINT ( 'NONE',  ( 10.69227409735890078, -13.31703061742499017, 6.672349528511551497 ) ) ;
#10514 = FACE_OUTER_BOUND ( 'NONE', #17944, .T. ) ;
#10515 = AXIS2_PLACEMENT_3D ( 'NONE', #16035, #29617, #8712 ) ;
#10516 = CARTESIAN_POINT ( 'NONE',  ( 33.55224573311710401, -10.10291939066352640, 35.71721447083890411 ) ) ;
#10517 = ORIENTED_EDGE ( 'NONE', *, *, #10380, .F. ) ;
#10518 = ORIENTED_EDGE ( 'NONE', *, *, #28987, .T. ) ;
#10519 = CARTESIAN_POINT ( 'NONE',  ( 14.44122519041005681, -13.83658248990206729, 24.50000000000000000 ) ) ;
#10520 = CARTESIAN_POINT ( 'NONE',  ( -5.374868878256215510, -44.10336124695545124, -19.50000000000000355 ) ) ;
#10521 = EDGE_CURVE ( 'NONE', #23899, #30628, #3534, .T. ) ;
#10522 = CARTESIAN_POINT ( 'NONE',  ( 5.068365686548764515, -37.22901435740217124, 37.49999999996078515 ) ) ;
#10523 = EDGE_CURVE ( 'NONE', #26276, #6382, #26784, .T. ) ;
#10524 = DIRECTION ( 'NONE',  ( 0.8910248307962433945, -0.4539545692076750738, 0.000000000000000000 ) ) ;
#10525 = ORIENTED_EDGE ( 'NONE', *, *, #1052, .T. ) ;
#10526 = CONTEXT_DEPENDENT_SHAPE_REPRESENTATION ( #24724, #2971 ) ;
#10527 = CARTESIAN_POINT ( 'NONE',  ( 3.062151163506454665, 16.80153468414595253, 6.588756557121049795 ) ) ;
#10528 = ADVANCED_FACE ( 'NONE', ( #5867 ), #29577, .F. ) ;
#10529 = CARTESIAN_POINT ( 'NONE',  ( 42.49999999999998579, 50.00000000000000000, 97.07879600563551037 ) ) ;
#10530 = ORIENTED_EDGE ( 'NONE', *, *, #2658, .F. ) ;
#10531 = CARTESIAN_POINT ( 'NONE',  ( 5.335947603960575769, 19.29354331951100576, 18.34777357837151612 ) ) ;
#10532 = EDGE_CURVE ( 'NONE', #9285, #7702, #12589, .T. ) ;
#10533 = CARTESIAN_POINT ( 'NONE',  ( 0.09252763182293005650, -6.914127053141865709, 6.024380653971853405 ) ) ;
#10534 = CARTESIAN_POINT ( 'NONE',  ( -36.28305795128277111, -9.498090346893212299, 37.50000000001156053 ) ) ;
#10535 = ORIENTED_EDGE ( 'NONE', *, *, #10890, .T. ) ;
#10536 = EDGE_CURVE ( 'NONE', #22024, #15589, #27223, .T. ) ;
#10537 = DIRECTION ( 'NONE',  ( -0.000000000000000000, -0.000000000000000000, -1.000000000000000000 ) ) ;
#10538 = EDGE_CURVE ( 'NONE', #21725, #15101, #15778, .T. ) ;
#10539 = DIRECTION ( 'NONE',  ( 0.000000000000000000, 0.000000000000000000, 1.000000000000000000 ) ) ;
#10540 = AXIS2_PLACEMENT_3D ( 'NONE', #14199, #28411, #19194 ) ;
#10541 = FACE_OUTER_BOUND ( 'NONE', #17215, .T. ) ;
#10542 = FACE_OUTER_BOUND ( 'NONE', #30249, .T. ) ;
#10543 = ORIENTED_EDGE ( 'NONE', *, *, #24216, .F. ) ;
#10544 = LINE ( 'NONE', #24895, #29249 ) ;
#10545 = EDGE_CURVE ( 'NONE', #2627, #16462, #24426, .T. ) ;
#10546 = DIRECTION ( 'NONE',  ( -1.000000000000000000, 0.000000000000000000, 0.000000000000000000 ) ) ;
#10547 =( LENGTH_UNIT ( ) NAMED_UNIT ( * ) SI_UNIT ( .MILLI., .METRE. ) );
#10548 = DIRECTION ( 'NONE',  ( -1.000000000000000000, 0.000000000000000000, 0.000000000000000000 ) ) ;
#10549 = DIRECTION ( 'NONE',  ( 1.000000000000000000, 0.000000000000000000, 0.000000000000000000 ) ) ;
#10550 = CARTESIAN_POINT ( 'NONE',  ( 17.22181377297005866, 14.41708049311048789, 1.500000000000000000 ) ) ;
#10551 = CARTESIAN_POINT ( 'NONE',  ( 0.000000000000000000, 1.699320956058915452E-16, -1.500000000000001776 ) ) ;
#10552 = DIRECTION ( 'NONE',  ( 0.000000000000000000, 0.000000000000000000, 1.000000000000000000 ) ) ;
#10553 = VERTEX_POINT ( 'NONE', #30185 ) ;
#10554 = CIRCLE ( 'NONE', #19498, 9.482273699623480212 ) ;
#10555 = DIRECTION ( 'NONE',  ( 0.000000000000000000, 0.000000000000000000, 1.000000000000000000 ) ) ;
#10556 = DIRECTION ( 'NONE',  ( -0.000000000000000000, -0.000000000000000000, 1.000000000000000000 ) ) ;
#10557 = ORIENTED_EDGE ( 'NONE', *, *, #24420, .F. ) ;
#10558 = ORIENTED_EDGE ( 'NONE', *, *, #9371, .T. ) ;
#10559 = CARTESIAN_POINT ( 'NONE',  ( 0.000000000000000000, -2.435693370351110282E-15, 21.50000000000000355 ) ) ;
#10560 = CARTESIAN_POINT ( 'NONE',  ( -20.65888525914364493, -38.75220717792906555, -19.50000000000000355 ) ) ;
#10561 = EDGE_CURVE ( 'NONE', #479, #30031, #24226, .T. ) ;
#10562 = DIRECTION ( 'NONE',  ( 0.000000000000000000, -0.000000000000000000, -1.000000000000000000 ) ) ;
#10563 = ADVANCED_FACE ( 'NONE', ( #11619 ), #3835, .F. ) ;
#10564 =( LENGTH_UNIT ( ) NAMED_UNIT ( * ) SI_UNIT ( .MILLI., .METRE. ) );
#10565 = AXIS2_PLACEMENT_3D ( 'NONE', #22721, #9843, #13234 ) ;
#10566 = CARTESIAN_POINT ( 'NONE',  ( 0.000000000000000000, 0.000000000000000000, 63.50000000000000000 ) ) ;
#10567 = DIRECTION ( 'NONE',  ( 0.000000000000000000, 0.000000000000000000, -1.000000000000000000 ) ) ;
#10568 = EDGE_LOOP ( 'NONE', ( #22095, #13062 ) ) ;
#10569 = EDGE_LOOP ( 'NONE', ( #2477, #9337, #2400, #8915 ) ) ;
#10570 = CARTESIAN_POINT ( 'NONE',  ( 18.48179574117062529, -7.690589227441820164, 20.29915277494337644 ) ) ;
#10571 = DIRECTION ( 'NONE',  ( 0.000000000000000000, 0.000000000000000000, 1.000000000000000000 ) ) ;
#10572 = FACE_OUTER_BOUND ( 'NONE', #12270, .T. ) ;
#10573 = VERTEX_POINT ( 'NONE', #30482 ) ;
#10574 = APPLICATION_CONTEXT ( 'automotive_design' ) ;
#10575 = CARTESIAN_POINT ( 'NONE',  ( -4.697473163589096501, 16.36296782917919757, 19.85270094495842130 ) ) ;
#10576 = ORIENTED_EDGE ( 'NONE', *, *, #29297, .F. ) ;
#10577 = AXIS2_PLACEMENT_3D ( 'NONE', #12870, #10827, #15337 ) ;
#10578 = CYLINDRICAL_SURFACE ( 'NONE', #24274, 6.000000000000005329 ) ;
#10579 = ORIENTED_EDGE ( 'NONE', *, *, #24597, .F. ) ;
#10580 = CARTESIAN_POINT ( 'NONE',  ( 9.958038337755681368, 17.34466697471553331, 1.500000000000001332 ) ) ;
#10581 = CARTESIAN_POINT ( 'NONE',  ( 28.21921180493569281, -29.36589712660545359, 30.11501300312919938 ) ) ;
#10582 = CARTESIAN_POINT ( 'NONE',  ( 16.65022252850694429, 3.724077645907917677, 7.500147780736496017 ) ) ;
#10583 = CARTESIAN_POINT ( 'NONE',  ( -12.66227964008306550, -1.387778780781445676E-14, 1.500000000000000000 ) ) ;
#10584 = CARTESIAN_POINT ( 'NONE',  ( -8.550548368345316064, -14.74545326172986570, 20.34789198813115263 ) ) ;
#10585 = CARTESIAN_POINT ( 'NONE',  ( -38.72977682550716594, 5.035713241503631643, 32.14724780218217859 ) ) ;
#10586 = CARTESIAN_POINT ( 'NONE',  ( -9.072316094091473104, -14.41194981475155679, 7.453286057244485008 ) ) ;
#10587 = DIRECTION ( 'NONE',  ( 0.000000000000000000, 0.000000000000000000, 1.000000000000000000 ) ) ;
#10588 = ORIENTED_EDGE ( 'NONE', *, *, #27858, .T. ) ;
#10589 = EDGE_CURVE ( 'NONE', #1286, #7440, #15273, .T. ) ;
#10590 = DIRECTION ( 'NONE',  ( 0.6548607339452852116, -0.7557495743542581579, 0.000000000000000000 ) ) ;
#10591 = EDGE_CURVE ( 'NONE', #13891, #29673, #16263, .T. ) ;
#10592 = CARTESIAN_POINT ( 'NONE',  ( 11.87672590887049751, -16.11366389249060305, 18.92976555901915603 ) ) ;
#10593 = CARTESIAN_POINT ( 'NONE',  ( -8.728722367416567707, 2.516121109503271835, 13.22130136205108819 ) ) ;
#10594 = ORIENTED_EDGE ( 'NONE', *, *, #11710, .T. ) ;
#10595 = ORIENTED_EDGE ( 'NONE', *, *, #22971, .F. ) ;
#10596 = CARTESIAN_POINT ( 'NONE',  ( 18.08053511453368500, -8.550039048713406586, 20.14992337338002670 ) ) ;
#10597 = AXIS2_PLACEMENT_3D ( 'NONE', #14589, #1697, #11781 ) ;
#10598 = CIRCLE ( 'NONE', #18567, 1.447898107987198646 ) ;
#10599 = PLANE ( 'NONE',  #25582 ) ;
#10600 = VECTOR ( 'NONE', #1691, 1000.000000000000000 ) ;
#10601 = DIRECTION ( 'NONE',  ( -0.000000000000000000, -0.000000000000000000, 1.000000000000000000 ) ) ;
#10602 = ORIENTED_EDGE ( 'NONE', *, *, #16569, .T. ) ;
#10603 = CARTESIAN_POINT ( 'NONE',  ( 57.49999999999998579, 50.00000000000000000, 52.07879600563550326 ) ) ;
#10604 = CARTESIAN_POINT ( 'NONE',  ( -6.778663211761420726, 6.630478080506977179, 1.500000000000001332 ) ) ;
#10605 = DIRECTION ( 'NONE',  ( 1.982541115402065110E-16, 0.000000000000000000, -1.000000000000000000 ) ) ;
#10606 = ORIENTED_EDGE ( 'NONE', *, *, #17668, .F. ) ;
#10607 = CARTESIAN_POINT ( 'NONE',  ( 37.99999999999999289, 80.00000000000000000, 15.49999999999998934 ) ) ;
#10608 = CARTESIAN_POINT ( 'NONE',  ( -3.469446951953614189E-15, -30.50000000000000711, 1.500000000000000000 ) ) ;
#10609 = CARTESIAN_POINT ( 'NONE',  ( 19.89498243266959676, 2.215034284604906922, 6.420335371522007506 ) ) ;
#10610 = VERTEX_POINT ( 'NONE', #6324 ) ;
#10611 = CARTESIAN_POINT ( 'NONE',  ( 12.43151381881690831, 11.65737597917812529, 5.657991946698900598 ) ) ;
#10612 = ORIENTED_EDGE ( 'NONE', *, *, #5961, .T. ) ;
#10613 = CARTESIAN_POINT ( 'NONE',  ( -13.99459037270471029, 9.787106705871224221, 19.61324152429827450 ) ) ;
#10614 = CARTESIAN_POINT ( 'NONE',  ( -8.637616862297814890, 3.912171961292036482, 1.500000000000001332 ) ) ;
#10615 = ORIENTED_EDGE ( 'NONE', *, *, #1425, .F. ) ;
#10616 = VECTOR ( 'NONE', #15327, 1000.000000000000000 ) ;
#10617 = CARTESIAN_POINT ( 'NONE',  ( 4.376647981176111202, 19.53331152111370628, 6.995624166085161910 ) ) ;
#10618 = VECTOR ( 'NONE', #29397, 1000.000000000000000 ) ;
#10619 = LINE ( 'NONE', #8735, #10660 ) ;
#10620 = CARTESIAN_POINT ( 'NONE',  ( 5.888181818956395475, 19.11381997051147863, 18.54479204710284890 ) ) ;
#10621 = B_SPLINE_CURVE_WITH_KNOTS ( 'NONE', 3,
 ( #11383, #2010, #6684, #9182, #25713, #13869, #11534, #2306, #11991, #21484, #21801, #28831, #26333, #5271, #28676, #9646, #440, #2946 ),
 .UNSPECIFIED., .F., .F.,
 ( 4, 2, 2, 2, 2, 2, 2, 2, 4 ),
 ( 0.000000000000000000, 0.0003967869494442920046, 0.0007935738988885840091, 0.001190360848332876068, 0.001587147797777168018, 0.001983934747221460185, 0.002380721696665752136, 0.002777508646110044086, 0.003174295595554332567 ),
 .UNSPECIFIED. ) ;
#10622 = DIRECTION ( 'NONE',  ( 0.000000000000000000, 0.000000000000000000, -1.000000000000000000 ) ) ;
#10623 = CARTESIAN_POINT ( 'NONE',  ( 3.683253992019827727, -8.303920738747228469, 21.50000000000000000 ) ) ;
#10624 = CARTESIAN_POINT ( 'NONE',  ( 0.000000000000000000, 0.000000000000000000, -87.50000000000000000 ) ) ;
#10625 = ORIENTED_EDGE ( 'NONE', *, *, #5968, .T. ) ;
#10626 = CARTESIAN_POINT ( 'NONE',  ( 27.03074382657074537, 6.449748410230989215, 47.21042702067963148 ) ) ;
#10627 = CARTESIAN_POINT ( 'NONE',  ( -37.98493438988128901, 11.12428508575241004, -1.500000000000000000 ) ) ;
#10628 = DIRECTION ( 'NONE',  ( 0.000000000000000000, 0.000000000000000000, -1.000000000000000000 ) ) ;
#10629 = DIRECTION ( 'NONE',  ( 1.000000000000000000, 0.000000000000000000, 0.000000000000000000 ) ) ;
#10630 = VERTEX_POINT ( 'NONE', #25189 ) ;
#10631 = CARTESIAN_POINT ( 'NONE',  ( 28.74414854879570314, -28.72450863477462235, 10.34889633708970536 ) ) ;
#10632 = DIRECTION ( 'NONE',  ( -0.7071067811865541231, 8.659560562354850274E-17, -0.7071067811865408004 ) ) ;
#10633 = B_SPLINE_SURFACE_WITH_KNOTS ( 'NONE', 3, 1, ( 
 ( #21512, #14350 ),
 ( #9830, #23862 ),
 ( #14188, #12172 ),
 ( #23693, #23544 ),
 ( #2505, #12021 ),
 ( #16534, #28706 ),
 ( #21368, #21670 ),
 ( #7344, #306 ),
 ( #7, #19343 ),
 ( #28865, #7498 ),
 ( #16995, #24325 ) ),
 .UNSPECIFIED., .F., .F., .F.,
 ( 4, 1, 1, 1, 1, 1, 1, 1, 4 ),
 ( 2, 2 ),
 ( 0.000000000000000000, 0.3926990816987241395, 0.7853981633974482790, 1.178097245096172418, 1.570796326794896558, 1.963495408493620697, 2.356194490192344837, 2.748893571891068976, 3.141592653589793116 ),
 ( 0.000000000000000000, 1.000000000000000000 ),
 .UNSPECIFIED. ) ;
#10634 = CARTESIAN_POINT ( 'NONE',  ( -14.76283269969004230, 13.49301113316030865, 19.85261563089511228 ) ) ;
#10635 = DIRECTION ( 'NONE',  ( 1.000000000000000000, 0.000000000000000000, 0.000000000000000000 ) ) ;
#10636 = CIRCLE ( 'NONE', #1176, 0.6002263538043630664 ) ;
#10637 = FACE_OUTER_BOUND ( 'NONE', #1262, .T. ) ;
#10638 = LINE ( 'NONE', #20149, #30326 ) ;
#10639 = VECTOR ( 'NONE', #18271, 1000.000000000000000 ) ;
#10640 = CARTESIAN_POINT ( 'NONE',  ( 17.09492967699473809, 33.38213141764304481, 37.50000000000831335 ) ) ;
#10641 = ORIENTED_EDGE ( 'NONE', *, *, #1556, .F. ) ;
#10642 = CARTESIAN_POINT ( 'NONE',  ( 2.810445847081854964, 9.056208293496318618, 21.50000000000000000 ) ) ;
#10643 = VERTEX_POINT ( 'NONE', #9124 ) ;
#10644 = CARTESIAN_POINT ( 'NONE',  ( -24.03057240117690441, -26.57182937991348481, 24.50000000000000000 ) ) ;
#10645 = ORIENTED_EDGE ( 'NONE', *, *, #26618, .F. ) ;
#10646 = ORIENTED_EDGE ( 'NONE', *, *, #13979, .T. ) ;
#10647 = LINE ( 'NONE', #20157, #29869 ) ;
#10648 = CARTESIAN_POINT ( 'NONE',  ( -28.78283879316666471, -7.125616703334841873, 41.10667063058298965 ) ) ;
#10649 = ORIENTED_EDGE ( 'NONE', *, *, #8661, .T. ) ;
#10650 = LINE ( 'NONE', #22348, #4391 ) ;
#10651 = CARTESIAN_POINT ( 'NONE',  ( 14.97511466866788865, 47.70480676130072339, -55.99548085139268494 ) ) ;
#10652 = CARTESIAN_POINT ( 'NONE',  ( 3.395021109945021376, 30.50000000000000000, 1.500000000000000000 ) ) ;
#10653 = CARTESIAN_POINT ( 'NONE',  ( -12.24063095261064227, 4.490763173670005770, 24.50000000000000000 ) ) ;
#10654 = FACE_OUTER_BOUND ( 'NONE', #16004, .T. ) ;
#10655 = AXIS2_PLACEMENT_3D ( 'NONE', #19887, #8040, #17542 ) ;
#10656 = CARTESIAN_POINT ( 'NONE',  ( -10.51513057463695233, -17.01270198993486460, 7.652108011868850035 ) ) ;
#10657 = DIRECTION ( 'NONE',  ( -0.000000000000000000, -1.000000000000000000, -0.000000000000000000 ) ) ;
#10658 = FACE_OUTER_BOUND ( 'NONE', #21662, .T. ) ;
#10659 = ORIENTED_EDGE ( 'NONE', *, *, #18754, .F. ) ;
#10660 = VECTOR ( 'NONE', #1107, 1000.000000000000000 ) ;
#10661 = CARTESIAN_POINT ( 'NONE',  ( -9.396043825398766813, -14.19290753657279858, 19.45164628100866722 ) ) ;
#10662 = CARTESIAN_POINT ( 'NONE',  ( -18.02885658979140260, -8.699255478180120349, 7.652108011868850035 ) ) ;
#10663 = LINE ( 'NONE', #11136, #29005 ) ;
#10664 = EDGE_CURVE ( 'NONE', #29091, #19074, #4451, .T. ) ;
#10665 = CARTESIAN_POINT ( 'NONE',  ( 11.86528446860016928, -16.12209958341615135, 7.098451512883313441 ) ) ;
#10666 = ADVANCED_FACE ( 'NONE', ( #25515 ), #18644, .F. ) ;
#10667 = CARTESIAN_POINT ( 'NONE',  ( 25.19442432473618254, -35.44676296258426618, -19.50000000000000355 ) ) ;
#10668 = CARTESIAN_POINT ( 'NONE',  ( -15.57266529552203416, 38.96488032230103471, 1.500000000000000000 ) ) ;
#10669 = ORIENTED_EDGE ( 'NONE', *, *, #30510, .T. ) ;
#10670 = EDGE_LOOP ( 'NONE', ( #3099, #18412, #23029, #3978 ) ) ;
#10671 = CARTESIAN_POINT ( 'NONE',  ( -31.46108752401732289, 15.19043599309334702, 35.82118098715100984 ) ) ;
#10672 = CARTESIAN_POINT ( 'NONE',  ( 4.336808689942017736E-16, 42.50000000000000000, -1.500000000000000000 ) ) ;
#10673 = CARTESIAN_POINT ( 'NONE',  ( -12.91351154505913357, 11.09846585523631468, 5.940635272151477686 ) ) ;
#10674 = CARTESIAN_POINT ( 'NONE',  ( 0.4564504349074358647, -9.471281197126604212, 21.50000000000000000 ) ) ;
#10675 = VERTEX_POINT ( 'NONE', #22999 ) ;
#10676 = CARTESIAN_POINT ( 'NONE',  ( 29.61203839202723032, 15.40012917324034092, 37.38016955275583797 ) ) ;
#10677 = CARTESIAN_POINT ( 'NONE',  ( -40.89187623478217404, 5.790488632116478129, -19.50000000000000355 ) ) ;
#10678 = CARTESIAN_POINT ( 'NONE',  ( -9.378051617232568304, -14.20529941771991567, 6.420335371522007506 ) ) ;
#10679 = CIRCLE ( 'NONE', #14655, 6.999999999999999112 ) ;
#10680 = ORIENTED_EDGE ( 'NONE', *, *, #26931, .F. ) ;
#10681 = CARTESIAN_POINT ( 'NONE',  ( -18.04155359371238632, -8.631455508453164782, 5.652196082369963293 ) ) ;
#10682 = DIRECTION ( 'NONE',  ( -0.9898214418809326842, -0.1423148382732852824, 0.000000000000000000 ) ) ;
#10683 = CARTESIAN_POINT ( 'NONE',  ( 19.69872561633594188, 3.460482060625763800, 18.37545668562167478 ) ) ;
#10684 = ORIENTED_EDGE ( 'NONE', *, *, #25744, .T. ) ;
#10685 = CARTESIAN_POINT ( 'NONE',  ( 11.53007546964075836, -16.34234030559856166, 5.779535427900761135 ) ) ;
#10686 = CARTESIAN_POINT ( 'NONE',  ( -4.163336342344337027E-14, -1.387778780781445676E-14, 1.500000000000000000 ) ) ;
#10687 = EDGE_CURVE ( 'NONE', #15112, #5146, #21110, .T. ) ;
#10688 = FACE_BOUND ( 'NONE', #21604, .T. ) ;
#10689 = LINE ( 'NONE', #22535, #3880 ) ;
#10690 = ORIENTED_EDGE ( 'NONE', *, *, #25460, .T. ) ;
#10691 = CARTESIAN_POINT ( 'NONE',  ( -18.05883950494725099, -8.636531109380518600, 5.652196082367002106 ) ) ;
#10692 = DIRECTION ( 'NONE',  ( 0.8910248307962437275, 0.4539545692076742966, -0.000000000000000000 ) ) ;
#10693 = EDGE_CURVE ( 'NONE', #7304, #26027, #2315, .T. ) ;
#10694 = DIRECTION ( 'NONE',  ( -1.000000000000000000, 0.000000000000000000, 0.000000000000000000 ) ) ;
#10695 = EDGE_CURVE ( 'NONE', #15672, #2397, #30339, .T. ) ;
#10696 = CARTESIAN_POINT ( 'NONE',  ( -4.163336342344337027E-14, -1.387778780781445676E-14, 1.500000000000000000 ) ) ;
#10697 = CARTESIAN_POINT ( 'NONE',  ( -40.05520443301966083, -7.028746486913004077, -16.50000000000000000 ) ) ;
#10698 = DIRECTION ( 'NONE',  ( -1.000000000000000000, 0.000000000000000000, -0.000000000000000000 ) ) ;
#10699 = AXIS2_PLACEMENT_3D ( 'NONE', #10714, #29744, #28015 ) ;
#10700 = DIRECTION ( 'NONE',  ( -0.000000000000000000, -0.000000000000000000, 1.000000000000000000 ) ) ;
#10701 = FACE_OUTER_BOUND ( 'NONE', #22757, .T. ) ;
#10702 = ORIENTED_EDGE ( 'NONE', *, *, #30696, .F. ) ;
#10703 = EDGE_CURVE ( 'NONE', #479, #20644, #1505, .T. ) ;
#10704 = DIRECTION ( 'NONE',  ( 0.000000000000000000, 0.000000000000000000, -1.000000000000000000 ) ) ;
#10705 = CARTESIAN_POINT ( 'NONE',  ( 0.5584673446549203168, 9.967293815311105476, -0.7361406979141401630 ) ) ;
#10706 = ORIENTED_EDGE ( 'NONE', *, *, #3854, .F. ) ;
#10707 = EDGE_LOOP ( 'NONE', ( #17588, #22895, #25552, #13013 ) ) ;
#10708 = CYLINDRICAL_SURFACE ( 'NONE', #28383, 20.00000000000000355 ) ;
#10709 = ADVANCED_FACE ( 'NONE', ( #20514 ), #8677, .T. ) ;
#10710 = CARTESIAN_POINT ( 'NONE',  ( -0.9831090015668330073, 49.99275926214126997, -69.97591847141403321 ) ) ;
#10711 = VERTEX_POINT ( 'NONE', #26546 ) ;
#10712 = DIRECTION ( 'NONE',  ( -0.000000000000000000, -0.000000000000000000, -1.000000000000000000 ) ) ;
#10713 = ADVANCED_FACE ( 'NONE', ( #14378 ), #11323, .F. ) ;
#10714 = CARTESIAN_POINT ( 'NONE',  ( -24.03057240117691862, 26.57182937991349903, -1.500000000000000000 ) ) ;
#10715 = EDGE_CURVE ( 'NONE', #11332, #5262, #18282, .T. ) ;
#10716 = ORIENTED_EDGE ( 'NONE', *, *, #6228, .F. ) ;
#10717 = EDGE_LOOP ( 'NONE', ( #13248, #12341, #25264, #16057 ) ) ;
#10718 = CARTESIAN_POINT ( 'NONE',  ( -19.83108769839776642, 2.729924941536435057, 7.632642797338977658 ) ) ;
#10719 = CARTESIAN_POINT ( 'NONE',  ( 18.00031268893095771, -8.717656915646674776, 6.033082186765049926 ) ) ;
#10720 = DIRECTION ( 'NONE',  ( 0.000000000000000000, -1.132880637372608986E-16, 1.000000000000000000 ) ) ;
#10721 = FACE_OUTER_BOUND ( 'NONE', #28657, .T. ) ;
#10722 = VERTEX_POINT ( 'NONE', #28731 ) ;
#10723 = CARTESIAN_POINT ( 'NONE',  ( -5.062693764981720967, 16.26276758967388503, 18.47056384035244037 ) ) ;
#10724 = CIRCLE ( 'NONE', #14698, 9.084132297865673777 ) ;
#10725 = ORIENTED_EDGE ( 'NONE', *, *, #15262, .F. ) ;
#10726 = CARTESIAN_POINT ( 'NONE',  ( -16.96496224101209194, 1.652369717150043549, 20.34789198813115263 ) ) ;
#10727 = ORIENTED_EDGE ( 'NONE', *, *, #1172, .F. ) ;
#10728 = EDGE_CURVE ( 'NONE', #11596, #24236, #19271, .T. ) ;
#10729 = CARTESIAN_POINT ( 'NONE',  ( -6.565451881449789973, 18.89189346177362694, 18.54958172136247896 ) ) ;
#10730 = EDGE_CURVE ( 'NONE', #30328, #5571, #9319, .T. ) ;
#10731 = CARTESIAN_POINT ( 'NONE',  ( 5.141690706682880752, -7.488956955540417404, -1.500000000000002665 ) ) ;
#10732 = CARTESIAN_POINT ( 'NONE',  ( 19.61674503250824841, 3.986191100139169663, 6.041646659195333058 ) ) ;
#10733 = CARTESIAN_POINT ( 'NONE',  ( 6.962021646281533194, 6.437683520590192998, 1.500000000000001332 ) ) ;
#10734 = VECTOR ( 'NONE', #21929, 1000.000000000000000 ) ;
#10735 = ADVANCED_FACE ( 'NONE', ( #19056 ), #5020, .F. ) ;
#10736 = CARTESIAN_POINT ( 'NONE',  ( 29.99999999999925038, 1.387778780781445676E-14, 77.49999999999998579 ) ) ;
#10737 = CARTESIAN_POINT ( 'NONE',  ( 13.93942108199810193, -16.65122935894600076, -1.500000000000000000 ) ) ;
#10738 = CARTESIAN_POINT ( 'NONE',  ( -19.92178149465837578, 1.957245511797581106, 18.50655187082627862 ) ) ;
#10739 = CYLINDRICAL_SURFACE ( 'NONE', #27311, 20.00000000000000000 ) ;
#10740 = EDGE_LOOP ( 'NONE', ( #5037, #14105, #17124, #22879 ) ) ;
#10741 = CARTESIAN_POINT ( 'NONE',  ( 3.581105043790427711, 42.33170517314361092, 19.86130596537937976 ) ) ;
#10742 = EDGE_CURVE ( 'NONE', #12572, #7313, #8433, .T. ) ;
#10743 = CARTESIAN_POINT ( 'NONE',  ( 10.62299781869221604, -13.36838230995976495, 18.92976555901915603 ) ) ;
#10744 = CARTESIAN_POINT ( 'NONE',  ( 28.55068628633582151, 24.19494186940699620, 27.50000000000000355 ) ) ;
#10745 = ORIENTED_EDGE ( 'NONE', *, *, #30325, .F. ) ;
#10746 = ORIENTED_EDGE ( 'NONE', *, *, #2894, .F. ) ;
#10747 = AXIS2_PLACEMENT_3D ( 'NONE', #2269, #11790, #20982 ) ;
#10748 = DIRECTION ( 'NONE',  ( -1.000000000000000000, 0.000000000000000000, 0.000000000000000000 ) ) ;
#10749 = CARTESIAN_POINT ( 'NONE',  ( 4.510281037539698445E-13, -4.926614671774132148E-13, 82.49999999999998579 ) ) ;
#10750 = EDGE_CURVE ( 'NONE', #18996, #19059, #14787, .T. ) ;
#10751 = CARTESIAN_POINT ( 'NONE',  ( -5.205279254987321025, 19.32936484843851233, 7.272049892295485485 ) ) ;
#10752 = ORIENTED_EDGE ( 'NONE', *, *, #29770, .T. ) ;
#10753 = CARTESIAN_POINT ( 'NONE',  ( -12.86767874445213877, -1.850092897552710225, 1.500000000000001332 ) ) ;
#10754 = AXIS2_PLACEMENT_3D ( 'NONE', #24006, #12494, #2344 ) ;
#10755 = CARTESIAN_POINT ( 'NONE',  ( -12.73345385815986397, 11.29622791818862915, 6.910395520694543769 ) ) ;
#10756 = CARTESIAN_POINT ( 'NONE',  ( 23.94376008874366235, 13.17067969463889732, 47.67294373119254658 ) ) ;
#10757 = ORIENTED_EDGE ( 'NONE', *, *, #6548, .F. ) ;
#10758 = DIRECTION ( 'NONE',  ( 0.000000000000000000, -1.132880637372608986E-16, 1.000000000000000000 ) ) ;
#10759 = TOROIDAL_SURFACE ( 'NONE', #13265, 7.000000000000000000, 3.000000000000000000 ) ;
#10760 = CARTESIAN_POINT ( 'NONE',  ( 14.19710122452048928, 14.11195047426184246, 6.560937769032974209 ) ) ;
#10761 = CARTESIAN_POINT ( 'NONE',  ( 19.82606750293204456, 2.764250834391624334, 5.749228751562096562 ) ) ;
#10762 = VERTEX_POINT ( 'NONE', #4555 ) ;
#10763 = DIRECTION ( 'NONE',  ( 1.000000000000000000, 0.000000000000000000, 0.000000000000000000 ) ) ;
#10764 = VERTEX_POINT ( 'NONE', #2213 ) ;
#10765 = EDGE_CURVE ( 'NONE', #12881, #14629, #12306, .T. ) ;
#10766 = B_SPLINE_CURVE_WITH_KNOTS ( 'NONE', 3,
 ( #8657, #3975, #48, #16728, #2546, #7383, #26089, #12061, #11745, #4879, #13788, #18934, #4421, #2388, #30608, #11594, #16273, #21088 ),
 .UNSPECIFIED., .F., .F.,
 ( 4, 2, 2, 2, 2, 2, 2, 2, 4 ),
 ( 0.000000000000000000, 0.0003967869494442891856, 0.0007935738988885783713, 0.001190360848332867611, 0.001587147797777156743, 0.001983934747221445874, 0.002380721696665735222, 0.002777508646110024137, 0.003174295595554313485 ),
 .UNSPECIFIED. ) ;
#10767 = DIRECTION ( 'NONE',  ( -0.000000000000000000, -0.000000000000000000, -1.000000000000000000 ) ) ;
#10768 = EDGE_CURVE ( 'NONE', #25063, #28591, #9542, .T. ) ;
#10769 = CARTESIAN_POINT ( 'NONE',  ( 32.19782014694308003, -14.25394737442115201, 35.54550565580006349 ) ) ;
#10770 = ORIENTED_EDGE ( 'NONE', *, *, #29594, .F. ) ;
#10771 = VERTEX_POINT ( 'NONE', #4863 ) ;
#10772 = AXIS2_PLACEMENT_3D ( 'NONE', #17462, #21659, #26505 ) ;
#10773 = LINE ( 'NONE', #22768, #7610 ) ;
#10774 = CARTESIAN_POINT ( 'NONE',  ( 0.000000000000000000, 0.000000000000000000, 1.500000000000001332 ) ) ;
#10775 = AXIS2_PLACEMENT_3D ( 'NONE', #16052, #9334, #15738 ) ;
#10776 = CARTESIAN_POINT ( 'NONE',  ( -32.31576317091163730, -17.59561277345963148, 27.50000000000000355 ) ) ;
#10777 = CARTESIAN_POINT ( 'NONE',  ( 10.39222174957287415, -17.10906616942579817, 18.80699882434806369 ) ) ;
#10778 = CARTESIAN_POINT ( 'NONE',  ( 16.87408724266513360, 2.240810012149824892, 19.66989035740801839 ) ) ;
#10779 = ORIENTED_EDGE ( 'NONE', *, *, #25874, .F. ) ;
#10780 = CARTESIAN_POINT ( 'NONE',  ( -2.352830851074174223, -9.185733585337903406, 1.500000000000001332 ) ) ;
#10781 = CARTESIAN_POINT ( 'NONE',  ( 17.99235278053350839, -8.774603096602954011, 6.111214848085761986 ) ) ;
#10782 = CARTESIAN_POINT ( 'NONE',  ( -13.95039892200172638, 9.845341970609696958, 19.79423548914561692 ) ) ;
#10783 = VECTOR ( 'NONE', #9773, 1000.000000000000114 ) ;
#10784 = PLANE ( 'NONE',  #24752 ) ;
#10785 = VERTEX_POINT ( 'NONE', #17176 ) ;
#10786 = ORIENTED_EDGE ( 'NONE', *, *, #11617, .F. ) ;
#10787 = FACE_OUTER_BOUND ( 'NONE', #20565, .T. ) ;
#10788 = VECTOR ( 'NONE', #28897, 1000.000000000000000 ) ;
#10789 = CYLINDRICAL_SURFACE ( 'NONE', #16115, 0.7441270634456903510 ) ;
#10790 = CARTESIAN_POINT ( 'NONE',  ( -5.364573742045090299, 19.28565133533679088, 20.12545155307891065 ) ) ;
#10791 = DIRECTION ( 'NONE',  ( 0.000000000000000000, 1.000000000000000000, 1.193512090021232842E-16 ) ) ;
#10792 = CARTESIAN_POINT ( 'NONE',  ( 0.000000000000000000, 0.000000000000000000, 0.000000000000000000 ) ) ;
#10793 = DIRECTION ( 'NONE',  ( 1.000000000000000000, 0.000000000000000000, 0.000000000000000000 ) ) ;
#10794 = AXIS2_PLACEMENT_3D ( 'NONE', #883, #24119, #19921 ) ;
#10795 = CARTESIAN_POINT ( 'NONE',  ( -37.99999999999933920, 4.653657836759860688E-15, 82.49999999999998579 ) ) ;
#10796 = ORIENTED_EDGE ( 'NONE', *, *, #20599, .F. ) ;
#10797 = VECTOR ( 'NONE', #25357, 1000.000000000000000 ) ;
#10798 = AXIS2_PLACEMENT_3D ( 'NONE', #29395, #7876, #17685 ) ;
#10799 = CARTESIAN_POINT ( 'NONE',  ( 0.000000000000000000, 0.000000000000000000, 1.500000000000001332 ) ) ;
#10800 = EDGE_LOOP ( 'NONE', ( #15643, #4567, #129, #17983 ) ) ;
#10801 = LINE ( 'NONE', #22483, #9714 ) ;
#10802 = CYLINDRICAL_SURFACE ( 'NONE', #9475, 1.447898107987198646 ) ;
#10803 = EDGE_LOOP ( 'NONE', ( #21642, #20968 ) ) ;
#10804 = EDGE_LOOP ( 'NONE', ( #6988, #15048, #22031, #709 ) ) ;
#10805 = DIRECTION ( 'NONE',  ( -0.000000000000000000, -0.000000000000000000, -1.000000000000000000 ) ) ;
#10806 = EDGE_CURVE ( 'NONE', #3647, #15108, #13801, .T. ) ;
#10807 = CYLINDRICAL_SURFACE ( 'NONE', #15003, 9.000000000000000000 ) ;
#10808 = AXIS2_PLACEMENT_3D ( 'NONE', #30304, #8780, #22968 ) ;
#10809 = ORIENTED_EDGE ( 'NONE', *, *, #25773, .T. ) ;
#10810 = CARTESIAN_POINT ( 'NONE',  ( 13.24704986988986199, -36.75107818987552832, 27.50000000000000355 ) ) ;
#10811 = AXIS2_PLACEMENT_3D ( 'NONE', #20199, #27400, #1035 ) ;
#10812 = CARTESIAN_POINT ( 'NONE',  ( 14.49323551690688383, 47.85361797699681574, -51.10247338586245291 ) ) ;
#10813 = CYLINDRICAL_SURFACE ( 'NONE', #25942, 0.7500000000000006661 ) ;
#10814 = CARTESIAN_POINT ( 'NONE',  ( -36.99049879904470117, 13.48014611408327923, 9.989536694329901323 ) ) ;
#10815 = AXIS2_PLACEMENT_3D ( 'NONE', #14, #25757, #23246 ) ;
#10816 = DIRECTION ( 'NONE',  ( -1.000000000000000000, 0.000000000000000000, 0.000000000000000000 ) ) ;
#10817 = AXIS2_PLACEMENT_3D ( 'NONE', #22810, #13153, #20616 ) ;
#10818 = FACE_OUTER_BOUND ( 'NONE', #18560, .T. ) ;
#10819 = CARTESIAN_POINT ( 'NONE',  ( 4.510281037539698445E-13, -4.926614671774132148E-13, 57.49999999999999289 ) ) ;
#10820 =( LENGTH_UNIT ( ) NAMED_UNIT ( * ) SI_UNIT ( .MILLI., .METRE. ) );
#10821 = DIRECTION ( 'NONE',  ( -0.000000000000000000, -0.000000000000000000, -1.000000000000000000 ) ) ;
#10822 = ORIENTED_EDGE ( 'NONE', *, *, #1232, .F. ) ;
#10823 = AXIS2_PLACEMENT_3D ( 'NONE', #15140, #22322, #962 ) ;
#10824 = B_SPLINE_CURVE_WITH_KNOTS ( 'NONE', 3,
 ( #5943, #12968, #22459, #20132, #1575, #13277, #29814, #8901, #8596, #8456, #15923, #29649, #8285, #13587 ),
 .UNSPECIFIED., .F., .F.,
 ( 4, 2, 2, 2, 2, 2, 4 ),
 ( 0.0007411796533686801358, 0.001115232222424167698, 0.001489284791479655260, 0.001863337360535142605, 0.002237389929590630384, 0.002985495067701605075, 0.003733600205812580199 ),
 .UNSPECIFIED. ) ;
#10825 = CARTESIAN_POINT ( 'NONE',  ( -11.19021577446867255, -16.59822551944401781, 18.71435384576123440 ) ) ;
#10826 = CARTESIAN_POINT ( 'NONE',  ( -14.77756128048223694, -8.549967187541071212, 7.196036389296800451 ) ) ;
#10827 = DIRECTION ( 'NONE',  ( 0.000000000000000000, -1.000000000000000000, 0.000000000000000000 ) ) ;
#10828 = CARTESIAN_POINT ( 'NONE',  ( 11.90564931213029354, -16.09225693709294802, 6.341840715582230281 ) ) ;
#10829 = CARTESIAN_POINT ( 'NONE',  ( -2.687479362164884034, -44.39187623478217404, -19.50000000000000355 ) ) ;
#10830 = AXIS2_PLACEMENT_3D ( 'NONE', #9538, #11578, #21220 ) ;
#10831 = DIRECTION ( 'NONE',  ( 1.000000000000000000, 0.000000000000000000, 0.000000000000000000 ) ) ;
#10832 = CIRCLE ( 'NONE', #11348, 2.898871837527151385 ) ;
#10833 = ORIENTED_EDGE ( 'NONE', *, *, #617, .T. ) ;
#10834 = EDGE_LOOP ( 'NONE', ( #13289, #10746 ) ) ;
#10835 = CARTESIAN_POINT ( 'NONE',  ( -0.9370274472974918778, -8.840471615930066918, -3.621320343559650379 ) ) ;
#10836 = CARTESIAN_POINT ( 'NONE',  ( -37.98493438988125348, -11.12428508575252728, -1.500000000000000000 ) ) ;
#10837 = CARTESIAN_POINT ( 'NONE',  ( -15.07239450771860056, 13.17334274624126067, 5.749228751562096562 ) ) ;
#10838 = AXIS2_PLACEMENT_3D ( 'NONE', #7817, #26389, #14829 ) ;
#10839 = DIRECTION ( 'NONE',  ( 0.000000000000000000, 1.000000000000000000, -0.000000000000000000 ) ) ;
#10840 = ORIENTED_EDGE ( 'NONE', *, *, #13837, .F. ) ;
#10841 = CARTESIAN_POINT ( 'NONE',  ( 3.188743458493628502, 16.77324615163092858, 6.147510495896841398 ) ) ;
#10842 = VECTOR ( 'NONE', #2949, 1000.000000000000000 ) ;
#10843 = CARTESIAN_POINT ( 'NONE',  ( 32.74775157611827581, 27.21557300921217859, -19.50000000000000355 ) ) ;
#10844 = CARTESIAN_POINT ( 'NONE',  ( -9.400432693290859731, -14.18986588558385620, 6.641371103590088865 ) ) ;
#10845 = AXIS2_PLACEMENT_3D ( 'NONE', #17448, #20401, #12930 ) ;
#10846 = ORIENTED_EDGE ( 'NONE', *, *, #2346, .F. ) ;
#10847 = CARTESIAN_POINT ( 'NONE',  ( 24.44496207165490276, 7.595930209050162141, -16.55003854064094426 ) ) ;
#10848 = CARTESIAN_POINT ( 'NONE',  ( -6.513023399507313904, -41.93085199890154513, 28.88895809215988919 ) ) ;
#10849 = ORIENTED_EDGE ( 'NONE', *, *, #18588, .T. ) ;
#10850 = FACE_OUTER_BOUND ( 'NONE', #24887, .T. ) ;
#10851 = VECTOR ( 'NONE', #10682, 1000.000000000000114 ) ;
#10852 = VECTOR ( 'NONE', #20775, 1000.000000000000000 ) ;
#10853 = CARTESIAN_POINT ( 'NONE',  ( -40.00000000000000000, 87.00000000000001421, 52.49999999999999289 ) ) ;
#10854 = VERTEX_POINT ( 'NONE', #17336 ) ;
#10855 = CARTESIAN_POINT ( 'NONE',  ( 23.44138668973443629, 12.68271180600416237, 44.10533075972621475 ) ) ;
#10856 = CARTESIAN_POINT ( 'NONE',  ( 13.00948632770055546, 10.97642674697629062, 19.47784884541372818 ) ) ;
#10857 = CARTESIAN_POINT ( 'NONE',  ( 16.12090643789933253, -5.615848544355930727, 7.269896094239230777 ) ) ;
#10858 = DIRECTION ( 'NONE',  ( 1.000000000000000000, 0.000000000000000000, 0.000000000000000000 ) ) ;
#10859 = AXIS2_PLACEMENT_3D ( 'NONE', #2273, #11794, #30820 ) ;
#10860 = CARTESIAN_POINT ( 'NONE',  ( -16.96496224101209194, 1.652369717150044659, 7.652108011868850923 ) ) ;
#10861 = AXIS2_PLACEMENT_3D ( 'NONE', #28309, #23146, #11162 ) ;
#10862 = CARTESIAN_POINT ( 'NONE',  ( -4.163336342344337027E-14, 1.387778780781445676E-14, 62.49999999999999289 ) ) ;
#10863 = DIRECTION ( 'NONE',  ( 1.000000000000000000, 0.000000000000000000, 0.000000000000000000 ) ) ;
#10864 = LINE ( 'NONE', #5873, #6447 ) ;
#10865 = CARTESIAN_POINT ( 'NONE',  ( 25.64627119138473432, -23.40052582045089480, -6.500000000000000888 ) ) ;
#10866 = CARTESIAN_POINT ( 'NONE',  ( 34.70577939417261604, -10.49309206032036634, 34.49999999999999289 ) ) ;
#10867 = DIRECTION ( 'NONE',  ( -0.000000000000000000, -0.000000000000000000, -1.000000000000000000 ) ) ;
#10868 = ORIENTED_EDGE ( 'NONE', *, *, #11872, .F. ) ;
#10869 = ORIENTED_EDGE ( 'NONE', *, *, #29608, .F. ) ;
#10870 = CARTESIAN_POINT ( 'NONE',  ( 57.49999999999998579, 50.00000000000000000, 62.49999999999999289 ) ) ;
#10871 = CYLINDRICAL_SURFACE ( 'NONE', #6187, 20.00000000000000000 ) ;
#10872 = AXIS2_PLACEMENT_3D ( 'NONE', #24476, #12488, #21829 ) ;
#10873 = CARTESIAN_POINT ( 'NONE',  ( 0.5584673446549135445, 5.621163452808791483, 8.263859302085863945 ) ) ;
#10874 = VERTEX_POINT ( 'NONE', #12820 ) ;
#10875 = CIRCLE ( 'NONE', #21812, 22.49999999999996447 ) ;
#10876 = CARTESIAN_POINT ( 'NONE',  ( 23.11204206675566297, -35.56592873119179643, -11.49994521172425976 ) ) ;
#10877 = VECTOR ( 'NONE', #2055, 1000.000000000000000 ) ;
#10878 = CARTESIAN_POINT ( 'NONE',  ( 9.340794358644611606, -14.23940931090254125, 20.14907003336613300 ) ) ;
#10879 = ORIENTED_EDGE ( 'NONE', *, *, #6155, .F. ) ;
#10880 = ORIENTED_EDGE ( 'NONE', *, *, #28486, .T. ) ;
#10881 = CARTESIAN_POINT ( 'NONE',  ( -10.94312936609104270, -16.74105124841231529, 20.22277707861862339 ) ) ;
#10882 = CARTESIAN_POINT ( 'NONE',  ( -31.89119714134806927, -14.79609055705960863, 35.60128781023438194 ) ) ;
#10883 = AXIS2_PLACEMENT_3D ( 'NONE', #821, #29215, #27190 ) ;
#10884 = CARTESIAN_POINT ( 'NONE',  ( 15.40940123050674693, 12.74987339073084058, 7.267242832833945343 ) ) ;
#10885 = EDGE_CURVE ( 'NONE', #9573, #25790, #340, .T. ) ;
#10886 = CARTESIAN_POINT ( 'NONE',  ( -15.96900124075088456, 38.78095776257472949, 29.17368192679814243 ) ) ;
#10887 = ORIENTED_EDGE ( 'NONE', *, *, #27904, .F. ) ;
#10888 = CARTESIAN_POINT ( 'NONE',  ( -4.769904382750534744, 16.34378370244061429, 19.96344307082653202 ) ) ;
#10889 = ORIENTED_EDGE ( 'NONE', *, *, #20194, .F. ) ;
#10890 = EDGE_CURVE ( 'NONE', #20928, #3711, #16580, .T. ) ;
#10891 = FACE_OUTER_BOUND ( 'NONE', #18268, .T. ) ;
#10892 = CARTESIAN_POINT ( 'NONE',  ( 49.99999999999998579, -67.00000000000000000, 62.49999999999999289 ) ) ;
#10893 = VERTEX_POINT ( 'NONE', #15289 ) ;
#10894 = CARTESIAN_POINT ( 'NONE',  ( 37.99999999999999289, 70.00000000000000000, -28.49999999999999645 ) ) ;
#10895 = AXIS2_PLACEMENT_3D ( 'NONE', #16317, #13828, #25833 ) ;
#10896 = ADVANCED_FACE ( 'NONE', ( #494 ), #7992, .F. ) ;
#10897 = DIRECTION ( 'NONE',  ( -0.9594929736144974797, -0.2817325568414297265, 0.000000000000000000 ) ) ;
#10898 = B_SPLINE_SURFACE_WITH_KNOTS ( 'NONE', 3, 1, ( 
 ( #7151, #14305 ),
 ( #2472, #21481 ),
 ( #122, #20499 ),
 ( #29130, #12293 ),
 ( #13181, #22523 ),
 ( #17117, #27385 ),
 ( #5268, #15510 ),
 ( #25025, #26640 ),
 ( #8521, #27533 ),
 ( #30022, #2942 ),
 ( #3086, #13032 ),
 ( #5432, #1171 ),
 ( #579, #18170 ),
 ( #12461, #21798 ),
 ( #3667, #10844 ),
 ( #8353, #1323 ),
 ( #20184, #10678 ),
 ( #27678, #14935 ),
 ( #437, #24127 ),
 ( #9953, #6306 ),
 ( #19460, #18022 ),
 ( #24445, #19610 ),
 ( #17868, #7766 ),
 ( #28976, #7611 ),
 ( #15660, #22672 ),
 ( #14774, #17273 ),
 ( #2779, #20351 ),
 ( #29880, #24293 ),
 ( #26806, #13341 ),
 ( #25173, #6154 ),
 ( #3818, #22838 ) ),
 .UNSPECIFIED., .F., .F., .F.,
 ( 4, 3, 3, 3, 3, 3, 3, 3, 3, 3, 4 ),
 ( 2, 2 ),
 ( 0.000000000000000000, 0.05425176834609633791, 0.1085332949128352958, 0.1623767749169382768, 0.2157504826133063158, 0.2688657508888171455, 0.3218907763505476360, 0.3749548578363336993, 0.4282048033836242107, 0.4818374082110501444, 0.4999999999131654604 ),
 ( 0.000000000000000000, 1.000000000000000000 ),
 .UNSPECIFIED. ) ;
#10899 = CARTESIAN_POINT ( 'NONE',  ( 16.74250592927945647, 3.198927888044585721, 5.652196082364320695 ) ) ;
#10900 = LINE ( 'NONE', #22577, #12130 ) ;
#10901 = VECTOR ( 'NONE', #28763, 1000.000000000000000 ) ;
#10902 = EDGE_CURVE ( 'NONE', #17876, #897, #24820, .T. ) ;
#10903 = AXIS2_PLACEMENT_3D ( 'NONE', #2288, #13855, #9479 ) ;
#10904 = B_SPLINE_CURVE_WITH_KNOTS ( 'NONE', 3,
 ( #7007, #28530, #14325, #7164, #6554, #23217, #16066, #1870 ),
 .UNSPECIFIED., .F., .F.,
 ( 4, 2, 2, 4 ),
 ( 0.005257893453559869812, 0.006567392922673212161, 0.007876892391786554509, 0.01049589133001323921 ),
 .UNSPECIFIED. ) ;
#10905 = CARTESIAN_POINT ( 'NONE',  ( 1.795426799894640935, -16.98366215210794294, 6.588756557121054236 ) ) ;
#10906 = EDGE_CURVE ( 'NONE', #28482, #14635, #4330, .T. ) ;
#10907 = CARTESIAN_POINT ( 'NONE',  ( 32.82330813384650270, 22.94799032727486932, -1.500000000000000000 ) ) ;
#10908 = DIRECTION ( 'NONE',  ( -0.6707505147970090897, 0.7416830501633074890, 0.000000000000000000 ) ) ;
#10909 = FACE_BOUND ( 'NONE', #13354, .T. ) ;
#10910 = CARTESIAN_POINT ( 'NONE',  ( 11.93399590641349484, -16.07127689286907568, 19.14333282897057842 ) ) ;
#10911 = AXIS2_PLACEMENT_3D ( 'NONE', #30199, #9289, #13681 ) ;
#10912 = CARTESIAN_POINT ( 'NONE',  ( 28.55068628633582151, 24.19494186940699620, 34.80090346875809360 ) ) ;
#10913 = ORIENTED_EDGE ( 'NONE', *, *, #30347, .T. ) ;
#10914 = VERTEX_POINT ( 'NONE', #17808 ) ;
#10915 = DIRECTION ( 'NONE',  ( 0.000000000000000000, 0.000000000000000000, -1.000000000000000000 ) ) ;
#10916 = DIRECTION ( 'NONE',  ( -0.000000000000000000, -0.000000000000000000, 1.000000000000000000 ) ) ;
#10917 = B_SPLINE_CURVE_WITH_KNOTS ( 'NONE', 3,
 ( #15583, #18088, #6680, #13261 ),
 .UNSPECIFIED., .F., .F.,
 ( 4, 4 ),
 ( 3.022186913382060468E-07, 0.007932103869840195776 ),
 .UNSPECIFIED. ) ;
#10918 = CARTESIAN_POINT ( 'NONE',  ( -5.216068956281040059, 19.32652695433949930, 6.018569869498933578 ) ) ;
#10919 = ORIENTED_EDGE ( 'NONE', *, *, #2531, .T. ) ;
#10920 = PLANE ( 'NONE',  #27570 ) ;
#10921 = DIRECTION ( 'NONE',  ( 1.000000000000000000, 0.000000000000000000, 0.000000000000000000 ) ) ;
#10922 = EDGE_CURVE ( 'NONE', #3636, #7391, #27249, .T. ) ;
#10923 = CARTESIAN_POINT ( 'NONE',  ( -32.19782014694307293, -14.25394737442115733, 35.54550565580014876 ) ) ;
#10924 = ORIENTED_EDGE ( 'NONE', *, *, #12401, .T. ) ;
#10925 = EDGE_CURVE ( 'NONE', #1692, #17876, #20280, .T. ) ;
#10926 = EDGE_CURVE ( 'NONE', #30839, #12572, #14678, .T. ) ;
#10927 = LINE ( 'NONE', #17945, #29181 ) ;
#10928 = AXIS2_PLACEMENT_3D ( 'NONE', #2881, #12405, #26271 ) ;
#10929 = CARTESIAN_POINT ( 'NONE',  ( -27.75715622479468081, 2.303929616531696922E-16, 1.500000000000000000 ) ) ;
#10930 = ADVANCED_FACE ( 'NONE', ( #24182 ), #10014, .F. ) ;
#10931 = FACE_OUTER_BOUND ( 'NONE', #25708, .T. ) ;
#10932 = ORIENTED_EDGE ( 'NONE', *, *, #20024, .F. ) ;
#10933 = VERTEX_POINT ( 'NONE', #22008 ) ;
#10934 = CARTESIAN_POINT ( 'NONE',  ( -14.00715867683253357, 9.770345079983769665, 19.21769074125272780 ) ) ;
#10935 = EDGE_CURVE ( 'NONE', #12072, #21461, #4283, .T. ) ;
#10936 = EDGE_LOOP ( 'NONE', ( #89, #21873, #22262, #20907, #13417 ) ) ;
#10937 = AXIS2_PLACEMENT_3D ( 'NONE', #472, #2809, #4834 ) ;
#10938 = ORIENTED_EDGE ( 'NONE', *, *, #17585, .F. ) ;
#10939 = EDGE_CURVE ( 'NONE', #11554, #18416, #6923, .T. ) ;
#10940 = EDGE_CURVE ( 'NONE', #6144, #11315, #22622, .T. ) ;
#10941 = CARTESIAN_POINT ( 'NONE',  ( 4.330755352941445757, 19.54356050811955825, 6.447548852708279377 ) ) ;
#10942 = DIRECTION ( 'NONE',  ( -0.000000000000000000, -0.000000000000000000, -1.000000000000000000 ) ) ;
#10943 = CARTESIAN_POINT ( 'NONE',  ( 49.99999999999998579, 50.00000000000000000, 12.49999999999999112 ) ) ;
#10944 = VERTEX_POINT ( 'NONE', #5952 ) ;
#10945 = CIRCLE ( 'NONE', #27393, 12.66227964008308682 ) ;
#10946 = CARTESIAN_POINT ( 'NONE',  ( 15.41296542101254552, 5.939519782021115191, -0.6213203435596476032 ) ) ;
#10947 = CARTESIAN_POINT ( 'NONE',  ( 19.88727842228974652, 2.283828795636141162, 19.77662771831109367 ) ) ;
#10948 = ORIENTED_EDGE ( 'NONE', *, *, #14165, .F. ) ;
#10949 = CARTESIAN_POINT ( 'NONE',  ( -16.83923888061477570, 2.503175730361749896, 19.87181966307587544 ) ) ;
#10950 = CARTESIAN_POINT ( 'NONE',  ( 18.17321615974886129, -8.393345561651573306, 5.749228751562096562 ) ) ;
#10951 = DIRECTION ( 'NONE',  ( 0.000000000000000000, 0.000000000000000000, 1.000000000000000000 ) ) ;
#10952 = CARTESIAN_POINT ( 'NONE',  ( 5.089453839167152438, 19.35995229554825769, 20.32367522806703874 ) ) ;
#10953 = VERTEX_POINT ( 'NONE', #3765 ) ;
#10954 = ORIENTED_EDGE ( 'NONE', *, *, #22329, .T. ) ;
#10955 = FACE_OUTER_BOUND ( 'NONE', #19280, .T. ) ;
#10956 = EDGE_CURVE ( 'NONE', #21029, #27347, #3788, .T. ) ;
#10957 = CARTESIAN_POINT ( 'NONE',  ( -4.573183673931448645, 16.39543396787672691, 19.45164628100866722 ) ) ;
#10958 = FACE_OUTER_BOUND ( 'NONE', #9909, .T. ) ;
#10959 = VECTOR ( 'NONE', #1410, 1000.000000000000000 ) ;
#10960 = DIRECTION ( 'NONE',  ( 1.000000000000000000, 0.000000000000000000, 0.000000000000000000 ) ) ;
#10961 = EDGE_CURVE ( 'NONE', #4691, #28054, #11093, .T. ) ;
#10962 = CARTESIAN_POINT ( 'NONE',  ( 0.000000000000000000, 0.000000000000000000, 1.500000000000001332 ) ) ;
#10963 = ORIENTED_EDGE ( 'NONE', *, *, #28970, .T. ) ;
#10964 = EDGE_CURVE ( 'NONE', #13279, #20113, #25281, .T. ) ;
#10965 = AXIS2_PLACEMENT_3D ( 'NONE', #2736, #24398, #2582 ) ;
#10966 = CARTESIAN_POINT ( 'NONE',  ( -33.19297012087366028, -9.154531925606914200, 36.32560960716998011 ) ) ;
#10967 = DIRECTION ( 'NONE',  ( 0.000000000000000000, 0.000000000000000000, 1.000000000000000000 ) ) ;
#10968 = CARTESIAN_POINT ( 'NONE',  ( 32.24119409414369386, 26.76047229433004659, -16.50000600000000262 ) ) ;
#10969 = ORIENTED_EDGE ( 'NONE', *, *, #18537, .F. ) ;
#10970 = ORIENTED_EDGE ( 'NONE', *, *, #249, .T. ) ;
#10971 = CARTESIAN_POINT ( 'NONE',  ( -19.82706496683076836, 2.627678016133613959, 7.652108011868850923 ) ) ;
#10972 = CARTESIAN_POINT ( 'NONE',  ( 39.52380524533145945, -7.028748154382054913, -11.49999999999999645 ) ) ;
#10973 = VERTEX_POINT ( 'NONE', #3928 ) ;
#10974 = CARTESIAN_POINT ( 'NONE',  ( -11.86767874445213167, -1.850092897552710225, 24.50000000000000000 ) ) ;
#10975 = CARTESIAN_POINT ( 'NONE',  ( 11.29805255599380587, 48.71189377371128160, -45.08539549253174528 ) ) ;
#10976 = DIRECTION ( 'NONE',  ( -0.000000000000000000, 0.000000000000000000, -1.000000000000000000 ) ) ;
#10977 = CARTESIAN_POINT ( 'NONE',  ( 16.47768670952434178, 14.41708049311048789, -1.500000000000000000 ) ) ;
#10978 = AXIS2_PLACEMENT_3D ( 'NONE', #24163, #19187, #16698 ) ;
#10979 = CARTESIAN_POINT ( 'NONE',  ( 25.64627119138473432, 23.40052582045089480, -6.500000000000000888 ) ) ;
#10980 = CARTESIAN_POINT ( 'NONE',  ( 24.03057240117691862, -26.57182937991349903, 1.500000000000000000 ) ) ;
#10981 = CARTESIAN_POINT ( 'NONE',  ( 1.303806812501129064, -19.97511938206332971, 6.995624166085161910 ) ) ;
#10982 = CARTESIAN_POINT ( 'NONE',  ( -16.82262805706082531, 2.599658093664293457, 6.973843882838226094 ) ) ;
#10983 = ORIENTED_EDGE ( 'NONE', *, *, #11235, .T. ) ;
#10984 = DIRECTION ( 'NONE',  ( 0.000000000000000000, 0.000000000000000000, 1.000000000000000000 ) ) ;
#10985 = CARTESIAN_POINT ( 'NONE',  ( -27.03074382657074537, -6.449748410230988327, -16.55003854064094426 ) ) ;
#10986 = DIRECTION ( 'NONE',  ( 0.000000000000000000, 0.000000000000000000, 1.000000000000000000 ) ) ;
#10987 = CARTESIAN_POINT ( 'NONE',  ( 1.438332125858173605, -8.884323311075778662, 21.50000000000000000 ) ) ;
#10988 = EDGE_CURVE ( 'NONE', #16799, #10191, #28176, .T. ) ;
#10989 = CARTESIAN_POINT ( 'NONE',  ( 10.64374042650304020, -42.96126232887725394, -19.50000000000000355 ) ) ;
#10990 = DIRECTION ( 'NONE',  ( -0.000000000000000000, -0.000000000000000000, 1.000000000000000000 ) ) ;
#10991 = ORIENTED_EDGE ( 'NONE', *, *, #7295, .T. ) ;
#10992 =( REPRESENTATION_RELATIONSHIP ('NONE','NONE', #19885, #13696 ) REPRESENTATION_RELATIONSHIP_WITH_TRANSFORMATION ( #4080 )SHAPE_REPRESENTATION_RELATIONSHIP( ) );
#10993 = FACE_OUTER_BOUND ( 'NONE', #22284, .T. ) ;
#10994 = CARTESIAN_POINT ( 'NONE',  ( 31.18700685317242716, 26.11823559933198879, -1.500000000000000000 ) ) ;
#10995 = CARTESIAN_POINT ( 'NONE',  ( 36.61818605946716332, -14.68367171281316175, 31.56304765520175692 ) ) ;
#10996 = DIRECTION ( 'NONE',  ( -0.000000000000000000, 1.000000000000000000, -0.000000000000000000 ) ) ;
#10997 = ORIENTED_EDGE ( 'NONE', *, *, #18399, .T. ) ;
#10998 = CIRCLE ( 'NONE', #26940, 0.7499999999999988898 ) ;
#10999 = CARTESIAN_POINT ( 'NONE',  ( -10.64374042650306862, 42.96126232887723972, -19.50000000000000355 ) ) ;
#11000 = CARTESIAN_POINT ( 'NONE',  ( 7.562559277181973627, -5.881244434206257310, 21.50000000000000000 ) ) ;
#11001 = VERTEX_POINT ( 'NONE', #18263 ) ;
#11002 = DIRECTION ( 'NONE',  ( -0.000000000000000000, -0.000000000000000000, 1.000000000000000000 ) ) ;
#11003 = CARTESIAN_POINT ( 'NONE',  ( 19.55539447853113799, 4.193631725790831766, 19.48477075383299351 ) ) ;
#11004 = VERTEX_POINT ( 'NONE', #15605 ) ;
#11005 = CARTESIAN_POINT ( 'NONE',  ( -32.08353430114796367, 26.68014822536797226, -14.83332872408068148 ) ) ;
#11006 = DIRECTION ( 'NONE',  ( 0.000000000000000000, 0.000000000000000000, 1.000000000000000000 ) ) ;
#11007 = CARTESIAN_POINT ( 'NONE',  ( 31.46108752401734066, -15.19043599309334169, 40.06382167427020136 ) ) ;
#11008 = DIRECTION ( 'NONE',  ( 0.4495526574063634095, 0.8932538319083086487, 0.000000000000000000 ) ) ;
#11009 = ORIENTED_EDGE ( 'NONE', *, *, #18721, .F. ) ;
#11010 = CARTESIAN_POINT ( 'NONE',  ( 11.67912593704039637, 12.45929511323409855, 19.61324152429827095 ) ) ;
#11011 = DIRECTION ( 'NONE',  ( 0.000000000000000000, -1.000000000000000000, 0.000000000000000000 ) ) ;
#11012 = CARTESIAN_POINT ( 'NONE',  ( 0.9770435002939156233, -19.97634058022565995, 18.54958172136248251 ) ) ;
#11013 = AXIS2_PLACEMENT_3D ( 'NONE', #11269, #20764, #16550 ) ;
#11014 = CARTESIAN_POINT ( 'NONE',  ( -12.66227964008306550, -1.387778780781445676E-14, 1.500000000000000000 ) ) ;
#11015 = CARTESIAN_POINT ( 'NONE',  ( -6.974883619896829146, -5.687793815610328707, 1.500000000000001332 ) ) ;
#11016 = DIRECTION ( 'NONE',  ( -0.000000000000000000, -0.000000000000000000, -1.000000000000000000 ) ) ;
#11017 = LINE ( 'NONE', #15372, #27975 ) ;
#11018 = DIRECTION ( 'NONE',  ( -1.000000000000000000, 0.000000000000000000, 0.000000000000000000 ) ) ;
#11019 = CARTESIAN_POINT ( 'NONE',  ( 9.035144332694070357, -14.42607982873159678, 6.910395520694542881 ) ) ;
#11020 = CARTESIAN_POINT ( 'NONE',  ( 0.000000000000000000, 0.000000000000000000, 1.500000000000001332 ) ) ;
#11021 = PLANE ( 'NONE',  #26023 ) ;
#11022 = ORIENTED_EDGE ( 'NONE', *, *, #22530, .T. ) ;
#11023 = VERTEX_POINT ( 'NONE', #10780 ) ;
#11024 = DIRECTION ( 'NONE',  ( -0.000000000000000000, -0.000000000000000000, 1.000000000000000000 ) ) ;
#11025 = EDGE_CURVE ( 'NONE', #6674, #14001, #8605, .T. ) ;
#11026 = CARTESIAN_POINT ( 'NONE',  ( -52.99999999999955236, -4.926614671774132148E-13, 62.49999999999998579 ) ) ;
#11027 = CARTESIAN_POINT ( 'NONE',  ( 18.33599632111990374, -7.986941774664180649, 20.34789198813115263 ) ) ;
#11028 = ORIENTED_EDGE ( 'NONE', *, *, #12472, .F. ) ;
#11029 = CARTESIAN_POINT ( 'NONE',  ( 23.00100564131886927, -35.20929533517521293, -8.166629612182571663 ) ) ;
#11030 = CARTESIAN_POINT ( 'NONE',  ( -7.730328572437709767, 4.608906612435681005, 21.50000000000000000 ) ) ;
#11031 = VERTEX_POINT ( 'NONE', #1434 ) ;
#11032 = ORIENTED_EDGE ( 'NONE', *, *, #11034, .F. ) ;
#11033 = CARTESIAN_POINT ( 'NONE',  ( -19.72724879956886923, 3.398799651952292056, 6.211014596808754007 ) ) ;
#11034 = EDGE_CURVE ( 'NONE', #2118, #13370, #5787, .T. ) ;
#11035 = CARTESIAN_POINT ( 'NONE',  ( -32.19782014694307293, -14.25394737442115733, 35.54550565580014876 ) ) ;
#11036 = AXIS2_PLACEMENT_3D ( 'NONE', #11770, #9278, #1804 ) ;
#11037 = DIRECTION ( 'NONE',  ( 0.000000000000000000, 1.000000000000000000, -0.000000000000000000 ) ) ;
#11038 = DIRECTION ( 'NONE',  ( 0.000000000000000000, 1.000000000000000000, 0.000000000000000000 ) ) ;
#11039 = ORIENTED_EDGE ( 'NONE', *, *, #13448, .T. ) ;
#11040 = DIRECTION ( 'NONE',  ( 0.000000000000000000, -0.000000000000000000, 1.000000000000000000 ) ) ;
#11041 = ORIENTED_EDGE ( 'NONE', *, *, #19663, .F. ) ;
#11042 = CARTESIAN_POINT ( 'NONE',  ( -14.76516729829709007, -8.573104839208673056, 7.158811349119584833 ) ) ;
#11043 = DIRECTION ( 'NONE',  ( 1.000000000000000000, 0.000000000000000000, 0.000000000000000000 ) ) ;
#11044 = ORIENTED_EDGE ( 'NONE', *, *, #10312, .F. ) ;
#11045 = CARTESIAN_POINT ( 'NONE',  ( -6.933969404122160007, 18.75953273845654579, 19.48477075383299706 ) ) ;
#11046 = VECTOR ( 'NONE', #808, 1000.000000000000000 ) ;
#11047 = CARTESIAN_POINT ( 'NONE',  ( 29.04733024409324571, -28.39068243925979473, 30.21700144173808411 ) ) ;
#11048 = CARTESIAN_POINT ( 'NONE',  ( 0.3493064693810319365, -20.01473674030432548, 7.652108011868850035 ) ) ;
#11049 = CARTESIAN_POINT ( 'NONE',  ( -9.650234827617421018, -17.53789701089550590, 19.47783254395485031 ) ) ;
#11050 = CARTESIAN_POINT ( 'NONE',  ( -17.02500080808232852, 1.126395502206346100, 18.45571264222803975 ) ) ;
#11051 = CARTESIAN_POINT ( 'NONE',  ( -19.95113275051131652, 1.631914050426796381, 18.82680253904184298 ) ) ;
#11052 = DIRECTION ( 'NONE',  ( 1.000000000000000000, 0.000000000000000000, 0.000000000000000000 ) ) ;
#11053 = ORIENTED_EDGE ( 'NONE', *, *, #590, .T. ) ;
#11054 = CARTESIAN_POINT ( 'NONE',  ( -14.36006998371493637, -17.26937953831884442, -1.500000000000000000 ) ) ;
#11055 = VECTOR ( 'NONE', #28953, 1000.000000000000000 ) ;
#11056 = CARTESIAN_POINT ( 'NONE',  ( 17.94248964168179583, 34.33858135081683827, 27.50000000000000355 ) ) ;
#11057 = ORIENTED_EDGE ( 'NONE', *, *, #1264, .T. ) ;
#11058 = ORIENTED_EDGE ( 'NONE', *, *, #30067, .T. ) ;
#11059 = CARTESIAN_POINT ( 'NONE',  ( 42.39173574096481900, 68.49922546432578940, 12.78508226459883801 ) ) ;
#11060 = ADVANCED_FACE ( 'NONE', ( #20731 ), #27784, .F. ) ;
#11061 = CARTESIAN_POINT ( 'NONE',  ( -4.163336342344337027E-14, 1.387778780781445676E-14, 24.50000000000000000 ) ) ;
#11062 = ADVANCED_FACE ( 'NONE', ( #15759 ), #912, .T. ) ;
#11063 = CARTESIAN_POINT ( 'NONE',  ( -4.581181804672376678, 16.39335237280002033, 6.530762810602277924 ) ) ;
#11064 = VERTEX_POINT ( 'NONE', #26354 ) ;
#11065 = DIRECTION ( 'NONE',  ( -5.125319360840571077E-16, 1.000000000000000000, 0.000000000000000000 ) ) ;
#11066 = CARTESIAN_POINT ( 'NONE',  ( -13.38160118231794549, 10.55829203257430038, 5.652196082368482699 ) ) ;
#11067 = DIRECTION ( 'NONE',  ( 0.000000000000000000, 1.132880637372608986E-16, -1.000000000000000000 ) ) ;
#11068 = VERTEX_POINT ( 'NONE', #4981 ) ;
#11069 = VECTOR ( 'NONE', #23273, 1000.000000000000000 ) ;
#11070 = CARTESIAN_POINT ( 'NONE',  ( 31.56327786402390245, -10.34181101807379655, -16.55003854064094426 ) ) ;
#11071 = CARTESIAN_POINT ( 'NONE',  ( -8.478038329015333829, 15.04174200911163517, 24.50000000000000000 ) ) ;
#11072 = ORIENTED_EDGE ( 'NONE', *, *, #11683, .F. ) ;
#11073 = EDGE_CURVE ( 'NONE', #7851, #25580, #14029, .T. ) ;
#11074 = CARTESIAN_POINT ( 'NONE',  ( 12.40635649856746525, 11.68570839673119544, 5.653912893140659257 ) ) ;
#11075 = ORIENTED_EDGE ( 'NONE', *, *, #14735, .F. ) ;
#11076 = CARTESIAN_POINT ( 'NONE',  ( -13.93282946020425328, 9.868441342995359022, 18.84329447212443753 ) ) ;
#11077 = CIRCLE ( 'NONE', #16536, 12.50000000000000000 ) ;
#11078 = ORIENTED_EDGE ( 'NONE', *, *, #3805, .T. ) ;
#11079 = ORIENTED_EDGE ( 'NONE', *, *, #18723, .F. ) ;
#11080 = CARTESIAN_POINT ( 'NONE',  ( 3.283642163210882092, 16.75135354181592007, 7.280727868105637768 ) ) ;
#11081 = FACE_OUTER_BOUND ( 'NONE', #14279, .T. ) ;
#11082 = CARTESIAN_POINT ( 'NONE',  ( 5.780652116621848968, 19.14677724775279088, 18.47110296274025387 ) ) ;
#11083 = EDGE_LOOP ( 'NONE', ( #14442, #5664, #23489, #25449 ) ) ;
#11084 = EDGE_CURVE ( 'NONE', #11358, #12072, #23846, .T. ) ;
#11085 = AXIS2_PLACEMENT_3D ( 'NONE', #17941, #27450, #23618 ) ;
#11086 = CARTESIAN_POINT ( 'NONE',  ( -21.86019681245147694, -31.48592878035298170, 34.80090346875804386 ) ) ;
#11087 = FACE_OUTER_BOUND ( 'NONE', #5116, .T. ) ;
#11088 = CARTESIAN_POINT ( 'NONE',  ( 16.84609478243854852, 2.477959627222519057, 20.05479082170252525 ) ) ;
#11089 = ADVANCED_FACE ( 'NONE', ( #9661 ), #18876, .F. ) ;
#11090 = EDGE_LOOP ( 'NONE', ( #15043, #15963, #30291, #11429 ) ) ;
#11091 = ADVANCED_FACE ( 'NONE', ( #21182 ), #15882, .T. ) ;
#11092 = AXIS2_PLACEMENT_3D ( 'NONE', #11948, #23465, #16461 ) ;
#11093 = LINE ( 'NONE', #13449, #296 ) ;
#11094 = CARTESIAN_POINT ( 'NONE',  ( 15.43168774359948969, -7.187270164670358952, 6.211014596808754007 ) ) ;
#11095 = CARTESIAN_POINT ( 'NONE',  ( -15.35487439336962723, 12.84287527963943809, 20.34789198813115263 ) ) ;
#11096 = CARTESIAN_POINT ( 'NONE',  ( 4.678038002344203861, 19.46363151887951659, 18.56793045041961321 ) ) ;
#11097 = ORIENTED_EDGE ( 'NONE', *, *, #8203, .T. ) ;
#11098 = ORIENTED_EDGE ( 'NONE', *, *, #366, .F. ) ;
#11099 = CYLINDRICAL_SURFACE ( 'NONE', #21255, 2.061368542273053883 ) ;
#11100 = EDGE_CURVE ( 'NONE', #27407, #6185, #6273, .T. ) ;
#11101 = DIRECTION ( 'NONE',  ( -0.000000000000000000, -0.000000000000000000, -1.000000000000000000 ) ) ;
#11102 = ADVANCED_FACE ( 'NONE', ( #28853 ), #11153, .T. ) ;
#11103 = CARTESIAN_POINT ( 'NONE',  ( -5.435829780283180312, 16.15227280059887605, 20.34789198813115263 ) ) ;
#11104 = SURFACE_SIDE_STYLE ('',( #16084 ) ) ;
#11105 = CARTESIAN_POINT ( 'NONE',  ( 26.83043119477639138, -8.695877139419035728, -1.500000000000000000 ) ) ;
#11106 = EDGE_CURVE ( 'NONE', #25827, #25672, #28859, .T. ) ;
#11107 = DIRECTION ( 'NONE',  ( 1.000000000000000000, 0.000000000000000000, 0.000000000000000000 ) ) ;
#11108 = DIRECTION ( 'NONE',  ( 1.000000000000000000, 0.000000000000000000, 0.000000000000000000 ) ) ;
#11109 = EDGE_CURVE ( 'NONE', #22249, #24431, #21515, .T. ) ;
#11110 = ORIENTED_EDGE ( 'NONE', *, *, #7113, .F. ) ;
#11111 = CARTESIAN_POINT ( 'NONE',  ( -16.97424920726489717, 1.578583718960129945, 7.652108011868850035 ) ) ;
#11112 = ADVANCED_FACE ( 'NONE', ( #29163 ), #26521, .F. ) ;
#11113 = DIRECTION ( 'NONE',  ( 1.000000000000000000, 0.000000000000000000, 0.000000000000000000 ) ) ;
#11114 = CARTESIAN_POINT ( 'NONE',  ( 48.64405085385531180, 18.29172496293574213, 24.50000000000000355 ) ) ;
#11115 = ORIENTED_EDGE ( 'NONE', *, *, #30760, .T. ) ;
#11116 = EDGE_CURVE ( 'NONE', #20027, #1048, #1343, .T. ) ;
#11117 = VERTEX_POINT ( 'NONE', #7502 ) ;
#11118 = CARTESIAN_POINT ( 'NONE',  ( -19.84404562991029763, 2.492760124447686465, 5.652196082369965069 ) ) ;
#11119 = CIRCLE ( 'NONE', #7125, 9.482273699623480212 ) ;
#11120 = CARTESIAN_POINT ( 'NONE',  ( -19.87571927687822892, 2.229464111918812552, 18.37545668562167478 ) ) ;
#11121 = ORIENTED_EDGE ( 'NONE', *, *, #13206, .T. ) ;
#11122 = LINE ( 'NONE', #29994, #16286 ) ;
#11123 = CARTESIAN_POINT ( 'NONE',  ( -31.29501345865439532, 26.27841684421964885, -6.500000000000000888 ) ) ;
#11124 = CARTESIAN_POINT ( 'NONE',  ( 5.349779314757592275, 7.341751895053254096, 21.50000000000000000 ) ) ;
#11125 = CARTESIAN_POINT ( 'NONE',  ( 16.09518941752841670, 6.251081041772567737, 24.50000000000000000 ) ) ;
#11126 = CARTESIAN_POINT ( 'NONE',  ( -25.32744450373244760, 23.23809170341762709, -16.50001200000000168 ) ) ;
#11127 = CARTESIAN_POINT ( 'NONE',  ( 10.47960520055065992, -7.757439966934453146, 1.500000000000001332 ) ) ;
#11128 = DIRECTION ( 'NONE',  ( -0.000000000000000000, -1.000000000000000000, -0.000000000000000000 ) ) ;
#11129 = CARTESIAN_POINT ( 'NONE',  ( -32.19782014694307293, 14.25394737442115733, 39.78814634291943975 ) ) ;
#11130 = EDGE_CURVE ( 'NONE', #23754, #13645, #19185, .T. ) ;
#11131 = ORIENTED_EDGE ( 'NONE', *, *, #24666, .F. ) ;
#11132 = ADVANCED_FACE ( 'NONE', ( #474 ), #7770, .T. ) ;
#11133 = LINE ( 'NONE', #23117, #18821 ) ;
#11134 = CARTESIAN_POINT ( 'NONE',  ( 52.16608720827707657, -36.86186943028246787, 12.49999999999999112 ) ) ;
#11135 = EDGE_CURVE ( 'NONE', #15425, #11338, #24177, .T. ) ;
#11136 = CARTESIAN_POINT ( 'NONE',  ( -33.16313691975489064, -0.000000000000000000, -1.500000000000000000 ) ) ;
#11137 = CARTESIAN_POINT ( 'NONE',  ( -17.91073422896668177, -8.940227287121107480, 18.39992786714538298 ) ) ;
#11138 = EDGE_CURVE ( 'NONE', #24968, #19771, #27698, .T. ) ;
#11139 = CIRCLE ( 'NONE', #5656, 0.7500000000000006661 ) ;
#11140 = CARTESIAN_POINT ( 'NONE',  ( -12.56641067637752229, 40.32935944495016400, -1.500000000000000000 ) ) ;
#11141 = CARTESIAN_POINT ( 'NONE',  ( -23.05654803568342359, 35.38768970123298629, -9.833278305020469290 ) ) ;
#11142 = ORIENTED_EDGE ( 'NONE', *, *, #2132, .F. ) ;
#11143 = FACE_OUTER_BOUND ( 'NONE', #5922, .T. ) ;
#11144 = CARTESIAN_POINT ( 'NONE',  ( 37.98493438989863336, -11.12428508576153341, -1.500000000000000000 ) ) ;
#11145 = CARTESIAN_POINT ( 'NONE',  ( 33.55102796320213798, -21.82697637830245085, 30.90080749576968699 ) ) ;
#11146 = EDGE_CURVE ( 'NONE', #13891, #203, #14225, .T. ) ;
#11147 = LINE ( 'NONE', #23132, #19120 ) ;
#11148 = ORIENTED_EDGE ( 'NONE', *, *, #25245, .T. ) ;
#11149 = CARTESIAN_POINT ( 'NONE',  ( 15.91781874855163004, -6.122627424427364851, 20.34789198813115263 ) ) ;
#11150 = CARTESIAN_POINT ( 'NONE',  ( -39.83602371821029919, -11.57901747687044924, -19.50000000000000355 ) ) ;
#11151 = DIRECTION ( 'NONE',  ( -0.000000000000000000, -0.000000000000000000, 1.000000000000000000 ) ) ;
#11152 = VERTEX_POINT ( 'NONE', #28870 ) ;
#11153 = B_SPLINE_SURFACE_WITH_KNOTS ( 'NONE', 3, 1, ( 
 ( #17612, #9980 ),
 ( #17138, #24314 ),
 ( #2964, #10119 ),
 ( #10270, #19626 ),
 ( #3112, #12632 ),
 ( #22121, #19783 ),
 ( #7955, #25612 ),
 ( #26055, #16232 ),
 ( #4534, #21198 ),
 ( #13748, #30579 ),
 ( #14190, #30728 ),
 ( #9374, #16389 ),
 ( #18894, #25904 ),
 ( #27951, #11252 ),
 ( #23546, #8929 ),
 ( #6580, #11564 ),
 ( #16091, #4226 ),
 ( #2039, #30432 ),
 ( #23242, #1893 ),
 ( #7028, #6875 ),
 ( #11419, #14042 ),
 ( #28404, #2193 ),
 ( #6721, #20751 ),
 ( #9217, #25461 ),
 ( #8757, #30281 ),
 ( #4382, #16537 ),
 ( #11711, #18448 ),
 ( #4688, #25753 ),
 ( #20607, #28245 ),
 ( #1603, #11111 ),
 ( #23404, #30127 ) ),
 .UNSPECIFIED., .F., .F., .F.,
 ( 4, 3, 3, 3, 3, 3, 3, 3, 3, 3, 4 ),
 ( 2, 2 ),
 ( 0.4999999998345684427, 0.5360336730431942698, 0.5907651151589017324, 0.6456034593241839481, 0.6998270958050443191, 0.7529536536315944995, 0.8052385063053264513, 0.8575343587103996246, 0.9106564858195047574, 0.9648414833209688624, 1.000000006602610014 ),
 ( 0.000000000000000000, 1.000000000000000000 ),
 .UNSPECIFIED. ) ;
#11154 = AXIS2_PLACEMENT_3D ( 'NONE', #5368, #15171, #24537 ) ;
#11155 = CARTESIAN_POINT ( 'NONE',  ( 2.555255504830960867, -9.131494062835622927, 21.50000000000000000 ) ) ;
#11156 = CARTESIAN_POINT ( 'NONE',  ( 19.69983030747900088, 3.454193845114029049, 20.32200205377523972 ) ) ;
#11157 = ORIENTED_EDGE ( 'NONE', *, *, #9757, .T. ) ;
#11158 = CARTESIAN_POINT ( 'NONE',  ( 8.637616862297841536, -3.912171961291982747, 21.50000000000000000 ) ) ;
#11159 = EDGE_CURVE ( 'NONE', #27228, #8044, #29696, .T. ) ;
#11160 = CIRCLE ( 'NONE', #12151, 11.99999999999998224 ) ;
#11161 = EDGE_CURVE ( 'NONE', #7065, #22885, #22754, .T. ) ;
#11162 = DIRECTION ( 'NONE',  ( 1.000000000000000000, 0.000000000000000000, 0.000000000000000000 ) ) ;
#11163 = ORIENTED_EDGE ( 'NONE', *, *, #1023, .F. ) ;
#11164 = LINE ( 'NONE', #3831, #7829 ) ;
#11165 = CARTESIAN_POINT ( 'NONE',  ( 12.44336852771590962, 11.64466880974753416, 18.34727598691068096 ) ) ;
#11166 = DIRECTION ( 'NONE',  ( 1.000000000000000000, 0.000000000000000000, 0.000000000000000000 ) ) ;
#11167 = CARTESIAN_POINT ( 'NONE',  ( -48.60671492705895247, 69.95510233907151587, 17.36422100552513470 ) ) ;
#11168 = DIRECTION ( 'NONE',  ( 1.000000000000000000, 0.000000000000000000, 0.000000000000000000 ) ) ;
#11169 = PLANE ( 'NONE',  #15310 ) ;
#11170 = CARTESIAN_POINT ( 'NONE',  ( 49.99999999999998579, 70.00000000000000000, 12.49999999999999112 ) ) ;
#11171 = DIRECTION ( 'NONE',  ( 0.000000000000000000, -1.000000000000000000, 0.000000000000000000 ) ) ;
#11172 = CARTESIAN_POINT ( 'NONE',  ( -6.187077094091591789, 11.47693674426096955, 1.500000000000001332 ) ) ;
#11173 = PLANE ( 'NONE',  #124 ) ;
#11174 = VERTEX_POINT ( 'NONE', #12955 ) ;
#11175 = ORIENTED_EDGE ( 'NONE', *, *, #4955, .T. ) ;
#11176 = DIRECTION ( 'NONE',  ( 1.000000000000000000, 0.000000000000000000, 0.000000000000000000 ) ) ;
#11177 = AXIS2_PLACEMENT_3D ( 'NONE', #9331, #7462, #14011 ) ;
#11178 = DIRECTION ( 'NONE',  ( 0.000000000000000000, -1.132880637372608986E-16, 1.000000000000000000 ) ) ;
#11179 = CARTESIAN_POINT ( 'NONE',  ( -7.869584159753960861, 10.39565510934976977, 1.500000000000001332 ) ) ;
#11180 = B_SPLINE_CURVE_WITH_KNOTS ( 'NONE', 3,
 ( #4365, #2024, #11551, #21041, #25891, #9356, #30563, #23681, #6856, #28390, #7015, #16524, #2326, #21353, #16983, #17139, #295, #29315, #749, #10120, #10440, #14957, #24468, #24149, #3113, #12633, #22122, #5136, #5609, #26983 ),
 .UNSPECIFIED., .F., .F.,
 ( 4, 2, 2, 2, 2, 2, 2, 2, 2, 2, 2, 2, 2, 2, 4 ),
 ( 0.000000000000000000, 0.006058912026177337706, 0.009088368039266010029, 0.01060309604581034446, 0.01211782405235468062, 0.01817673607853203394, 0.02120619209162071667, 0.02423564810470939940, 0.03029456013088676139, 0.03332401614397544759, 0.03483874415051978202, 0.03635347215706412338, 0.04241238418324148884, 0.04544184019633017851, 0.04847129620941885431 ),
 .UNSPECIFIED. ) ;
#11181 = ORIENTED_EDGE ( 'NONE', *, *, #3233, .F. ) ;
#11182 = CARTESIAN_POINT ( 'NONE',  ( 23.16753609997519092, -35.74416776804734752, -13.16661218287092971 ) ) ;
#11183 = CARTESIAN_POINT ( 'NONE',  ( 37.16608720827707657, 36.86186943028246787, 57.49999999999999289 ) ) ;
#11184 = ORIENTED_EDGE ( 'NONE', *, *, #4203, .F. ) ;
#11185 = CARTESIAN_POINT ( 'NONE',  ( -11.33743862782229250, -16.47619710613050970, 19.08232364404840098 ) ) ;
#11186 = CARTESIAN_POINT ( 'NONE',  ( -24.03057240117691862, 26.57182937991348481, 24.50000000000000000 ) ) ;
#11187 = CARTESIAN_POINT ( 'NONE',  ( -6.091847012640411840, 42.00621603651080704, 28.88234630096432554 ) ) ;
#11188 = ORIENTED_EDGE ( 'NONE', *, *, #13585, .T. ) ;
#11189 = DIRECTION ( 'NONE',  ( -0.4154150130018972598, -0.9096319953545133341, 0.000000000000000000 ) ) ;
#11190 = ORIENTED_EDGE ( 'NONE', *, *, #11504, .F. ) ;
#11191 = FACE_OUTER_BOUND ( 'NONE', #30514, .T. ) ;
#11192 = FACE_OUTER_BOUND ( 'NONE', #29587, .T. ) ;
#11193 = ORIENTED_EDGE ( 'NONE', *, *, #13973, .F. ) ;
#11194 = EDGE_CURVE ( 'NONE', #27603, #23407, #1252, .T. ) ;
#11195 = VECTOR ( 'NONE', #28786, 1000.000000000000000 ) ;
#11196 = CARTESIAN_POINT ( 'NONE',  ( -39.52380524535903561, -7.028748154198949827, -6.500000000000000888 ) ) ;
#11197 = CARTESIAN_POINT ( 'NONE',  ( 30.22537216192871057, -26.86607088810509936, 30.37637886334946558 ) ) ;
#11198 = CARTESIAN_POINT ( 'NONE',  ( -8.413215745754975217, 3.196529495465474380, 21.50000000000000000 ) ) ;
#11199 = CARTESIAN_POINT ( 'NONE',  ( 17.22181377297005866, 14.41708049311048789, 1.500000000000000000 ) ) ;
#11200 = DIRECTION ( 'NONE',  ( 1.000000000000000000, 0.000000000000000000, 0.000000000000000000 ) ) ;
#11201 = CARTESIAN_POINT ( 'NONE',  ( -19.95825857724417318, 1.540497788607360086, 19.03762469184452755 ) ) ;
#11202 = FACE_BOUND ( 'NONE', #26647, .T. ) ;
#11203 = ORIENTED_EDGE ( 'NONE', *, *, #29175, .T. ) ;
#11204 = EDGE_CURVE ( 'NONE', #281, #16514, #5272, .T. ) ;
#11205 = LINE ( 'NONE', #13413, #15748 ) ;
#11206 = CARTESIAN_POINT ( 'NONE',  ( 27.03943647958860197, -26.20092231554396633, 27.50000000000001066 ) ) ;
#11207 = VERTEX_POINT ( 'NONE', #8586 ) ;
#11208 = ORIENTED_EDGE ( 'NONE', *, *, #12202, .F. ) ;
#11209 = CARTESIAN_POINT ( 'NONE',  ( 8.999114229549594057, -0.1262659238204522361, 1.500000000000001332 ) ) ;
#11210 = CARTESIAN_POINT ( 'NONE',  ( -5.151082791877244382, 19.34385597943987989, 6.111214848085761986 ) ) ;
#11211 = ORIENTED_EDGE ( 'NONE', *, *, #15638, .F. ) ;
#11212 = DIRECTION ( 'NONE',  ( 1.000000000000000000, 0.000000000000000000, 0.000000000000000000 ) ) ;
#11213 = CARTESIAN_POINT ( 'NONE',  ( -9.033033306777449312, 0.9621688436940325495, 21.50000000000000000 ) ) ;
#11214 = CIRCLE ( 'NONE', #20161, 0.7500000000000015543 ) ;
#11215 = CARTESIAN_POINT ( 'NONE',  ( -30.53339558441486190, 7.800891647352838909, 43.48653168448687012 ) ) ;
#11216 = ORIENTED_EDGE ( 'NONE', *, *, #18202, .F. ) ;
#11217 = DIRECTION ( 'NONE',  ( -0.000000000000000000, -0.000000000000000000, 1.000000000000000000 ) ) ;
#11218 =( REPRESENTATION_RELATIONSHIP ('NONE','NONE', #19885, #10307 ) REPRESENTATION_RELATIONSHIP_WITH_TRANSFORMATION ( #20603 )SHAPE_REPRESENTATION_RELATIONSHIP( ) );
#11219 = CARTESIAN_POINT ( 'NONE',  ( -33.42925964089141644, -11.06161099612212695, 39.78814634291941843 ) ) ;
#11220 = ORIENTED_EDGE ( 'NONE', *, *, #22415, .T. ) ;
#11221 = ORIENTED_EDGE ( 'NONE', *, *, #11867, .T. ) ;
#11222 = CARTESIAN_POINT ( 'NONE',  ( -30.26724724044731829, 27.72993536917570623, -6.500000000000000888 ) ) ;
#11223 = ORIENTED_EDGE ( 'NONE', *, *, #14318, .F. ) ;
#11224 = ORIENTED_EDGE ( 'NONE', *, *, #7710, .F. ) ;
#11225 = EDGE_CURVE ( 'NONE', #12499, #27312, #17736, .T. ) ;
#11226 = CARTESIAN_POINT ( 'NONE',  ( -18.35575104603286078, -7.986347210076461423, 5.940635272151477686 ) ) ;
#11227 = CARTESIAN_POINT ( 'NONE',  ( 39.99999999999998579, 87.00000000000001421, 22.49999999999999289 ) ) ;
#11228 = LINE ( 'NONE', #27316, #875 ) ;
#11229 = EDGE_LOOP ( 'NONE', ( #10178, #14081, #10156, #25304, #67, #2123 ) ) ;
#11230 = CIRCLE ( 'NONE', #28671, 1.447898107987198646 ) ;
#11231 = CARTESIAN_POINT ( 'NONE',  ( -34.13832859401788511, 12.80067323710188276, 34.80090346875805807 ) ) ;
#11232 = CARTESIAN_POINT ( 'NONE',  ( -27.03074382657074537, 6.449748410230984774, 42.96778633356043287 ) ) ;
#11233 = CARTESIAN_POINT ( 'NONE',  ( 19.77948086832033425, 3.081792779576177033, 20.34789198813115263 ) ) ;
#11234 = ORIENTED_EDGE ( 'NONE', *, *, #15708, .F. ) ;
#11235 = EDGE_CURVE ( 'NONE', #52, #946, #12797, .T. ) ;
#11236 = CARTESIAN_POINT ( 'NONE',  ( -16.86183147812083760, 2.368508504629200484, 20.05479082170252525 ) ) ;
#11237 = CARTESIAN_POINT ( 'NONE',  ( 17.99082164042340537, -8.777603813954270251, 7.176035686813569292 ) ) ;
#11238 = CARTESIAN_POINT ( 'NONE',  ( -13.51981801095249835, 10.39108251695558316, 20.32367522806703874 ) ) ;
#11239 = CARTESIAN_POINT ( 'NONE',  ( 5.159688198573267215, 19.34150021954530274, 20.33971507717571114 ) ) ;
#11240 = VERTEX_POINT ( 'NONE', #17782 ) ;
#11241 = ORIENTED_EDGE ( 'NONE', *, *, #8786, .F. ) ;
#11242 = DIRECTION ( 'NONE',  ( -1.000000000000000000, 0.000000000000000000, 0.000000000000000000 ) ) ;
#11243 = CARTESIAN_POINT ( 'NONE',  ( 0.000000000000000000, 0.000000000000000000, 1.500000000000000000 ) ) ;
#11244 = DIRECTION ( 'NONE',  ( 1.000000000000000000, 0.000000000000000000, -0.000000000000000000 ) ) ;
#11245 = CARTESIAN_POINT ( 'NONE',  ( -5.151082791877242606, 19.34385597943988344, 18.80699882434806369 ) ) ;
#11246 = DIRECTION ( 'NONE',  ( -0.000000000000000000, -0.000000000000000000, 1.000000000000000000 ) ) ;
#11247 = DIRECTION ( 'NONE',  ( -0.000000000000000000, -0.000000000000000000, -1.000000000000000000 ) ) ;
#11248 = VECTOR ( 'NONE', #14483, 1000.000000000000114 ) ;
#11249 = CARTESIAN_POINT ( 'NONE',  ( 29.61203839202725518, -15.40012917324033381, 37.38016955275580244 ) ) ;
#11250 = DIRECTION ( 'NONE',  ( 0.000000000000000000, 0.000000000000000000, 1.000000000000000000 ) ) ;
#11251 = EDGE_LOOP ( 'NONE', ( #22935, #2384, #18490, #24578, #13485, #11601 ) ) ;
#11252 = CARTESIAN_POINT ( 'NONE',  ( -17.06520330450695866, 0.6550632133703672144, 6.447548852708279377 ) ) ;
#11253 = CYLINDRICAL_SURFACE ( 'NONE', #16195, 19.49999999999996447 ) ;
#11254 = CARTESIAN_POINT ( 'NONE',  ( 27.03074382657074537, 6.449748410230989215, 47.21042702067963148 ) ) ;
#11255 = EDGE_LOOP ( 'NONE', ( #7759, #16311, #29229, #4696 ) ) ;
#11256 = AXIS2_PLACEMENT_3D ( 'NONE', #23480, #16936, #26454 ) ;
#11257 = DIRECTION ( 'NONE',  ( -0.000000000000000000, -0.000000000000000000, 1.000000000000000000 ) ) ;
#11258 = EDGE_CURVE ( 'NONE', #11338, #5002, #7271, .T. ) ;
#11259 = ORIENTED_EDGE ( 'NONE', *, *, #28016, .T. ) ;
#11260 = ADVANCED_FACE ( 'NONE', ( #15586 ), #20428, .F. ) ;
#11261 = CARTESIAN_POINT ( 'NONE',  ( 18.48560952955220316, -7.681425967031917601, 5.704143890883081269 ) ) ;
#11262 = CARTESIAN_POINT ( 'NONE',  ( -27.03074382657074537, -6.449748410230988327, 42.96778633356042576 ) ) ;
#11263 = EDGE_CURVE ( 'NONE', #15560, #4711, #25709, .T. ) ;
#11264 = ORIENTED_EDGE ( 'NONE', *, *, #5780, .F. ) ;
#11265 = CARTESIAN_POINT ( 'NONE',  ( 0.6237340761795171495, -8.999114229549588728, -3.621320343559650379 ) ) ;
#11266 = EDGE_CURVE ( 'NONE', #27939, #24466, #783, .T. ) ;
#11267 = DIRECTION ( 'NONE',  ( -0.000000000000000000, -0.000000000000000000, 1.000000000000000000 ) ) ;
#11268 = EDGE_CURVE ( 'NONE', #4505, #25524, #10927, .T. ) ;
#11269 = CARTESIAN_POINT ( 'NONE',  ( -50.00000000000000000, 50.00000000000000000, -87.50000000000000000 ) ) ;
#11270 = CARTESIAN_POINT ( 'NONE',  ( -21.90865045291186775, -23.69204963285888610, -16.50001200000000168 ) ) ;
#11271 = DIRECTION ( 'NONE',  ( -1.000000000000000000, 0.000000000000000000, 0.000000000000000000 ) ) ;
#11272 = AXIS2_PLACEMENT_3D ( 'NONE', #2606, #26786, #5412 ) ;
#11273 = DIRECTION ( 'NONE',  ( 0.000000000000000000, -0.5000000000000006661, -0.8660254037844382635 ) ) ;
#11274 = CARTESIAN_POINT ( 'NONE',  ( 0.6820093937066838974, -20.00641896168558986, 7.603368798681074736 ) ) ;
#11275 = CARTESIAN_POINT ( 'NONE',  ( -3.469446951953614189E-15, -30.50000000000000711, 24.50000000000000000 ) ) ;
#11276 = EDGE_CURVE ( 'NONE', #29673, #13769, #22448, .T. ) ;
#11277 = VERTEX_POINT ( 'NONE', #10607 ) ;
#11278 = EDGE_CURVE ( 'NONE', #10066, #18622, #957, .T. ) ;
#11279 = CARTESIAN_POINT ( 'NONE',  ( 26.73000961532937225, -9.331429872129930914, 1.500000000000000000 ) ) ;
#11280 = DIRECTION ( 'NONE',  ( -0.000000000000000000, -0.000000000000000000, 1.000000000000000000 ) ) ;
#11281 = EDGE_LOOP ( 'NONE', ( #4604, #15230, #8934, #10477 ) ) ;
#11282 = CARTESIAN_POINT ( 'NONE',  ( -23.07950435457407679, -11.50806656539752737, -16.55003854064094426 ) ) ;
#11284 = EDGE_CURVE ( 'NONE', #19542, #23909, #15426, .T. ) ;
#11283 = AXIS2_PLACEMENT_3D ( 'NONE', #21183, #19173, #14030 ) ;
#11285 = CARTESIAN_POINT ( 'NONE',  ( -17.60607916434270237, -9.525343863633434438, 19.14333282897057842 ) ) ;
#11286 = AXIS2_PLACEMENT_3D ( 'NONE', #13157, #22816, #1467 ) ;
#11287 = CARTESIAN_POINT ( 'NONE',  ( 0.8038475772933696417, 10.39230484541327471, -1.336447385876663028E-16 ) ) ;
#11288 = CIRCLE ( 'NONE', #24227, 0.6002263538043630664 ) ;
#11289 = CARTESIAN_POINT ( 'NONE',  ( 35.76344986163714168, -22.29344514668044752, -19.50000000000000355 ) ) ;
#11290 = ORIENTED_EDGE ( 'NONE', *, *, #21603, .F. ) ;
#11291 = LINE ( 'NONE', #23128, #1955 ) ;
#11292 = LINE ( 'NONE', #9415, #3699 ) ;
#11293 = CARTESIAN_POINT ( 'NONE',  ( 30.96729785525396395, -21.29736153647971619, 37.49999999991082689 ) ) ;
#11294 = LINE ( 'NONE', #20792, #8176 ) ;
#11295 = VERTEX_POINT ( 'NONE', #13110 ) ;
#11296 = B_SPLINE_CURVE_WITH_KNOTS ( 'NONE', 3,
 ( #16946, #29109, #21774, #12122, #24421, #2452, #26465, #23957, #17254, #9624, #413, #11803, #9770, #105, #5096, #19441, #28651, #14609 ),
 .UNSPECIFIED., .F., .F.,
 ( 4, 2, 2, 2, 2, 2, 2, 2, 4 ),
 ( 0.000000000000000000, 0.0003967869494442875051, 0.0007935738988885750102, 0.001190360848332862407, 0.001587147797777150020, 0.001983934747221437634, 0.002380721696665724814, 0.002777508646110012427, 0.003174295595554300041 ),
 .UNSPECIFIED. ) ;
#11297 = CARTESIAN_POINT ( 'NONE',  ( -14.01114995435608179, 9.765040422203638215, 6.588756557121049795 ) ) ;
#11298 = CARTESIAN_POINT ( 'NONE',  ( -20.71335220384823117, -27.86167394782616213, -16.50000000000000000 ) ) ;
#11299 = CARTESIAN_POINT ( 'NONE',  ( 2.599508007902112006, 14.29059753516471964, 1.500000000000000000 ) ) ;
#11300 = CIRCLE ( 'NONE', #28726, 0.7500000000000006661 ) ;
#11301 = EDGE_CURVE ( 'NONE', #2551, #6787, #15119, .T. ) ;
#11302 = ORIENTED_EDGE ( 'NONE', *, *, #28196, .T. ) ;
#11303 = EDGE_CURVE ( 'NONE', #8240, #8380, #2158, .T. ) ;
#11304 = ADVANCED_FACE ( 'NONE', ( #16198 ), #13574, .F. ) ;
#11305 = CIRCLE ( 'NONE', #24738, 9.084132297865673777 ) ;
#11306 = CARTESIAN_POINT ( 'NONE',  ( 19.56124041029250904, 4.166605025611204383, 19.61564845152807735 ) ) ;
#11307 = ORIENTED_EDGE ( 'NONE', *, *, #30007, .F. ) ;
#11308 = CARTESIAN_POINT ( 'NONE',  ( -30.74147208807243814, -15.49548351932574697, 40.57409041152976670 ) ) ;
#11309 = AXIS2_PLACEMENT_3D ( 'NONE', #30140, #8770, #3638 ) ;
#11310 = AXIS2_PLACEMENT_3D ( 'NONE', #13996, #27738, #13851 ) ;
#11311 = EDGE_CURVE ( 'NONE', #11004, #4539, #13260, .T. ) ;
#11312 = AXIS2_PLACEMENT_3D ( 'NONE', #19413, #7411, #23608 ) ;
#11313 = CARTESIAN_POINT ( 'NONE',  ( -8.134323311075783991, -1.438332125858144295, 21.50000000000000000 ) ) ;
#11314 = CYLINDRICAL_SURFACE ( 'NONE', #22296, 0.9999999999999983347 ) ;
#11315 = VERTEX_POINT ( 'NONE', #8890 ) ;
#11316 = CARTESIAN_POINT ( 'NONE',  ( 11.80353037513723713, 12.33292095759475338, 18.73314399819312115 ) ) ;
#11317 = CARTESIAN_POINT ( 'NONE',  ( 16.55527708515956675, 4.194179076328800271, 6.588756557121050683 ) ) ;
#11318 = CARTESIAN_POINT ( 'NONE',  ( -4.163336342344337027E-14, 1.387778780781445676E-14, 62.49999999999999289 ) ) ;
#11319 = EDGE_CURVE ( 'NONE', #16485, #11391, #3905, .T. ) ;
#11320 = DIRECTION ( 'NONE',  ( 0.000000000000000000, 0.000000000000000000, -1.000000000000000000 ) ) ;
#11321 = CIRCLE ( 'NONE', #19788, 9.482273699623480212 ) ;
#11322 = CARTESIAN_POINT ( 'NONE',  ( 22.94541271838008356, -35.03073867843704647, -6.500000000000000888 ) ) ;
#11323 =( BOUNDED_SURFACE ( )  B_SPLINE_SURFACE ( 3, 1, ( 
 ( #16875, #19370 ),
 ( #30753, #11730 ),
 ( #28890, #9694 ),
 ( #23721, #2370 ) ),
 .UNSPECIFIED., .F., .F., .T. ) 
 B_SPLINE_SURFACE_WITH_KNOTS ( ( 4, 4 ),
 ( 2, 2 ),
 ( 0.000000000000000000, 1.000000000000000000 ),
 ( 0.000000000000000000, 1.000000000000000000 ),
 .UNSPECIFIED. ) 
 GEOMETRIC_REPRESENTATION_ITEM ( )  RATIONAL_B_SPLINE_SURFACE ( (
 ( 1.000000000000000000, 1.000000000000000000),
 ( 0.9908525036704132205, 0.9908525036704132205),
 ( 0.9908525036704132205, 0.9908525036704132205),
 ( 1.000000000000000000, 1.000000000000000000) ) ) 
 REPRESENTATION_ITEM ( '' )  SURFACE ( )  );
#11324 = CARTESIAN_POINT ( 'NONE',  ( 0.000000000000000000, 1.604273173167211147E-31, -87.50000000000000000 ) ) ;
#11325 = PLANE ( 'NONE',  #74 ) ;
#11326 = CARTESIAN_POINT ( 'NONE',  ( 39.52380524533145945, -7.028748154382054913, -11.49999999999999645 ) ) ;
#11327 = FACE_OUTER_BOUND ( 'NONE', #21766, .T. ) ;
#11328 = CARTESIAN_POINT ( 'NONE',  ( -15.54251014615008941, -6.943938207015637687, 19.77662771831109367 ) ) ;
#11329 = CARTESIAN_POINT ( 'NONE',  ( -8.658642353097244282, -14.67867993405429772, 18.34727598691068096 ) ) ;
#11330 = AXIS2_PLACEMENT_3D ( 'NONE', #9076, #16394, #15950 ) ;
#11331 = ORIENTED_EDGE ( 'NONE', *, *, #22687, .F. ) ;
#11332 = VERTEX_POINT ( 'NONE', #23515 ) ;
#11333 = VECTOR ( 'NONE', #9768, 1000.000000000000000 ) ;
#11334 = CARTESIAN_POINT ( 'NONE',  ( 33.42925964089140933, 11.06161099612213405, -16.55003854064094426 ) ) ;
#11335 = CARTESIAN_POINT ( 'NONE',  ( -7.700393225236267902, -15.24241778594199737, 6.392658652357120275 ) ) ;
#11336 = EDGE_CURVE ( 'NONE', #29934, #10944, #20202, .T. ) ;
#11337 = CARTESIAN_POINT ( 'NONE',  ( 0.000000000000000000, 39.50000000000000000, 37.50000000000000000 ) ) ;
#11338 = VERTEX_POINT ( 'NONE', #23053 ) ;
#11339 = DIRECTION ( 'NONE',  ( 1.000000000000000000, 0.000000000000000000, 0.000000000000000000 ) ) ;
#11340 = ADVANCED_FACE ( 'NONE', ( #6834 ), #27916, .F. ) ;
#11341 = AXIS2_PLACEMENT_3D ( 'NONE', #26777, #12898, #6015 ) ;
#11342 = CARTESIAN_POINT ( 'NONE',  ( 18.02181326450767784, -8.714141732420079833, 18.71435384576123440 ) ) ;
#11343 = CARTESIAN_POINT ( 'NONE',  ( 9.118789845653434867, -14.37574228027166434, 18.83976166372255534 ) ) ;
#11344 = CIRCLE ( 'NONE', #3360, 5.000000000000004441 ) ;
#11345 = ORIENTED_EDGE ( 'NONE', *, *, #26947, .T. ) ;
#11346 = CARTESIAN_POINT ( 'NONE',  ( -16.93638505691475871, 1.872096242067389227, 5.670038381137163519 ) ) ;
#11347 = VECTOR ( 'NONE', #170, 1000.000000000000000 ) ;
#11348 = AXIS2_PLACEMENT_3D ( 'NONE', #12277, #12591, #28961 ) ;
#11349 = DIRECTION ( 'NONE',  ( 1.000000000000000000, 0.000000000000000000, 0.000000000000000000 ) ) ;
#11350 = CARTESIAN_POINT ( 'NONE',  ( -14.09828636627701925, 39.65347080688651715, 29.09260480754099021 ) ) ;
#11351 = ORIENTED_EDGE ( 'NONE', *, *, #8094, .F. ) ;
#11352 = DIRECTION ( 'NONE',  ( 1.000000000000000000, 0.000000000000000000, 0.000000000000000000 ) ) ;
#11353 = ORIENTED_EDGE ( 'NONE', *, *, #26337, .T. ) ;
#11354 = VECTOR ( 'NONE', #17957, 1000.000000000000114 ) ;
#11355 = DIRECTION ( 'NONE',  ( 0.000000000000000000, 1.000000000000000000, 1.193512090021232842E-16 ) ) ;
#11356 = CARTESIAN_POINT ( 'NONE',  ( 9.999999999999959144, 1.510243460696181139E-14, 1.500000000000000000 ) ) ;
#11357 = CIRCLE ( 'NONE', #26302, 9.482273699623480212 ) ;
#11358 = VERTEX_POINT ( 'NONE', #23371 ) ;
#11359 = VECTOR ( 'NONE', #19130, 1000.000000000000000 ) ;
#11360 = DIRECTION ( 'NONE',  ( -0.000000000000000000, -0.000000000000000000, 1.000000000000000000 ) ) ;
#11361 = CYLINDRICAL_SURFACE ( 'NONE', #17208, 7.500000000000007994 ) ;
#11362 = CARTESIAN_POINT ( 'NONE',  ( 0.7788148816922453310, -17.02744011591805062, 7.652108011868850923 ) ) ;
#11363 = CARTESIAN_POINT ( 'NONE',  ( -7.488956955540436056, -5.141690706682852330, 21.50000000000000000 ) ) ;
#11364 = FACE_OUTER_BOUND ( 'NONE', #11090, .T. ) ;
#11365 = CARTESIAN_POINT ( 'NONE',  ( -17.05632420042081776, 0.7692048344978460461, 18.84329447212444109 ) ) ;
#11366 = DIRECTION ( 'NONE',  ( 0.000000000000000000, 0.000000000000000000, -1.000000000000000000 ) ) ;
#11367 = DIRECTION ( 'NONE',  ( 0.000000000000000000, 0.000000000000000000, 1.000000000000000000 ) ) ;
#11368 = ORIENTED_EDGE ( 'NONE', *, *, #21194, .T. ) ;
#11369 = VECTOR ( 'NONE', #2500, 1000.000000000000000 ) ;
#11370 = AXIS2_PLACEMENT_3D ( 'NONE', #9769, #14454, #5095 ) ;
#11371 = CARTESIAN_POINT ( 'NONE',  ( 10.30429258806635140, -13.59853737800766815, 20.19593175699879595 ) ) ;
#11372 = FACE_OUTER_BOUND ( 'NONE', #12158, .T. ) ;
#11373 = ORIENTED_EDGE ( 'NONE', *, *, #3164, .T. ) ;
#11374 = ORIENTED_EDGE ( 'NONE', *, *, #21748, .T. ) ;
#11375 = CARTESIAN_POINT ( 'NONE',  ( 0.000000000000000000, 0.000000000000000000, 21.50000000000000000 ) ) ;
#11376 = EDGE_CURVE ( 'NONE', #8129, #28377, #12781, .T. ) ;
#11377 = ORIENTED_EDGE ( 'NONE', *, *, #23145, .F. ) ;
#11378 = AXIS2_PLACEMENT_3D ( 'NONE', #10145, #24169, #25803 ) ;
#11379 = CARTESIAN_POINT ( 'NONE',  ( -37.99999999999999289, 209.2686044187655909, -28.49999999999998934 ) ) ;
#11380 = CIRCLE ( 'NONE', #18347, 9.084132297865673777 ) ;
#11381 = CARTESIAN_POINT ( 'NONE',  ( 4.510281037539698445E-13, -4.926614671774132148E-13, 82.49999999999998579 ) ) ;
#11382 = VERTEX_POINT ( 'NONE', #30687 ) ;
#11383 = CARTESIAN_POINT ( 'NONE',  ( -15.34618562042307843, 12.82554431217322310, 18.34798005863227388 ) ) ;
#11384 = LINE ( 'NONE', #13430, #19962 ) ;
#11385 = ORIENTED_EDGE ( 'NONE', *, *, #232, .T. ) ;
#11386 = CARTESIAN_POINT ( 'NONE',  ( 6.899999999999999467, 5.196152422706634688, -9.000000000000001776 ) ) ;
#11387 = VERTEX_POINT ( 'NONE', #20714 ) ;
#11388 = AXIS2_PLACEMENT_3D ( 'NONE', #1086, #10601, #3897 ) ;
#11389 = CARTESIAN_POINT ( 'NONE',  ( -22.94541271838176044, 35.03073867844246081, -6.500000000000000888 ) ) ;
#11390 = AXIS2_PLACEMENT_3D ( 'NONE', #8330, #7864, #5983 ) ;
#11391 = VERTEX_POINT ( 'NONE', #16360 ) ;
#11392 = CIRCLE ( 'NONE', #28820, 0.7500000000000006661 ) ;
#11393 = ORIENTED_EDGE ( 'NONE', *, *, #19501, .T. ) ;
#11394 = CARTESIAN_POINT ( 'NONE',  ( -40.00000000000002842, 80.00000000000001421, 22.49999999999983302 ) ) ;
#11395 = CARTESIAN_POINT ( 'NONE',  ( -18.04156136322729864, -8.631457789788587576, 5.652196082369963293 ) ) ;
#11396 = AXIS2_PLACEMENT_3D ( 'NONE', #17160, #11461, #9111 ) ;
#11397 = CARTESIAN_POINT ( 'NONE',  ( -32.31576317091163730, -17.59561277345963148, 34.80090346875804386 ) ) ;
#11398 = DIRECTION ( 'NONE',  ( -0.000000000000000000, -0.000000000000000000, 1.000000000000000000 ) ) ;
#11399 = FACE_BOUND ( 'NONE', #20230, .T. ) ;
#11400 = ORIENTED_EDGE ( 'NONE', *, *, #25059, .F. ) ;
#11401 = DIRECTION ( 'NONE',  ( -0.2972711322815274615, 0.9547931052914335748, -0.000000000000000000 ) ) ;
#11402 = CARTESIAN_POINT ( 'NONE',  ( 15.40685886292497386, -7.237730981567048083, 6.974106381145714018 ) ) ;
#11403 = CARTESIAN_POINT ( 'NONE',  ( -15.98601489809224319, 12.04791232832105408, 6.782048567692550378 ) ) ;
#11404 = CARTESIAN_POINT ( 'NONE',  ( 3.060137030613564235, 16.80197902060524484, 19.25672174529527325 ) ) ;
#11405 = EDGE_LOOP ( 'NONE', ( #2862, #19933, #25941, #15651, #27631, #24934, #27079, #5451, #8321, #659, #2590, #14050, #7290, #15593, #7806, #14195, #7236, #28017, #11989, #20250, #9767, #8748, #14861, #11959, #25877, #2889, #2279, #5309, #8313, #15787, #30351, #30285, #8778, #5537, #17466, #30268, #20263, #13258, #29699, #9546, #12356, #28921, #14941, #2868, #12347, #22088, #16854, #25578, #2078, #10625, #23424, #15765, #2976, #13322, #7267, #8437, #28511, #17706, #17833, #7599, #133, #9187, #19536, #24547, #26616, #3716, #21084, #26179, #24583, #13905, #23017, #6225, #22681, #29519, #29476, #22059, #15747, #29058, #19107, #27067, #22011, #22089, #13599 ) ) ;
#11406 = ORIENTED_EDGE ( 'NONE', *, *, #8081, .F. ) ;
#11407 = CARTESIAN_POINT ( 'NONE',  ( 32.87304123117094434, -22.86929295230439152, 18.00000000000000355 ) ) ;
#11408 = CARTESIAN_POINT ( 'NONE',  ( -15.75339717617903545, 12.35099711776840081, 7.441806358946449151 ) ) ;
#11409 = CARTESIAN_POINT ( 'NONE',  ( 10.69237140622465532, -13.31695822555149356, 6.783738457429053348 ) ) ;
#11410 = B_SPLINE_SURFACE_WITH_KNOTS ( 'NONE', 3, 1, ( 
 ( #2728, #29081 ),
 ( #21736, #10053 ),
 ( #17065, #7874 ),
 ( #27052, #22047 ),
 ( #19877, #5524 ),
 ( #9734, #7410 ),
 ( #22205, #7722 ),
 ( #29394, #16918 ),
 ( #378, #26594 ),
 ( #8029, #15027 ),
 ( #19561, #24079 ),
 ( #5373, #24541 ),
 ( #3189, #17533 ),
 ( #14721, #14426 ),
 ( #684, #24230 ),
 ( #7563, #10201 ),
 ( #14880, #21901 ),
 ( #23929, #19709 ),
 ( #21588, #221 ),
 ( #19247, #26434 ),
 ( #5067, #9897 ),
 ( #19412, #28929 ),
 ( #2879, #529 ),
 ( #13016, #10512 ),
 ( #24694, #22824 ),
 ( #15495, #25012 ),
 ( #8507, #18009 ),
 ( #27518, #6137 ),
 ( #29541, #30008 ),
 ( #8645, #1005 ),
 ( #8179, #22969 ) ),
 .UNSPECIFIED., .F., .F., .F.,
 ( 4, 3, 3, 3, 3, 3, 3, 3, 3, 3, 4 ),
 ( 2, 2 ),
 ( 0.4999999998345681651, 0.5360336730431942698, 0.5907651151589017324, 0.6456034593241839481, 0.6998270958050443191, 0.7529536536315944995, 0.8052385063053264513, 0.8575343587103996246, 0.9106564858195047574, 0.9648414833209688624, 1.000000006602610014 ),
 ( 0.000000000000000000, 1.000000000000000000 ),
 .UNSPECIFIED. ) ;
#11411 = CARTESIAN_POINT ( 'NONE',  ( 13.01350570279884700, 10.97146294988703907, 6.714907520933422802 ) ) ;
#11412 = DIRECTION ( 'NONE',  ( 0.000000000000000000, 0.000000000000000000, -1.000000000000000000 ) ) ;
#11413 = AXIS2_PLACEMENT_3D ( 'NONE', #2577, #5069, #11947 ) ;
#11414 = CIRCLE ( 'NONE', #23353, 9.000000000000000000 ) ;
#11415 = CARTESIAN_POINT ( 'NONE',  ( -12.08674330573844813, 37.23003549701822834, 27.50000000000000355 ) ) ;
#11416 = CONTEXT_DEPENDENT_SHAPE_REPRESENTATION ( #12822, #2705 ) ;
#11417 = CARTESIAN_POINT ( 'NONE',  ( 23.21352257770656635, -10.78826658734920052, 49.40206402021031806 ) ) ;
#11418 = ORIENTED_EDGE ( 'NONE', *, *, #15070, .T. ) ;
#11419 = CARTESIAN_POINT ( 'NONE',  ( -19.94989956810792009, 1.646935350084929972, 7.196036389296800451 ) ) ;
#11420 = VECTOR ( 'NONE', #27874, 1000.000000000000000 ) ;
#11421 = DIRECTION ( 'NONE',  ( -1.000000000000000000, 0.000000000000000000, 0.000000000000000000 ) ) ;
#11422 = CARTESIAN_POINT ( 'NONE',  ( 19.87646685382694756, 2.220054991963869462, 19.60917204426170457 ) ) ;
#11423 = ORIENTED_EDGE ( 'NONE', *, *, #29576, .F. ) ;
#11424 = LINE ( 'NONE', #30436, #21777 ) ;
#11425 = ORIENTED_EDGE ( 'NONE', *, *, #6869, .F. ) ;
#11426 = CARTESIAN_POINT ( 'NONE',  ( 4.608906612435600181, 7.730328572437758616, -1.500000000000000888 ) ) ;
#11427 = CIRCLE ( 'NONE', #17909, 0.7500000000000001110 ) ;
#11428 = DIRECTION ( 'NONE',  ( -0.000000000000000000, -0.000000000000000000, 1.000000000000000000 ) ) ;
#11429 = ORIENTED_EDGE ( 'NONE', *, *, #5452, .F. ) ;
#11430 = LINE ( 'NONE', #11265, #26787 ) ;
#11431 = CARTESIAN_POINT ( 'NONE',  ( 77.99999999999998579, 42.50000000000000711, 1.500000000000001110 ) ) ;
#11432 = CARTESIAN_POINT ( 'NONE',  ( -3.576392677004104570, -42.36439329621270389, 19.83430273327883953 ) ) ;
#11433 = CARTESIAN_POINT ( 'NONE',  ( -20.48466473087059114, -26.10042409808303887, -16.50001200000000523 ) ) ;
#11434 = CARTESIAN_POINT ( 'NONE',  ( -52.99999999999955236, -4.926614671774132148E-13, 65.49999999999998579 ) ) ;
#11435 = LINE ( 'NONE', #27510, #2875 ) ;
#11436 = DIRECTION ( 'NONE',  ( -0.000000000000000000, 1.132880637372608986E-16, -1.000000000000000000 ) ) ;
#11437 = ORIENTED_EDGE ( 'NONE', *, *, #3732, .T. ) ;
#11438 = VECTOR ( 'NONE', #2652, 1000.000000000000000 ) ;
#11439 = DIRECTION ( 'NONE',  ( 1.000000000000000000, 0.000000000000000000, 0.000000000000000000 ) ) ;
#11440 = CARTESIAN_POINT ( 'NONE',  ( 22.58267429318971864, 26.57182937991349903, 1.500000000000001332 ) ) ;
#11441 = ADVANCED_FACE ( 'NONE', ( #13428 ), #30093, .F. ) ;
#11442 = ORIENTED_EDGE ( 'NONE', *, *, #8452, .T. ) ;
#11443 = DIRECTION ( 'NONE',  ( -0.000000000000000000, -0.000000000000000000, 1.000000000000000000 ) ) ;
#11444 = CARTESIAN_POINT ( 'NONE',  ( -15.09693789817080223, -7.923486267757676060, 18.35718225375110180 ) ) ;
#11445 = CARTESIAN_POINT ( 'NONE',  ( 31.18700685317022803, -26.11823559933272421, -1.500000000000000000 ) ) ;
#11446 = AXIS2_PLACEMENT_3D ( 'NONE', #25911, #4390, #23250 ) ;
#11447 = CARTESIAN_POINT ( 'NONE',  ( 10.64374042650304020, -42.96126232887725394, -19.50000000000000355 ) ) ;
#11448 = ORIENTED_EDGE ( 'NONE', *, *, #10768, .F. ) ;
#11449 = DIRECTION ( 'NONE',  ( 1.000000000000000000, 0.000000000000000000, 0.000000000000000000 ) ) ;
#11450 = DIRECTION ( 'NONE',  ( -1.000000000000000000, 0.000000000000000000, 0.000000000000000000 ) ) ;
#11451 = CARTESIAN_POINT ( 'NONE',  ( 24.35498655531922196, -28.61621432983365665, 37.50000000002946621 ) ) ;
#11452 = EDGE_CURVE ( 'NONE', #22188, #154, #9275, .T. ) ;
#11453 = DIRECTION ( 'NONE',  ( -0.000000000000000000, -0.000000000000000000, 1.000000000000000000 ) ) ;
#11454 = ORIENTED_EDGE ( 'NONE', *, *, #7084, .T. ) ;
#11455 = LINE ( 'NONE', #24199, #22614 ) ;
#11456 = ORIENTED_EDGE ( 'NONE', *, *, #1825, .F. ) ;
#11457 = CARTESIAN_POINT ( 'NONE',  ( -31.18700685316100163, -26.11823559932341610, -1.500000000000000000 ) ) ;
#11458 = DIRECTION ( 'NONE',  ( -0.000000000000000000, 0.000000000000000000, 1.000000000000000000 ) ) ;
#11459 = VERTEX_POINT ( 'NONE', #25570 ) ;
#11460 = EDGE_CURVE ( 'NONE', #28009, #7211, #8728, .T. ) ;
#11461 = DIRECTION ( 'NONE',  ( -0.000000000000000000, -1.000000000000000000, -0.000000000000000000 ) ) ;
#11462 = ORIENTED_EDGE ( 'NONE', *, *, #29004, .F. ) ;
#11463 = DIRECTION ( 'NONE',  ( 0.000000000000000000, 0.000000000000000000, -1.000000000000000000 ) ) ;
#11464 = ADVANCED_FACE ( 'NONE', ( #13716 ), #27763, .T. ) ;
#11465 = CARTESIAN_POINT ( 'NONE',  ( 17.75446986341059841, 9.207540381081344094, 1.500000000000001332 ) ) ;
#11466 = VECTOR ( 'NONE', #18654, 1000.000000000000227 ) ;
#11467 = DIRECTION ( 'NONE',  ( 0.000000000000000000, -0.000000000000000000, -1.000000000000000000 ) ) ;
#11468 = DIRECTION ( 'NONE',  ( 1.000000000000000000, 0.000000000000000000, 0.000000000000000000 ) ) ;
#11469 = ORIENTED_EDGE ( 'NONE', *, *, #28801, .T. ) ;
#11470 = CARTESIAN_POINT ( 'NONE',  ( 11.75175153055562838, 12.38566219040472305, 19.85459532544248162 ) ) ;
#11471 = CARTESIAN_POINT ( 'NONE',  ( 12.35522425158188931, 11.74279415389956327, 18.34798005863078885 ) ) ;
#11472 = DIRECTION ( 'NONE',  ( 0.000000000000000000, 0.000000000000000000, 1.000000000000000000 ) ) ;
#11473 = CARTESIAN_POINT ( 'NONE',  ( -15.13937296497744178, 13.09668952202109438, 18.39701043959520987 ) ) ;
#11474 = CARTESIAN_POINT ( 'NONE',  ( -49.32716953814647809, 69.98911764784745060, 18.87824250137748550 ) ) ;
#11475 = DIRECTION ( 'NONE',  ( -0.000000000000000000, -0.000000000000000000, 1.000000000000000000 ) ) ;
#11476 = CARTESIAN_POINT ( 'NONE',  ( -12.85122823560700134, 11.16779817461281432, 18.72771030977187579 ) ) ;
#11477 = DIRECTION ( 'NONE',  ( -0.5503133621338236470, 0.8349582046168341209, -0.000000000000000000 ) ) ;
#11478 = CARTESIAN_POINT ( 'NONE',  ( 40.05520465696179855, -7.028746455191999587, -16.50000000000000000 ) ) ;
#11479 = CARTESIAN_POINT ( 'NONE',  ( -4.390207617113899730, 7.856594496258241023, 21.50000000000000000 ) ) ;
#11480 = EDGE_CURVE ( 'NONE', #7845, #4361, #8136, .T. ) ;
#11481 = EDGE_CURVE ( 'NONE', #16205, #16378, #10621, .T. ) ;
#11482 = CARTESIAN_POINT ( 'NONE',  ( -15.49606647121365555, -7.052879176030717900, 19.96783386855779341 ) ) ;
#11483 = AXIS2_PLACEMENT_3D ( 'NONE', #9523, #16860, #5000 ) ;
#11484 = DIRECTION ( 'NONE',  ( 0.000000000000000000, 0.000000000000000000, 1.000000000000000000 ) ) ;
#11485 = ORIENTED_EDGE ( 'NONE', *, *, #21390, .F. ) ;
#11486 = ORIENTED_EDGE ( 'NONE', *, *, #18356, .T. ) ;
#11487 = CARTESIAN_POINT ( 'NONE',  ( 0.9307681286968548795, -9.436481611552755666, 13.00000000000000178 ) ) ;
#11488 = CARTESIAN_POINT ( 'NONE',  ( -7.677470532978346363, -15.25505107809155980, 6.521906765011493690 ) ) ;
#11489 = LINE ( 'NONE', #16315, #11420 ) ;
#11490 = ADVANCED_FACE ( 'NONE', ( #9956 ), #17120, .T. ) ;
#11491 = ORIENTED_EDGE ( 'NONE', *, *, #8476, .T. ) ;
#11492 = DIRECTION ( 'NONE',  ( 1.000000000000000000, 0.000000000000000000, 0.000000000000000000 ) ) ;
#11493 = CARTESIAN_POINT ( 'NONE',  ( 18.13085077595199834, -8.485104792618541225, 18.49267272388512140 ) ) ;
#11494 = CARTESIAN_POINT ( 'NONE',  ( 5.828790066614889298, 19.15065750257362609, 7.500898271101006820 ) ) ;
#11495 = EDGE_CURVE ( 'NONE', #8162, #28813, #16818, .T. ) ;
#11496 = ADVANCED_FACE ( 'NONE', ( #28374 ), #15092, .T. ) ;
#11497 = VERTEX_POINT ( 'NONE', #13076 ) ;
#11498 = CARTESIAN_POINT ( 'NONE',  ( 6.187077094091595342, 11.47693674426096599, 1.500000000000001332 ) ) ;
#11499 = CARTESIAN_POINT ( 'NONE',  ( 11.75961732103506385, 12.37772240090666642, 6.131018562779544823 ) ) ;
#11500 = CARTESIAN_POINT ( 'NONE',  ( -20.27188091683318660, -38.18452458809359484, -16.50000000000000000 ) ) ;
#11501 = CARTESIAN_POINT ( 'NONE',  ( -0.5346017343310117687, 42.60462856552967281, 28.83069491023030295 ) ) ;
#11502 = ORIENTED_EDGE ( 'NONE', *, *, #30168, .T. ) ;
#11503 = DIRECTION ( 'NONE',  ( 0.000000000000000000, 0.000000000000000000, -1.000000000000000000 ) ) ;
#11504 = EDGE_CURVE ( 'NONE', #9025, #9060, #23706, .T. ) ;
#11505 = CARTESIAN_POINT ( 'NONE',  ( 0.000000000000000000, 1.699320956058915452E-16, -1.500000000000001776 ) ) ;
#11506 = VECTOR ( 'NONE', #14632, 1000.000000000000000 ) ;
#11507 = CARTESIAN_POINT ( 'NONE',  ( -15.26094448139683202, 12.92753815214665103, 5.651480102388686255 ) ) ;
#11508 = ORIENTED_EDGE ( 'NONE', *, *, #21388, .T. ) ;
#11509 =( BOUNDED_CURVE ( )  B_SPLINE_CURVE ( 3, ( #24586, #3228, #12751, #4150 ),
 .UNSPECIFIED., .F., .T. ) 
 B_SPLINE_CURVE_WITH_KNOTS ( ( 4, 4 ),
 ( 0.5278016404580625487, 2.613791013131731233 ),
 .UNSPECIFIED. ) 
 CURVE ( )  GEOMETRIC_REPRESENTATION_ITEM ( )  RATIONAL_B_SPLINE_CURVE ( ( 1.000000000000000000, 0.6690902406732673890, 0.6690902406732673890, 1.000000000000000000 ) ) 
 REPRESENTATION_ITEM ( '' )  );
#11510 = CARTESIAN_POINT ( 'NONE',  ( 0.000000000000000000, 42.50000000000000000, 1.500000000000000000 ) ) ;
#11511 = CIRCLE ( 'NONE', #8537, 0.7500000000000006661 ) ;
#11512 = FACE_OUTER_BOUND ( 'NONE', #15856, .T. ) ;
#11513 = CARTESIAN_POINT ( 'NONE',  ( 12.20512804738064716, -42.03592599325837398, -16.50000000000000355 ) ) ;
#11514 = CARTESIAN_POINT ( 'NONE',  ( 0.5496282100021196992, -17.03044801512709938, 7.632642797338977658 ) ) ;
#11515 = CARTESIAN_POINT ( 'NONE',  ( 25.07174449839132180, -6.739288358966156522, 49.03857552305933609 ) ) ;
#11516 = LINE ( 'NONE', #28503, #21987 ) ;
#11517 = DIRECTION ( 'NONE',  ( -0.000000000000000000, 1.000000000000000000, -0.000000000000000000 ) ) ;
#11518 = CARTESIAN_POINT ( 'NONE',  ( 0.000000000000000000, 0.000000000000000000, -87.50000000000000000 ) ) ;
#11519 = VERTEX_POINT ( 'NONE', #12757 ) ;
#11520 = EDGE_CURVE ( 'NONE', #30839, #24164, #896, .T. ) ;
#11521 = EDGE_CURVE ( 'NONE', #17261, #7784, #20226, .T. ) ;
#11522 = CARTESIAN_POINT ( 'NONE',  ( -6.481689221553158298, 15.79948487157344772, 6.917457548096559883 ) ) ;
#11523 = CARTESIAN_POINT ( 'NONE',  ( -29.61203839202723032, -15.40012917324033381, -16.55003854064094426 ) ) ;
#11524 = EDGE_LOOP ( 'NONE', ( #28294, #1059, #8355, #3087 ) ) ;
#11525 = ADVANCED_FACE ( 'NONE', ( #8085 ), #731, .F. ) ;
#11526 = ORIENTED_EDGE ( 'NONE', *, *, #7930, .T. ) ;
#11527 = CARTESIAN_POINT ( 'NONE',  ( 4.437794406404234060, 19.50150518896417751, 19.85730954408918336 ) ) ;
#11528 = DIRECTION ( 'NONE',  ( 0.000000000000000000, 0.000000000000000000, -1.000000000000000000 ) ) ;
#11529 = EDGE_LOOP ( 'NONE', ( #16900, #6462, #22742, #18849 ) ) ;
#11530 = CIRCLE ( 'NONE', #2549, 7.500000000000000000 ) ;
#11531 = LINE ( 'NONE', #9177, #8706 ) ;
#11532 = SURFACE_STYLE_FILL_AREA ( #6831 ) ;
#11533 = ORIENTED_EDGE ( 'NONE', *, *, #23307, .T. ) ;
#11534 = CARTESIAN_POINT ( 'NONE',  ( -15.89797731339009523, 12.13494807016274635, 18.84486140012300837 ) ) ;
#11535 = CARTESIAN_POINT ( 'NONE',  ( -39.52380524536136619, -7.028748154183637631, -1.499999999999999556 ) ) ;
#11536 = ORIENTED_EDGE ( 'NONE', *, *, #4028, .T. ) ;
#11537 = ORIENTED_EDGE ( 'NONE', *, *, #19501, .F. ) ;
#11538 = CARTESIAN_POINT ( 'NONE',  ( 4.510281037539698445E-13, -4.926614671774132148E-13, 79.49999999999998579 ) ) ;
#11539 = AXIS2_PLACEMENT_3D ( 'NONE', #30667, #4490, #2607 ) ;
#11540 = ORIENTED_EDGE ( 'NONE', *, *, #12204, .F. ) ;
#11541 = EDGE_LOOP ( 'NONE', ( #25589, #1082, #15476, #1380 ) ) ;
#11542 = ADVANCED_FACE ( 'NONE', ( #24751 ), #5436, .T. ) ;
#11543 = FACE_OUTER_BOUND ( 'NONE', #1986, .T. ) ;
#11544 = DIRECTION ( 'NONE',  ( 1.000000000000000000, -2.890115478905172036E-15, 0.000000000000000000 ) ) ;
#11545 = EDGE_CURVE ( 'NONE', #26314, #29153, #1062, .T. ) ;
#11546 = DIRECTION ( 'NONE',  ( -0.000000000000000000, -0.000000000000000000, 1.000000000000000000 ) ) ;
#11547 = CARTESIAN_POINT ( 'NONE',  ( -15.16120755655624741, 17.22181377296911720, 1.500000000000000000 ) ) ;
#11548 = CARTESIAN_POINT ( 'NONE',  ( 16.87335920545513801, 2.247671665613721004, 19.00652017443069752 ) ) ;
#11549 = VERTEX_POINT ( 'NONE', #20082 ) ;
#11550 = CARTESIAN_POINT ( 'NONE',  ( 9.252152043196041120, -14.29436518012015256, 7.359006845440219102 ) ) ;
#11551 = CARTESIAN_POINT ( 'NONE',  ( 4.066382127562278015, -39.30923493945141445, 34.49999999999999289 ) ) ;
#11552 = CARTESIAN_POINT ( 'NONE',  ( -15.70110224921264930, 12.41706793386161323, 5.810767894563978686 ) ) ;
#11553 = CARTESIAN_POINT ( 'NONE',  ( 3.352743984114606057, 16.73528478182340962, 20.06253562465620632 ) ) ;
#11554 = VERTEX_POINT ( 'NONE', #26963 ) ;
#11555 = ORIENTED_EDGE ( 'NONE', *, *, #4774, .T. ) ;
#11556 = FACE_BOUND ( 'NONE', #23613, .T. ) ;
#11557 = CARTESIAN_POINT ( 'NONE',  ( 2.168404344971008868E-16, 42.50000000000000711, -1.500000000000000000 ) ) ;
#11558 = CARTESIAN_POINT ( 'NONE',  ( -5.031059497539946079, 16.27164807758199672, 18.49267272388512140 ) ) ;
#11559 = DIRECTION ( 'NONE',  ( 0.5406408174555974444, 0.8412535328311813165, 0.000000000000000000 ) ) ;
#11560 = CYLINDRICAL_SURFACE ( 'NONE', #20856, 0.7500000000000011102 ) ;
#11561 = LINE ( 'NONE', #6264, #20884 ) ;
#11562 = VERTEX_POINT ( 'NONE', #3553 ) ;
#11563 = VECTOR ( 'NONE', #23343, 1000.000000000000000 ) ;
#11564 = CARTESIAN_POINT ( 'NONE',  ( -17.06629068372215485, 0.6401188461407946173, 6.672349528511551497 ) ) ;
#11565 = CARTESIAN_POINT ( 'NONE',  ( -32.32717498572578307, -1.387778780781445676E-14, 1.500000000000000000 ) ) ;
#11566 = CARTESIAN_POINT ( 'NONE',  ( 0.000000000000000000, 0.000000000000000000, 85.49999999999998579 ) ) ;
#11567 = ORIENTED_EDGE ( 'NONE', *, *, #25434, .T. ) ;
#11568 = CARTESIAN_POINT ( 'NONE',  ( 18.65775367615955460, -7.252215724661030372, 6.041646659195333058 ) ) ;
#11569 = CARTESIAN_POINT ( 'NONE',  ( -5.221130439941095602, 43.71380105377362213, -16.49999999999999645 ) ) ;
#11570 = ORIENTED_EDGE ( 'NONE', *, *, #45, .T. ) ;
#11571 = CARTESIAN_POINT ( 'NONE',  ( 26.86404174848737725, -26.32179565544504030, 27.50000000000000711 ) ) ;
#11572 = CARTESIAN_POINT ( 'NONE',  ( -40.05104235265675783, -2.353288714454546238, -11.49999999999999645 ) ) ;
#11573 = CIRCLE ( 'NONE', #26514, 10.00000000000000178 ) ;
#11574 = DIRECTION ( 'NONE',  ( 0.000000000000000000, 0.000000000000000000, 1.000000000000000000 ) ) ;
#11575 = FACE_OUTER_BOUND ( 'NONE', #28317, .T. ) ;
#11576 = CARTESIAN_POINT ( 'NONE',  ( -6.393592071792286724, 18.96945647184856654, 20.25542030744407640 ) ) ;
#11577 = EDGE_CURVE ( 'NONE', #24166, #20151, #8396, .T. ) ;
#11578 = DIRECTION ( 'NONE',  ( -0.000000000000000000, 0.000000000000000000, 1.000000000000000000 ) ) ;
#11579 = DIRECTION ( 'NONE',  ( 0.9594929736144952592, -0.2817325568414371095, 0.000000000000000000 ) ) ;
#11580 = ORIENTED_EDGE ( 'NONE', *, *, #587, .T. ) ;
#11581 = CARTESIAN_POINT ( 'NONE',  ( 15.55762523212740689, -6.926306048626145184, 5.848946451764560628 ) ) ;
#11582 = DIRECTION ( 'NONE',  ( 1.000000000000000000, 0.000000000000000000, 0.000000000000000000 ) ) ;
#11583 = DIRECTION ( 'NONE',  ( 0.000000000000000000, 1.132880637372608986E-16, -1.000000000000000000 ) ) ;
#11584 = ORIENTED_EDGE ( 'NONE', *, *, #25747, .T. ) ;
#11585 = FACE_OUTER_BOUND ( 'NONE', #28013, .T. ) ;
#11586 = CARTESIAN_POINT ( 'NONE',  ( 11.11463800144301750, -16.64861661464430043, 7.652108011868850035 ) ) ;
#11587 = DIRECTION ( 'NONE',  ( 0.000000000000000000, 0.000000000000000000, -1.000000000000000000 ) ) ;
#11588 = ORIENTED_EDGE ( 'NONE', *, *, #807, .T. ) ;
#11589 = DIRECTION ( 'NONE',  ( 0.000000000000000000, 1.000000000000000000, 0.000000000000000000 ) ) ;
#11590 = AXIS2_PLACEMENT_3D ( 'NONE', #28903, #14550, #24047 ) ;
#11591 = CIRCLE ( 'NONE', #29025, 9.084132297865673777 ) ;
#11592 = DIRECTION ( 'NONE',  ( 0.000000000000000000, -1.132880637372608986E-16, 1.000000000000000000 ) ) ;
#11593 = CARTESIAN_POINT ( 'NONE',  ( 33.33631137181001236, -22.22424899003631182, 34.67383366597271532 ) ) ;
#11595 = VECTOR ( 'NONE', #10087, 1000.000000000000000 ) ;
#11594 = CARTESIAN_POINT ( 'NONE',  ( -6.222613296526849247, 19.00773140132665517, 7.626218077512939786 ) ) ;
#11596 = VERTEX_POINT ( 'NONE', #21415 ) ;
#11597 = DIRECTION ( 'NONE',  ( 0.000000000000000000, 1.000000000000000000, 1.193512090021232842E-16 ) ) ;
#11598 = CARTESIAN_POINT ( 'NONE',  ( 49.99999999999998579, 50.00000000000000000, 52.07879600563550326 ) ) ;
#11599 = FACE_BOUND ( 'NONE', #24599, .T. ) ;
#11600 = ORIENTED_EDGE ( 'NONE', *, *, #17933, .T. ) ;
#11601 = ORIENTED_EDGE ( 'NONE', *, *, #10589, .F. ) ;
#11602 = DIRECTION ( 'NONE',  ( -0.000000000000000000, -0.000000000000000000, 1.000000000000000000 ) ) ;
#11603 = CARTESIAN_POINT ( 'NONE',  ( -33.78553900464347493, 24.40792682089791654, -16.50000000000000000 ) ) ;
#11604 = VERTEX_POINT ( 'NONE', #30616 ) ;
#11605 = CYLINDRICAL_SURFACE ( 'NONE', #22341, 0.7500000000000006661 ) ;
#11606 = CARTESIAN_POINT ( 'NONE',  ( -10.39981488257415165, -17.10438141112844690, 7.643931100913408550 ) ) ;
#11607 = DIRECTION ( 'NONE',  ( 0.000000000000000000, 0.000000000000000000, 1.000000000000000000 ) ) ;
#11608 = CARTESIAN_POINT ( 'NONE',  ( 1.139261986572421614, -19.98520933375989728, 19.97651184436794125 ) ) ;
#11609 = ORIENTED_EDGE ( 'NONE', *, *, #20455, .T. ) ;
#11610 = LINE ( 'NONE', #28313, #29735 ) ;
#11611 = VECTOR ( 'NONE', #19619, 1000.000000000000000 ) ;
#11612 = ADVANCED_FACE ( 'NONE', ( #22876 ), #13538, .F. ) ;
#11613 = DIRECTION ( 'NONE',  ( 0.000000000000000000, 0.000000000000000000, 1.000000000000000000 ) ) ;
#11614 = CARTESIAN_POINT ( 'NONE',  ( 1.112485354161228759E-15, -9.084132297865675554, 21.50000000000000355 ) ) ;
#11615 = CARTESIAN_POINT ( 'NONE',  ( 28.78283879316666471, 7.125616703334846314, 41.10667063058291149 ) ) ;
#11616 = EDGE_LOOP ( 'NONE', ( #3784, #6762, #22195, #23507 ) ) ;
#11617 = EDGE_CURVE ( 'NONE', #14972, #18098, #20536, .T. ) ;
#11618 = AXIS2_PLACEMENT_3D ( 'NONE', #27057, #12407, #21904 ) ;
#11619 = FACE_OUTER_BOUND ( 'NONE', #12958, .T. ) ;
#11620 = CARTESIAN_POINT ( 'NONE',  ( -15.27764744541513053, -7.543477926929822885, 20.32222155561918697 ) ) ;
#11621 = CARTESIAN_POINT ( 'NONE',  ( -12.79952941388599896, 11.22436372989799125, 18.83976166372256245 ) ) ;
#11622 = CARTESIAN_POINT ( 'NONE',  ( -25.64627119138473432, -23.40052582045089480, -6.500000000000000888 ) ) ;
#11623 = CARTESIAN_POINT ( 'NONE',  ( 18.25545825136821421, 37.59715331615011991, 23.77245749941748798 ) ) ;
#11624 = CARTESIAN_POINT ( 'NONE',  ( -18.37606348208443308, -7.894877446839454471, 18.72886616302736229 ) ) ;
#11625 = CARTESIAN_POINT ( 'NONE',  ( -15.57452153527462535, -6.867569271111570117, 19.22654678686458141 ) ) ;
#11626 = DIRECTION ( 'NONE',  ( 0.000000000000000000, 0.000000000000000000, -1.000000000000000000 ) ) ;
#11627 = ORIENTED_EDGE ( 'NONE', *, *, #14133, .F. ) ;
#11628 = ORIENTED_EDGE ( 'NONE', *, *, #18135, .F. ) ;
#11629 = DIRECTION ( 'NONE',  ( 1.000000000000000000, 0.000000000000000000, 0.000000000000000000 ) ) ;
#11630 = CARTESIAN_POINT ( 'NONE',  ( -20.65888525914099105, 38.75220717792564784, -19.50000000000000355 ) ) ;
#11631 = DIRECTION ( 'NONE',  ( -0.000000000000000000, -0.000000000000000000, -1.000000000000000000 ) ) ;
#11632 = ORIENTED_EDGE ( 'NONE', *, *, #22202, .F. ) ;
#11633 = CARTESIAN_POINT ( 'NONE',  ( 15.71976421978570748, -6.574744378264570699, 20.32842677360128292 ) ) ;
#11634 = CARTESIAN_POINT ( 'NONE',  ( 4.874170568648002799, 16.31160065975152307, 7.176035686813569292 ) ) ;
#11635 = VECTOR ( 'NONE', #11101, 1000.000000000000000 ) ;
#11636 = EDGE_LOOP ( 'NONE', ( #6577, #25246, #7102, #17987, #14295, #9520, #23695, #22183, #11632, #21537, #18251, #14921, #24602, #3262, #30238, #25832, #12078, #18611, #19345, #29958, #5732, #26137, #21633, #11115, #8788, #12048, #4498, #16155, #15538, #24092, #10557, #16078, #23549, #9093, #2596, #493, #14230, #22163, #6804, #24677, #22596, #19795, #2717, #24845, #2168, #14726, #27250, #1793, #15306, #27752, #11190, #17797, #20060, #12468, #29, #22343, #11502, #8140, #4892, #26663, #27875, #5661, #29604, #4736, #3120, #14148, #9566, #7110, #15980, #29119, #21389, #10796, #3137, #6508, #4004, #29904, #7003 ) ) ;
#11637 = AXIS2_PLACEMENT_3D ( 'NONE', #22334, #29515, #3776 ) ;
#11638 = CARTESIAN_POINT ( 'NONE',  ( -32.82330813384598400, -22.94799032726886523, -1.500000000000000000 ) ) ;
#11639 = EDGE_CURVE ( 'NONE', #29565, #23323, #23194, .T. ) ;
#11640 = CARTESIAN_POINT ( 'NONE',  ( 0.000000000000000000, 0.000000000000000000, 0.000000000000000000 ) ) ;
#11641 = CARTESIAN_POINT ( 'NONE',  ( -35.21927848278606632, 18.30290806334510023, 31.24093525326876275 ) ) ;
#11642 = VERTEX_POINT ( 'NONE', #20394 ) ;
#11643 = LINE ( 'NONE', #18667, #27293 ) ;
#11644 = EDGE_CURVE ( 'NONE', #8908, #23909, #22715, .T. ) ;
#11645 = EDGE_CURVE ( 'NONE', #17647, #10553, #25218, .T. ) ;
#11646 = DIRECTION ( 'NONE',  ( 0.000000000000000000, 0.000000000000000000, -1.000000000000000000 ) ) ;
#11647 = CARTESIAN_POINT ( 'NONE',  ( -14.67655575066034856, 13.58671083542087921, 6.518927109361836614 ) ) ;
#11648 = ORIENTED_EDGE ( 'NONE', *, *, #18891, .T. ) ;
#11649 = CARTESIAN_POINT ( 'NONE',  ( -40.05520497409654013, 7.028746409781321702, -16.50000000000000000 ) ) ;
#11650 = CARTESIAN_POINT ( 'NONE',  ( 12.72536390617885438, -2.839914339433650348, 1.500000000000001332 ) ) ;
#11651 = EDGE_CURVE ( 'NONE', #29372, #25287, #30681, .T. ) ;
#11652 = CARTESIAN_POINT ( 'NONE',  ( 2.095349214508610114, -44.03244755841715374, -16.50000000000000355 ) ) ;
#11653 = PRODUCT_DEFINITION_SHAPE ( 'NONE', 'NONE',  #22874 ) ;
#11654 = CARTESIAN_POINT ( 'NONE',  ( -0.3742200966386526884, -20.01457288233325471, 7.359006845440219102 ) ) ;
#11655 = DIRECTION ( 'NONE',  ( 0.000000000000000000, 1.000000000000000000, 0.000000000000000000 ) ) ;
#11656 = DIRECTION ( 'NONE',  ( -1.000000000000000000, 0.000000000000000000, 0.000000000000000000 ) ) ;
#11657 = CIRCLE ( 'NONE', #15639, 7.500000000000013323 ) ;
#11658 = CARTESIAN_POINT ( 'NONE',  ( -17.02496544227784270, 1.117683430491693386, 20.19593175699879595 ) ) ;
#11659 = CARTESIAN_POINT ( 'NONE',  ( -3.196529495465446402, -8.413215745754985875, 21.50000000000000000 ) ) ;
#11660 = VERTEX_POINT ( 'NONE', #8552 ) ;
#11661 = EDGE_CURVE ( 'NONE', #6974, #24290, #4795, .T. ) ;
#11662 = CARTESIAN_POINT ( 'NONE',  ( -37.99999999999999289, 209.2686044187655909, -75.50000000000000000 ) ) ;
#11663 = CARTESIAN_POINT ( 'NONE',  ( -0.1262659238204836554, -8.999114229549588728, 21.50000000000000000 ) ) ;
#11664 = EDGE_CURVE ( 'NONE', #9274, #7713, #20255, .T. ) ;
#11665 = ORIENTED_EDGE ( 'NONE', *, *, #5417, .F. ) ;
#11666 = ORIENTED_EDGE ( 'NONE', *, *, #7461, .F. ) ;
#11667 = EDGE_CURVE ( 'NONE', #11816, #11851, #25219, .T. ) ;
#11668 = CARTESIAN_POINT ( 'NONE',  ( -50.00000000000000711, 70.00000000000001421, 53.15210795805025867 ) ) ;
#11669 = DIRECTION ( 'NONE',  ( 0.000000000000000000, 0.000000000000000000, -1.000000000000000000 ) ) ;
#11670 = ORIENTED_EDGE ( 'NONE', *, *, #9581, .T. ) ;
#11671 = DIRECTION ( 'NONE',  ( 1.000000000000000000, 0.000000000000000000, 0.000000000000000000 ) ) ;
#11672 = CARTESIAN_POINT ( 'NONE',  ( -20.71335220384823117, 27.86167394782616213, -16.50001200000000168 ) ) ;
#11673 = ORIENTED_EDGE ( 'NONE', *, *, #17821, .T. ) ;
#11674 = CARTESIAN_POINT ( 'NONE',  ( 8.430595340551260364, -4.340342926364983533, 13.00000000000000178 ) ) ;
#11675 = CARTESIAN_POINT ( 'NONE',  ( -7.028330626922778990, 10.93629592680536788, 24.50000000000000000 ) ) ;
#11676 = ORIENTED_EDGE ( 'NONE', *, *, #27685, .F. ) ;
#11677 = AXIS2_PLACEMENT_3D ( 'NONE', #17774, #22291, #3583 ) ;
#11678 = ADVANCED_FACE ( 'NONE', ( #6926 ), #14231, .T. ) ;
#11679 = ORIENTED_EDGE ( 'NONE', *, *, #25937, .F. ) ;
#11680 = DIRECTION ( 'NONE',  ( 0.000000000000000000, -0.000000000000000000, 1.000000000000000000 ) ) ;
#11681 = EDGE_CURVE ( 'NONE', #11902, #5590, #29204, .T. ) ;
#11682 = ORIENTED_EDGE ( 'NONE', *, *, #9974, .F. ) ;
#11683 = EDGE_CURVE ( 'NONE', #21119, #24968, #11767, .T. ) ;
#11684 = VERTEX_POINT ( 'NONE', #18055 ) ;
#11685 = B_SPLINE_CURVE_WITH_KNOTS ( 'NONE', 3,
 ( #20083, #10251, #732, #29452, #22104, #3398, #17592, #12759, #19614, #15080, #12927, #17737, #7616, #7937 ),
 .UNSPECIFIED., .F., .F.,
 ( 4, 2, 1, 1, 2, 2, 2, 4 ),
 ( 0.7234904873890852794, 0.7367515904914523350, 0.7433821420426358628, 0.7466974178182276267, 0.7483550557060234532, 0.7500126935938193906, 0.7632737966961864462, 0.7765348997985535018 ),
 .UNSPECIFIED. ) ;
#11686 = ADVANCED_FACE ( 'NONE', ( #4889 ), #11754, .F. ) ;
#11687 = CYLINDRICAL_SURFACE ( 'NONE', #15577, 1.447898107987198646 ) ;
#11688 = CARTESIAN_POINT ( 'NONE',  ( -0.2301049870085050963, -17.01973991014545007, 19.21496526180055398 ) ) ;
#11689 = CARTESIAN_POINT ( 'NONE',  ( -5.127072262013854242, -42.13114360820154047, 28.87158698979397897 ) ) ;
#11690 = CARTESIAN_POINT ( 'NONE',  ( 1.795304038745377362, -16.98367057141059888, 19.47952243369110548 ) ) ;
#11691 = CARTESIAN_POINT ( 'NONE',  ( 19.89137488457043901, 2.247671665613721004, 19.00652017443069752 ) ) ;
#11692 = ORIENTED_EDGE ( 'NONE', *, *, #17924, .T. ) ;
#11693 = EDGE_CURVE ( 'NONE', #28858, #154, #9425, .T. ) ;
#11694 = DIRECTION ( 'NONE',  ( 0.9329908884337534403, 0.3598999890241668664, 0.000000000000000000 ) ) ;
#11695 = CARTESIAN_POINT ( 'NONE',  ( -0.6883321258581104329, 8.884323311075791096, -1.500000000000000888 ) ) ;
#11696 = CARTESIAN_POINT ( 'NONE',  ( -15.45023549775889116, 12.72816703665372096, 7.643931100913408550 ) ) ;
#11697 = DIRECTION ( 'NONE',  ( 1.000000000000000000, 0.000000000000000000, 0.000000000000000000 ) ) ;
#11698 = ORIENTED_EDGE ( 'NONE', *, *, #983, .F. ) ;
#11699 = ORIENTED_EDGE ( 'NONE', *, *, #25240, .F. ) ;
#11700 = CIRCLE ( 'NONE', #7729, 0.7500000000000006661 ) ;
#11701 = CARTESIAN_POINT ( 'NONE',  ( 30.75232512042845556, -9.966982604840845639, 1.500000000000000000 ) ) ;
#11702 = CARTESIAN_POINT ( 'NONE',  ( -23.96732207939035675, 33.98584080153585774, -1.500000000000009992 ) ) ;
#11703 = CARTESIAN_POINT ( 'NONE',  ( 15.45664188325222455, 12.69231265181875834, 19.85261563089510517 ) ) ;
#11704 = CARTESIAN_POINT ( 'NONE',  ( -5.549074438707200407, 16.11683645443577362, 18.34798005862930381 ) ) ;
#11705 = PLANE ( 'NONE',  #1184 ) ;
#11706 = CARTESIAN_POINT ( 'NONE',  ( 0.000000000000000000, 39.50000000000000000, 27.50000000000000355 ) ) ;
#11707 = DIRECTION ( 'NONE',  ( 0.000000000000000000, 0.000000000000000000, -1.000000000000000000 ) ) ;
#11708 = EDGE_CURVE ( 'NONE', #26722, #23884, #26573, .T. ) ;
#11709 = VERTEX_POINT ( 'NONE', #5351 ) ;
#11710 = EDGE_CURVE ( 'NONE', #10221, #6658, #12379, .T. ) ;
#11711 = CARTESIAN_POINT ( 'NONE',  ( -19.89984252009588062, 2.172142757504855304, 7.603368798681074736 ) ) ;
#11712 = CARTESIAN_POINT ( 'NONE',  ( 49.99999999999998579, -50.00000000000000000, 97.07879600563551037 ) ) ;
#11713 = DIRECTION ( 'NONE',  ( 0.000000000000000000, 0.000000000000000000, -1.000000000000000000 ) ) ;
#11714 = EDGE_LOOP ( 'NONE', ( #2613, #8184, #25914, #20103 ) ) ;
#11715 = DIRECTION ( 'NONE',  ( -0.000000000000000000, -0.000000000000000000, 1.000000000000000000 ) ) ;
#11716 = VERTEX_POINT ( 'NONE', #21882 ) ;
#11717 = DIRECTION ( 'NONE',  ( 1.000000000000000000, 0.000000000000000000, 0.000000000000000000 ) ) ;
#11718 = LINE ( 'NONE', #23707, #5064 ) ;
#11719 = EDGE_LOOP ( 'NONE', ( #24205, #8225, #21370, #9396 ) ) ;
#11720 = CARTESIAN_POINT ( 'NONE',  ( 35.99942728066312725, 0.6588716437970913997, 27.50000000000001066 ) ) ;
#11721 = AXIS2_PLACEMENT_3D ( 'NONE', #9995, #19500, #4305 ) ;
#11722 = DIRECTION ( 'NONE',  ( 0.000000000000000000, 0.000000000000000000, 1.000000000000000000 ) ) ;
#11723 = CARTESIAN_POINT ( 'NONE',  ( 9.864937699929956949, -13.90063973435163724, 18.34798005863078885 ) ) ;
#11724 = DIRECTION ( 'NONE',  ( 1.000000000000000000, 0.000000000000000000, 0.000000000000000000 ) ) ;
#11725 = CARTESIAN_POINT ( 'NONE',  ( -5.964083977939224290, 15.98216206238707926, 20.25542030744407640 ) ) ;
#11726 = LINE ( 'NONE', #30748, #5859 ) ;
#11727 = DIRECTION ( 'NONE',  ( -0.000000000000000000, -0.000000000000000000, -1.000000000000000000 ) ) ;
#11728 = CARTESIAN_POINT ( 'NONE',  ( 1.000000000000008438, 17.23749217771910480, -0.6213203435596476032 ) ) ;
#11729 = ORIENTED_EDGE ( 'NONE', *, *, #9965, .T. ) ;
#11730 = CARTESIAN_POINT ( 'NONE',  ( 23.17581250239729940, 34.50630206824671120, -1.499999999999999778 ) ) ;
#11731 = CARTESIAN_POINT ( 'NONE',  ( -12.56641067637617759, -40.32935944494947478, -1.500000000000000000 ) ) ;
#11732 = AXIS2_PLACEMENT_3D ( 'NONE', #3939, #18274, #27797 ) ;
#11733 = LINE ( 'NONE', #9858, #30240 ) ;
#11734 = ORIENTED_EDGE ( 'NONE', *, *, #5236, .T. ) ;
#11735 = FACE_OUTER_BOUND ( 'NONE', #14334, .T. ) ;
#11736 = CARTESIAN_POINT ( 'NONE',  ( -17.82234029294485467, -9.114408740892777416, 20.19593175699879595 ) ) ;
#11737 = CARTESIAN_POINT ( 'NONE',  ( 19.74328841314636307, 3.194145055459935101, 7.652108011868850035 ) ) ;
#11738 = PRESENTATION_STYLE_ASSIGNMENT (( #8785 ) ) ;
#11739 = CARTESIAN_POINT ( 'NONE',  ( 5.374868878254059013, -44.10336124695543703, -19.50000000000000355 ) ) ;
#11740 = ORIENTED_EDGE ( 'NONE', *, *, #1567, .T. ) ;
#11741 = CARTESIAN_POINT ( 'NONE',  ( -24.03057240117691862, 26.57182937991348481, -6.499999999999999112 ) ) ;
#11742 = VECTOR ( 'NONE', #7208, 1000.000000000000000 ) ;
#11743 = CARTESIAN_POINT ( 'NONE',  ( -31.18700685316050780, 26.11823559932051353, -1.500000000000000000 ) ) ;
#11744 = CARTESIAN_POINT ( 'NONE',  ( 30.38390623893337761, 22.11697395215319162, 37.50000000001698197 ) ) ;
#11745 = CARTESIAN_POINT ( 'NONE',  ( -6.934930584103121909, 18.75917743548997763, 6.523620417364445423 ) ) ;
#11746 = ORIENTED_EDGE ( 'NONE', *, *, #17988, .T. ) ;
#11747 = VECTOR ( 'NONE', #24969, 1000.000000000000000 ) ;
#11748 = DIRECTION ( 'NONE',  ( 0.000000000000000000, 0.000000000000000000, 1.000000000000000000 ) ) ;
#11749 = CARTESIAN_POINT ( 'NONE',  ( -39.00000000000000000, 5.563236990218665134, -1.500000000000000000 ) ) ;
#11750 = DIRECTION ( 'NONE',  ( -0.000000000000000000, -0.000000000000000000, -1.000000000000000000 ) ) ;
#11751 = EDGE_CURVE ( 'NONE', #15107, #15261, #11288, .T. ) ;
#11752 = ORIENTED_EDGE ( 'NONE', *, *, #10026, .T. ) ;
#11753 = ORIENTED_EDGE ( 'NONE', *, *, #23330, .T. ) ;
#11754 = CYLINDRICAL_SURFACE ( 'NONE', #9792, 0.7499999999999997780 ) ;
#11755 = ORIENTED_EDGE ( 'NONE', *, *, #21277, .F. ) ;
#11756 = CARTESIAN_POINT ( 'NONE',  ( 0.01636335959932410516, -20.01808238691632624, 18.39701043959520987 ) ) ;
#11757 = CARTESIAN_POINT ( 'NONE',  ( -8.487288213245035351, -14.78455279991285920, 7.652108011868850035 ) ) ;
#11758 = DIRECTION ( 'NONE',  ( 0.000000000000000000, 0.000000000000000000, 1.000000000000000000 ) ) ;
#11759 = CARTESIAN_POINT ( 'NONE',  ( 1.497940275966472390, -17.00196529467651985, 20.06253562465620632 ) ) ;
#11760 = ORIENTED_EDGE ( 'NONE', *, *, #25744, .F. ) ;
#11761 = CARTESIAN_POINT ( 'NONE',  ( 9.033033306777456417, -0.9621688436939737077, 21.50000000000000000 ) ) ;
#11762 = AXIS2_PLACEMENT_3D ( 'NONE', #604, #9981, #19786 ) ;
#11763 = CARTESIAN_POINT ( 'NONE',  ( 29.61203839202722676, 15.40012917324034092, 41.62281023987512185 ) ) ;
#11764 = CARTESIAN_POINT ( 'NONE',  ( 14.79201625507351991, 13.48748956535167665, 18.35718225375110180 ) ) ;
#11765 = CARTESIAN_POINT ( 'NONE',  ( -5.524309650260710747, 7.706848733601013635, 21.50000000000000000 ) ) ;
#11766 = ORIENTED_EDGE ( 'NONE', *, *, #25026, .T. ) ;
#11767 = CIRCLE ( 'NONE', #23218, 0.7499999999999988898 ) ;
#11768 = CARTESIAN_POINT ( 'NONE',  ( 0.000000000000000000, -2.435693370351110282E-15, 21.50000000000000355 ) ) ;
#11769 = CARTESIAN_POINT ( 'NONE',  ( -12.71197447203568132, 11.31946111510424302, 19.21496526180054332 ) ) ;
#11770 = CARTESIAN_POINT ( 'NONE',  ( -2.081668171172168513E-14, 90.00000000000001421, 37.49999999999999289 ) ) ;
#11771 = CARTESIAN_POINT ( 'NONE',  ( -19.94482228061659512, 1.484609193405912464, 6.523620417364436541 ) ) ;
#11772 = CARTESIAN_POINT ( 'NONE',  ( 8.268028093133368728, 3.763133143576462114, -1.500000000000001332 ) ) ;
#11773 = CARTESIAN_POINT ( 'NONE',  ( -15.43012792948217182, -7.204331193346493301, 20.12545155307891065 ) ) ;
#11774 = CARTESIAN_POINT ( 'NONE',  ( 33.03549465208794800, -8.974030344605379739, 36.52487348530875266 ) ) ;
#11775 = AXIS2_PLACEMENT_3D ( 'NONE', #8413, #16646, #4489 ) ;
#11776 = ORIENTED_EDGE ( 'NONE', *, *, #16255, .F. ) ;
#11777 = ORIENTED_EDGE ( 'NONE', *, *, #14308, .F. ) ;
#11778 = DIRECTION ( 'NONE',  ( -0.000000000000000000, -0.000000000000000000, 1.000000000000000000 ) ) ;
#11779 = CARTESIAN_POINT ( 'NONE',  ( 2.552544030762014415, -42.50000000000000000, -1.500000000000000000 ) ) ;
#11780 = DIRECTION ( 'NONE',  ( 0.9096319953545183301, 0.4154150130018865461, 0.000000000000000000 ) ) ;
#11781 = DIRECTION ( 'NONE',  ( -1.000000000000000000, 0.000000000000000000, 0.000000000000000000 ) ) ;
#11782 = EDGE_LOOP ( 'NONE', ( #21921, #23222, #676, #4352 ) ) ;
#11783 = DIRECTION ( 'NONE',  ( 1.000000000000000000, 0.000000000000000000, 0.000000000000000000 ) ) ;
#11784 = CARTESIAN_POINT ( 'NONE',  ( 15.39622458953737372, -7.259188434806183921, 19.56050940960062690 ) ) ;
#11785 = CARTESIAN_POINT ( 'NONE',  ( 4.564720541824407007, 16.40857754966928894, 5.796888747622817029 ) ) ;
#11786 = VECTOR ( 'NONE', #1046, 1000.000000000000000 ) ;
#11787 = ORIENTED_EDGE ( 'NONE', *, *, #13724, .F. ) ;
#11788 = CARTESIAN_POINT ( 'NONE',  ( 4.049916830765389442, 16.55712665160098851, 20.34789198813115263 ) ) ;
#11789 = VECTOR ( 'NONE', #20201, 1000.000000000000000 ) ;
#11790 = DIRECTION ( 'NONE',  ( -0.000000000000000000, -0.000000000000000000, 1.000000000000000000 ) ) ;
#11791 = DIRECTION ( 'NONE',  ( 0.000000000000000000, 0.000000000000000000, -1.000000000000000000 ) ) ;
#11792 = CARTESIAN_POINT ( 'NONE',  ( -25.91933551046517081, 31.76379658186127841, 29.86662960453368143 ) ) ;
#11793 = ORIENTED_EDGE ( 'NONE', *, *, #28430, .T. ) ;
#11794 = DIRECTION ( 'NONE',  ( -0.6548607339452851006, -0.7557495743542582689, 0.000000000000000000 ) ) ;
#11795 = CARTESIAN_POINT ( 'NONE',  ( 3.683253992019827727, -8.303920738747228469, 13.22130136205108641 ) ) ;
#11796 = B_SPLINE_CURVE_WITH_KNOTS ( 'NONE', 3,
 ( #20537, #6355, #15868, #25385, #13540, #29751, #23020, #8851, #21131, #25683, #6802, #7265, #30817, #9149, #23626, #13839, #16326, #4477, #9298, #26294, #23947, #4307, #21610, #11500, #6652, #2270, #2594, #12112, #18664 ),
 .UNSPECIFIED., .F., .F.,
 ( 4, 1, 2, 2, 2, 2, 2, 2, 1, 2, 2, 1, 2, 2, 2, 4 ),
 ( 0.000000000000000000, 0.01176252312833788068, 0.01470315391042235215, 0.01764378469250681841, 0.02352504625667574054, 0.03528756938501358825, 0.04116883094918252078, 0.04705009251335146025, 0.05881261564168926981, 0.06175324642377374995, 0.06469387720585821622, 0.07057513877002716263, 0.07645640033419609516, 0.08233766189836502769, 0.08821892346253397410, 0.09410018502670292051 ),
 .UNSPECIFIED. ) ;
#11797 = CARTESIAN_POINT ( 'NONE',  ( -14.81512577538153153, 13.43580467474268758, 6.033082186765052590 ) ) ;
#11798 = CIRCLE ( 'NONE', #1832, 9.084132297865673777 ) ;
#11799 = ORIENTED_EDGE ( 'NONE', *, *, #7531, .T. ) ;
#11800 = CARTESIAN_POINT ( 'NONE',  ( -18.47028637364415360, -7.717842544976232233, 6.530762810602277924 ) ) ;
#11801 = AXIS2_PLACEMENT_3D ( 'NONE', #8529, #15526, #24896 ) ;
#11802 = FACE_OUTER_BOUND ( 'NONE', #9587, .T. ) ;
#11803 = CARTESIAN_POINT ( 'NONE',  ( 14.27661992934221402, 14.00645734016344157, 7.161525567826881655 ) ) ;
#11804 = DIRECTION ( 'NONE',  ( 1.000000000000000000, 0.000000000000000000, -0.000000000000000000 ) ) ;
#11805 = CIRCLE ( 'NONE', #23746, 9.482273699623480212 ) ;
#11806 = DIRECTION ( 'NONE',  ( -0.000000000000000000, -0.000000000000000000, 1.000000000000000000 ) ) ;
#11807 = AXIS2_PLACEMENT_3D ( 'NONE', #22397, #22235, #13048 ) ;
#11808 = PLANE ( 'NONE',  #6052 ) ;
#11809 = CARTESIAN_POINT ( 'NONE',  ( -19.87001189204712759, 2.428856360474549003, 20.34789198813115263 ) ) ;
#11810 = CARTESIAN_POINT ( 'NONE',  ( -64.99999999999998579, 36.86186943028246787, 97.07879600563551037 ) ) ;
#11811 = ORIENTED_EDGE ( 'NONE', *, *, #21993, .F. ) ;
#11812 = CARTESIAN_POINT ( 'NONE',  ( 11.76322808224952610, -16.19669642467958326, 19.97651184436794125 ) ) ;
#11813 = CIRCLE ( 'NONE', #29255, 20.00000000000000000 ) ;
#11814 = LINE ( 'NONE', #114, #15058 ) ;
#11815 = EDGE_LOOP ( 'NONE', ( #3809, #24646, #19761, #22558 ) ) ;
#11816 = VERTEX_POINT ( 'NONE', #19543 ) ;
#11817 = CARTESIAN_POINT ( 'NONE',  ( -15.73346977245381240, 12.34774510571039130, 7.454606537396343491 ) ) ;
#11818 = CIRCLE ( 'NONE', #15804, 0.7500000000000006661 ) ;
#11819 = PRODUCT_RELATED_PRODUCT_CATEGORY ( 'part', '', ( #5199 ) ) ;
#11820 = LINE ( 'NONE', #30679, #23808 ) ;
#11821 = VECTOR ( 'NONE', #17019, 1000.000000000000000 ) ;
#11822 = ORIENTED_EDGE ( 'NONE', *, *, #11545, .T. ) ;
#11823 = AXIS2_PLACEMENT_3D ( 'NONE', #9403, #28893, #26549 ) ;
#11824 = EDGE_CURVE ( 'NONE', #27003, #14619, #2703, .T. ) ;
#11825 = CARTESIAN_POINT ( 'NONE',  ( 15.25711736267466634, 12.95927645368826653, 20.19668224736330941 ) ) ;
#11826 = PRESENTATION_STYLE_ASSIGNMENT (( #16358 ) ) ;
#11827 = CLOSED_SHELL ( 'NONE', ( #14809, #5735, #11612, #10528, #3833, #28222, #23864, #9567, #25661, #27330, #23649, #11091, #10306, #23428, #18585, #17573, #16090, #20848, #22882, #20434, #30714, #28064, #21959, #29797, #2342, #13762, #20484, #15901, #397, #11062, #30476, #1165, #24220, #13439, #9940, #25912, #28067, #24983, #22588, #9753, #17524, #18028, #18542, #7651, #27128, #10169, #13069, #8078, #13107, #30554, #16827, #11862, #12093, #1402, #17975, #23500, #7855, #16233, #13832, #28621, #21281, #16333, #24647, #21669, #1355, #13602, #12852, #27333, #14102, #7463, #13216, #586, #29113, #8054, #30004, #29829, #22703, #2339, #4043, #2954, #5403, #1822, #14531, #12037, #9790, #20045, #5273, #4427, #5516, #2314, #16824, #5061, #29115, #7504, #8815, #7319, #20744, #1900, #6013, #14287, #17798, #7684, #6931, #26513, #20955, #29441, #632, #22695, #15333, #28589, #22889, #16215, #23462, #13242, #10198, #15494, #11496, #25175, #1491, #10163, #30515, #25013, #19512, #28450, #7002, #3377, #12542, #4820, #21162, #20388, #22923, #9020, #3446, #3549, #25597, #9810, #26404, #17793, #8238, #5549, #20314, #11102, #11865, #28466, #1374, #16991, #18587, #18545, #6138, #12086, #30305, #4271, #15151, #26298, #9721, #3457, #9743, #8996, #28815, #3896, #16436, #21323, #25605, #21853, #6619, #1204, #25030, #22498, #16651, #20418, #19435, #17002, #15511, #1198, #19833, #21212, #13017, #19900, #14722, #30726, #19462, #3670, #595, #1055, #3676, #24432, #19897, #4990, #13358, #22364, #28838, #12315, #4784, #1020, #16989, #7647, #13929, #29940, #2754, #23463, #19236, #4838, #21539, #5169, #17237, #28283, #1769, #6886, #23646, #5700, #4530, #27541, #13916, #2906, #23925, #29421, #23665, #8278, #17950, #951, #5426, #12538, #12215, #7072, #5747, #17410, #7068, #13237, #21937, #23696, #198 ) ) ;
#11828 = ORIENTED_EDGE ( 'NONE', *, *, #11276, .T. ) ;
#11829 = ADVANCED_FACE ( 'NONE', ( #12692 ), #19244, .T. ) ;
#11830 = B_SPLINE_CURVE_WITH_KNOTS ( 'NONE', 3,
 ( #24440, #24288, #2616, #19755, #26800, #29285, #7928, #5427, #19455, #9788, #19305, #16809, #26954, #21793, #28973, #7296, #14297, #23816, #17113, #19606, #12136, #26323, #26637, #2937, #4957, #12455, #21945, #572, #272, #14930, #3080, #2466, #9639, #11984, #26477, #118, #19151, #14623, #28666, #2775, #1053, #8077, #22411, #3388, #8224, #5576, #20071, #29908, #29591, #10710, #15215, #22252 ),
 .UNSPECIFIED., .F., .F.,
 ( 4, 2, 2, 2, 2, 2, 2, 2, 2, 2, 2, 2, 2, 2, 2, 2, 2, 2, 2, 2, 2, 2, 2, 2, 2, 4 ),
 ( 1.813955208755348987E-18, 0.002948126770087892892, 0.004422190155131839120, 0.005896253540175785783, 0.008844380310263671302, 0.01031844369530762057, 0.01179250708035156983, 0.01474063385043945969, 0.01621469723548340028, 0.01768876062052733913, 0.01916282400557127452, 0.02063688739061521338, 0.02358501416070309109, 0.02505907754574704382, 0.02653314093079099656, 0.02948126770087891590, 0.03095533108592286517, 0.03242939447096682831, 0.03390345785601079492, 0.03537752124105476154, 0.03832564801114272945, 0.03979971139618670994, 0.04127377478123069043, 0.04422190155131865141, 0.04569596493636263884, 0.04717002832140662627 ),
 .UNSPECIFIED. ) ;
#11831 = CARTESIAN_POINT ( 'NONE',  ( 25.23756106473024730, -11.43858098102957577, -1.500000000000000000 ) ) ;
#11832 = CARTESIAN_POINT ( 'NONE',  ( 19.68435877536853695, 3.639270104310703857, 18.44527579819791185 ) ) ;
#11833 = AXIS2_PLACEMENT_3D ( 'NONE', #6396, #27920, #26028 ) ;
#11834 = CARTESIAN_POINT ( 'NONE',  ( -24.75800239156184190, 7.045788922043114688, 49.25937209215337020 ) ) ;
#11835 = ORIENTED_EDGE ( 'NONE', *, *, #2713, .F. ) ;
#11836 = CIRCLE ( 'NONE', #20301, 0.7500000000000006661 ) ;
#11837 = CARTESIAN_POINT ( 'NONE',  ( 15.60425753233939616, -6.827323759874019515, 20.22273502201483808 ) ) ;
#11838 = VERTEX_POINT ( 'NONE', #22187 ) ;
#11839 = EDGE_CURVE ( 'NONE', #8702, #14537, #28754, .T. ) ;
#11840 = VERTEX_POINT ( 'NONE', #21714 ) ;
#11841 = EDGE_CURVE ( 'NONE', #8036, #13645, #14702, .T. ) ;
#11842 = VECTOR ( 'NONE', #15357, 1000.000000000000000 ) ;
#11843 = CARTESIAN_POINT ( 'NONE',  ( -4.163336342344337027E-14, 1.387778780781445676E-14, 37.50000000000000000 ) ) ;
#11844 = DIRECTION ( 'NONE',  ( 0.000000000000000000, 0.000000000000000000, 1.000000000000000000 ) ) ;
#11845 = AXIS2_PLACEMENT_3D ( 'NONE', #25284, #13451, #18265 ) ;
#11846 = CIRCLE ( 'NONE', #22800, 19.49999999999996447 ) ;
#11847 = CARTESIAN_POINT ( 'NONE',  ( 1.279633210264037979, -19.97671948047977963, 6.233981582756856987 ) ) ;
#11848 = CARTESIAN_POINT ( 'NONE',  ( -10.15881039258890794, -41.03878892760899078, 28.96756984954204839 ) ) ;
#11849 = LINE ( 'NONE', #21346, #5884 ) ;
#11850 = CARTESIAN_POINT ( 'NONE',  ( 16.83427080350347183, 2.570616772381428383, 18.55820869691756769 ) ) ;
#11851 = VERTEX_POINT ( 'NONE', #7392 ) ;
#11852 = CARTESIAN_POINT ( 'NONE',  ( -16.95590486909633299, 1.723587065725477263, 18.34969686940296185 ) ) ;
#11853 = CARTESIAN_POINT ( 'NONE',  ( -50.00000000000000000, 50.00000000000000000, 62.49999999999999289 ) ) ;
#11854 = CARTESIAN_POINT ( 'NONE',  ( 0.000000000000000000, 0.000000000000000000, 196.3477631085023631 ) ) ;
#11855 = CARTESIAN_POINT ( 'NONE',  ( 0.7220001660362450613, 9.454746441592961403, 1.500000000000001332 ) ) ;
#11856 = ORIENTED_EDGE ( 'NONE', *, *, #16630, .T. ) ;
#11857 = ORIENTED_EDGE ( 'NONE', *, *, #11460, .T. ) ;
#11858 = AXIS2_PLACEMENT_3D ( 'NONE', #7398, #23753, #21723 ) ;
#11859 = CARTESIAN_POINT ( 'NONE',  ( -4.776122516674677878E-15, -42.50000000000000000, 24.50000000000000000 ) ) ;
#11860 = EDGE_CURVE ( 'NONE', #11332, #15421, #24198, .T. ) ;
#11861 = DIRECTION ( 'NONE',  ( 1.000000000000000000, 0.000000000000000000, -0.000000000000000000 ) ) ;
#11862 = ADVANCED_FACE ( 'NONE', ( #10181, #29211, #7546 ), #10036, .T. ) ;
#11863 = FACE_OUTER_BOUND ( 'NONE', #18075, .T. ) ;
#11864 = CARTESIAN_POINT ( 'NONE',  ( 7.500000000000000000, 0.000000000000000000, 0.000000000000000000 ) ) ;
#11865 = ADVANCED_FACE ( 'NONE', ( #14859 ), #5506, .T. ) ;
#11866 = DIRECTION ( 'NONE',  ( 1.000000000000000000, 0.000000000000000000, 0.000000000000000000 ) ) ;
#11867 = EDGE_CURVE ( 'NONE', #357, #10573, #9846, .T. ) ;
#11868 = CARTESIAN_POINT ( 'NONE',  ( -4.346265761537661199, -39.21681178834676018, 27.50000000000000355 ) ) ;
#11869 = FACE_OUTER_BOUND ( 'NONE', #16388, .T. ) ;
#11870 = AXIS2_PLACEMENT_3D ( 'NONE', #13421, #27290, #5921 ) ;
#11871 = ORIENTED_EDGE ( 'NONE', *, *, #1976, .F. ) ;
#11872 = EDGE_CURVE ( 'NONE', #6239, #14509, #22098, .T. ) ;
#11873 = CIRCLE ( 'NONE', #28816, 12.18947652193948272 ) ;
#11874 = CARTESIAN_POINT ( 'NONE',  ( -34.45740060152252227, -11.48158507098138692, 34.49999999999999289 ) ) ;
#11875 = AXIS2_PLACEMENT_3D ( 'NONE', #28269, #28422, #19201 ) ;
#11876 = DIRECTION ( 'NONE',  ( 0.000000000000000000, -1.132880637372608986E-16, 1.000000000000000000 ) ) ;
#11877 = DIRECTION ( 'NONE',  ( -1.000000000000000000, 0.000000000000000000, 0.000000000000000000 ) ) ;
#11878 = EDGE_CURVE ( 'NONE', #15766, #13097, #27499, .T. ) ;
#11879 = ORIENTED_EDGE ( 'NONE', *, *, #1023, .T. ) ;
#11880 = DIRECTION ( 'NONE',  ( 1.000000000000000000, 0.000000000000000000, 0.000000000000000000 ) ) ;
#11881 = ORIENTED_EDGE ( 'NONE', *, *, #2938, .F. ) ;
#11882 = EDGE_CURVE ( 'NONE', #25305, #30087, #1826, .T. ) ;
#11883 = DIRECTION ( 'NONE',  ( 1.000000000000000000, 0.000000000000000000, -0.000000000000000000 ) ) ;
#11884 = CIRCLE ( 'NONE', #13865, 0.7500000000000011102 ) ;
#11885 = CARTESIAN_POINT ( 'NONE',  ( -19.62486380000566655, 38.57793056412522503, -16.50000000000000000 ) ) ;
#11886 = VERTEX_POINT ( 'NONE', #20613 ) ;
#11887 = CARTESIAN_POINT ( 'NONE',  ( 29.06267346339080504, -23.31480175602749938, 27.50000000000000355 ) ) ;
#11888 = CARTESIAN_POINT ( 'NONE',  ( -0.6210184355500070197, 9.062880100047294718, 13.22130136205108997 ) ) ;
#11889 = CARTESIAN_POINT ( 'NONE',  ( 10.69247012765650062, -13.31688477309528196, 19.28454053338348473 ) ) ;
#11890 = DIRECTION ( 'NONE',  ( 1.000000000000000000, 0.000000000000000000, 0.000000000000000000 ) ) ;
#11891 = DIRECTION ( 'NONE',  ( 0.000000000000000000, -1.132880637372608986E-16, 1.000000000000000000 ) ) ;
#11892 = CARTESIAN_POINT ( 'NONE',  ( 10.99809977392671279, -16.70505906359367643, 20.34789198813115618 ) ) ;
#11893 =( GEOMETRIC_REPRESENTATION_CONTEXT ( 3 ) GLOBAL_UNCERTAINTY_ASSIGNED_CONTEXT ( ( #27959 ) ) GLOBAL_UNIT_ASSIGNED_CONTEXT ( ( #4005, #5883, #23013 ) ) REPRESENTATION_CONTEXT ( 'NONE', 'WORKASPACE' ) );
#11894 = EDGE_LOOP ( 'NONE', ( #15548, #3984, #10098, #6953 ) ) ;
#11895 = ADVANCED_FACE ( 'NONE', ( #8624 ), #29991, .F. ) ;
#11896 = DIRECTION ( 'NONE',  ( 0.000000000000000000, 1.000000000000000000, 0.000000000000000000 ) ) ;
#11897 = CIRCLE ( 'NONE', #17368, 4.999999999999997335 ) ;
#11898 = CIRCLE ( 'NONE', #10903, 0.7499999999999997780 ) ;
#11899 = CARTESIAN_POINT ( 'NONE',  ( 35.76344986163714168, -22.29344514668044752, -19.50000000000000355 ) ) ;
#11900 = AXIS2_PLACEMENT_3D ( 'NONE', #1447, #10326, #10960 ) ;
#11901 = CARTESIAN_POINT ( 'NONE',  ( 39.87808514715981545, 7.028748144847113188, -14.83333104077163256 ) ) ;
#11902 = VERTEX_POINT ( 'NONE', #3787 ) ;
#11903 = DIRECTION ( 'NONE',  ( 1.000000000000000000, 0.000000000000000000, 0.000000000000000000 ) ) ;
#11904 = CARTESIAN_POINT ( 'NONE',  ( -14.92657760816261359, -8.264136099378399436, 20.19593175699879595 ) ) ;
#11905 = EDGE_CURVE ( 'NONE', #16299, #19910, #30134, .T. ) ;
#11906 = DIRECTION ( 'NONE',  ( 1.000000000000000000, 0.000000000000000000, 0.000000000000000000 ) ) ;
#11907 = EDGE_CURVE ( 'NONE', #30397, #26027, #3311, .T. ) ;
#11908 = CARTESIAN_POINT ( 'NONE',  ( -15.10419704716067102, -17.26937953831884442, 1.500000000000000000 ) ) ;
#11909 = CARTESIAN_POINT ( 'NONE',  ( 0.000000000000000000, 44.39187623478217404, -19.50000000000000355 ) ) ;
#11910 = CIRCLE ( 'NONE', #7931, 10.00000000000000000 ) ;
#11911 = ORIENTED_EDGE ( 'NONE', *, *, #2312, .T. ) ;
#11912 = DIRECTION ( 'NONE',  ( 1.000000000000000000, 0.000000000000000000, 0.000000000000000000 ) ) ;
#11913 = CARTESIAN_POINT ( 'NONE',  ( -5.549075634136967139, 16.11684027513961226, 5.652196082368482699 ) ) ;
#11914 = CARTESIAN_POINT ( 'NONE',  ( 31.78338042482835846, 20.06055218721173006, 37.49999999987489474 ) ) ;
#11915 = DIRECTION ( 'NONE',  ( -0.000000000000000000, 0.8660254037844378194, 0.5000000000000015543 ) ) ;
#11916 = ORIENTED_EDGE ( 'NONE', *, *, #1608, .F. ) ;
#11917 = AXIS2_PLACEMENT_3D ( 'NONE', #18016, #29551, #13333 ) ;
#11918 = DIRECTION ( 'NONE',  ( -0.000000000000000000, 1.132880637372608986E-16, -1.000000000000000000 ) ) ;
#11919 = VERTEX_POINT ( 'NONE', #27810 ) ;
#11920 = CARTESIAN_POINT ( 'NONE',  ( -2.552544030762004645, -42.50000000000000000, -1.500000000000000000 ) ) ;
#11921 = DIRECTION ( 'NONE',  ( 1.000000000000000000, 0.000000000000000000, 0.000000000000000000 ) ) ;
#11922 = EDGE_LOOP ( 'NONE', ( #4309, #14742 ) ) ;
#11923 = ORIENTED_EDGE ( 'NONE', *, *, #13186, .T. ) ;
#11924 = DIRECTION ( 'NONE',  ( 1.000000000000000000, 0.000000000000000000, 0.000000000000000000 ) ) ;
#11925 = PRODUCT_DEFINITION_SHAPE ( 'NONE', 'NONE',  #6845 ) ;
#11926 = AXIS2_PLACEMENT_3D ( 'NONE', #14429, #7413, #12095 ) ;
#11927 = ORIENTED_EDGE ( 'NONE', *, *, #6716, .F. ) ;
#11928 = ORIENTED_EDGE ( 'NONE', *, *, #16398, .T. ) ;
#11929 = CARTESIAN_POINT ( 'NONE',  ( 0.05528831664089212811, -17.02727625121208632, 20.05479082170252525 ) ) ;
#11930 = CARTESIAN_POINT ( 'NONE',  ( -7.747355498299751453, -15.21644541356980440, 6.233981582756856987 ) ) ;
#11931 = CARTESIAN_POINT ( 'NONE',  ( -2.959227181723746547, 8.499586724479465616, 1.500000000000001332 ) ) ;
#11932 = AXIS2_PLACEMENT_3D ( 'NONE', #10962, #11250, #9214 ) ;
#11933 = CARTESIAN_POINT ( 'NONE',  ( 1.745046693156364404, -16.98705356654485854, 19.03762469184452755 ) ) ;
#11934 = ORIENTED_EDGE ( 'NONE', *, *, #3260, .T. ) ;
#11935 = CARTESIAN_POINT ( 'NONE',  ( 10.11202017158399968, 41.14070756921128691, -1.500000000000003997 ) ) ;
#11936 = CARTESIAN_POINT ( 'NONE',  ( -23.08991993893192785, -11.27014480227852644, 45.06404153503662258 ) ) ;
#11937 = CARTESIAN_POINT ( 'NONE',  ( 14.20032907733019911, 14.10870362182395077, 19.47783254395485031 ) ) ;
#11938 = CARTESIAN_POINT ( 'NONE',  ( 1.000000000000008438, 13.00000000000001421, 1.500000000000001332 ) ) ;
#11939 = ORIENTED_EDGE ( 'NONE', *, *, #16224, .T. ) ;
#11940 = ADVANCED_FACE ( 'NONE', ( #18137 ), #5817, .F. ) ;
#11941 = ADVANCED_FACE ( 'NONE', ( #3951 ), #24678, .T. ) ;
#11942 = AXIS2_PLACEMENT_3D ( 'NONE', #3482, #22487, #1134 ) ;
#11943 = DIRECTION ( 'NONE',  ( 0.000000000000000000, 0.000000000000000000, 1.000000000000000000 ) ) ;
#11944 = LINE ( 'NONE', #9589, #16759 ) ;
#11945 = CARTESIAN_POINT ( 'NONE',  ( -12.71614549213777678, 11.31496011770029853, 19.47784884541372818 ) ) ;
#11946 = CARTESIAN_POINT ( 'NONE',  ( -11.46182693247433804, -1.387778780781445676E-14, -1.500000000000000000 ) ) ;
#11947 = DIRECTION ( 'NONE',  ( 0.000000000000000000, 0.000000000000000000, 1.000000000000000000 ) ) ;
#11948 = CARTESIAN_POINT ( 'NONE',  ( -67.00000000000000000, -50.00000000000000000, 59.49999999999999289 ) ) ;
#11949 = ORIENTED_EDGE ( 'NONE', *, *, #1859, .F. ) ;
#11950 = ORIENTED_EDGE ( 'NONE', *, *, #10742, .T. ) ;
#11951 = CARTESIAN_POINT ( 'NONE',  ( 32.93066663369882718, 23.11087908567089855, -3.166603007242253298 ) ) ;
#11952 = CARTESIAN_POINT ( 'NONE',  ( -31.18700685316050780, 26.11823559932051353, -1.500000000000000000 ) ) ;
#11953 = DIRECTION ( 'NONE',  ( 1.000000000000000000, 0.000000000000000000, 0.000000000000000000 ) ) ;
#11954 = CARTESIAN_POINT ( 'NONE',  ( -42.49999999999998579, -50.00000000000000000, 52.07879600563550326 ) ) ;
#11955 = ORIENTED_EDGE ( 'NONE', *, *, #9737, .T. ) ;
#11956 = DIRECTION ( 'NONE',  ( 0.000000000000000000, 0.000000000000000000, 1.000000000000000000 ) ) ;
#11957 = CARTESIAN_POINT ( 'NONE',  ( 18.30570112562006102, -8.101025642224000123, 20.34789198813115263 ) ) ;
#11958 = FACE_OUTER_BOUND ( 'NONE', #2796, .T. ) ;
#11959 = ORIENTED_EDGE ( 'NONE', *, *, #30141, .T. ) ;
#11960 = CARTESIAN_POINT ( 'NONE',  ( 4.870982490315499014, 16.31268916845846206, 18.80699882434806369 ) ) ;
#11961 = CARTESIAN_POINT ( 'NONE',  ( 12.06031594364852033, 12.06435167025952282, 7.559636331181775581 ) ) ;
#11962 = AXIS2_PLACEMENT_3D ( 'NONE', #25204, #8543, #30196 ) ;
#11963 = CARTESIAN_POINT ( 'NONE',  ( 25.64627119138473432, -23.40052582045089480, -6.500000000000000888 ) ) ;
#11964 = CARTESIAN_POINT ( 'NONE',  ( -30.95493403226913998, 21.31809426914557193, 37.49999999984183319 ) ) ;
#11965 = VERTEX_POINT ( 'NONE', #12847 ) ;
#11966 = DIRECTION ( 'NONE',  ( 0.000000000000000000, 1.132880637372608986E-16, -1.000000000000000000 ) ) ;
#11967 = CARTESIAN_POINT ( 'NONE',  ( -9.301547456646385825, 8.591538895647085283, 1.500000000000000000 ) ) ;
#11968 = CARTESIAN_POINT ( 'NONE',  ( -29.55332031600282150, -27.89853503084716380, -1.500000000000000000 ) ) ;
#11969 = VERTEX_POINT ( 'NONE', #20321 ) ;
#11970 = CARTESIAN_POINT ( 'NONE',  ( -15.49172192819003691, -7.063155179282995633, 6.018569869498933578 ) ) ;
#11971 = CARTESIAN_POINT ( 'NONE',  ( 0.000000000000000000, 0.000000000000000000, -1.500000000000000000 ) ) ;
#11972 = DIRECTION ( 'NONE',  ( -0.9898214418809326842, -0.1423148382732852824, 0.000000000000000000 ) ) ;
#11973 = VECTOR ( 'NONE', #15312, 1000.000000000000000 ) ;
#11974 = DIRECTION ( 'NONE',  ( -0.000000000000000000, -0.000000000000000000, 1.000000000000000000 ) ) ;
#11975 = CARTESIAN_POINT ( 'NONE',  ( -17.06520330450695155, 0.6550632133703635507, 19.14333282897057842 ) ) ;
#11976 = DIRECTION ( 'NONE',  ( -0.8412535328311884220, -0.5406408174555862312, 0.000000000000000000 ) ) ;
#11977 = ORIENTED_EDGE ( 'NONE', *, *, #12771, .F. ) ;
#11978 = CYLINDRICAL_SURFACE ( 'NONE', #6290, 11.99999999999999645 ) ;
#11979 = DIRECTION ( 'NONE',  ( -0.000000000000000000, 1.132880637372608986E-16, -1.000000000000000000 ) ) ;
#11980 = ORIENTED_EDGE ( 'NONE', *, *, #25034, .F. ) ;
#11981 = AXIS2_PLACEMENT_3D ( 'NONE', #25641, #21085, #4418 ) ;
#11982 = ORIENTED_EDGE ( 'NONE', *, *, #14536, .T. ) ;
#11983 = CARTESIAN_POINT ( 'NONE',  ( 4.335955696074039523, 19.52440042691176458, 19.61564845152807735 ) ) ;
#11984 = CARTESIAN_POINT ( 'NONE',  ( -12.98621692273268913, 48.28473667581032913, -62.52316196060546361 ) ) ;
#11985 = CARTESIAN_POINT ( 'NONE',  ( 3.683253992019826839, -8.303920738747226693, -1.500000000000002665 ) ) ;
#11986 = ORIENTED_EDGE ( 'NONE', *, *, #15917, .F. ) ;
#11987 = DIRECTION ( 'NONE',  ( -0.000000000000000000, -0.000000000000000000, -1.000000000000000000 ) ) ;
#11988 =( REPRESENTATION_RELATIONSHIP ('NONE','NONE', #19885, #19685 ) REPRESENTATION_RELATIONSHIP_WITH_TRANSFORMATION ( #29556 )SHAPE_REPRESENTATION_RELATIONSHIP( ) );
#11989 = ORIENTED_EDGE ( 'NONE', *, *, #20437, .F. ) ;
#11990 = CARTESIAN_POINT ( 'NONE',  ( 16.09309408545196618, -5.686824080536027282, 18.64703902303423178 ) ) ;
#11991 = CARTESIAN_POINT ( 'NONE',  ( -15.97601187733367922, 12.03191775062556346, 19.21940439362674624 ) ) ;
#11992 = VECTOR ( 'NONE', #30848, 1000.000000000000000 ) ;
#11993 = CARTESIAN_POINT ( 'NONE',  ( -24.57973596967191554, 7.302173446879558938, 49.35895363830209703 ) ) ;
#11994 = ORIENTED_EDGE ( 'NONE', *, *, #28805, .T. ) ;
#11995 = CARTESIAN_POINT ( 'NONE',  ( 24.14264434021282213, -13.29031772318284865, 43.19835251277588384 ) ) ;
#11996 = VERTEX_POINT ( 'NONE', #986 ) ;
#11997 = ORIENTED_EDGE ( 'NONE', *, *, #26946, .T. ) ;
#11998 = EDGE_CURVE ( 'NONE', #20938, #3989, #15926, .T. ) ;
#11999 = CARTESIAN_POINT ( 'NONE',  ( -24.03057240117691862, 26.57182937991348481, 26.54355021145563143 ) ) ;
#12000 = CARTESIAN_POINT ( 'NONE',  ( -17.67829152986845642, -9.353438168054491797, 6.037995405461185960 ) ) ;
#12001 = DIRECTION ( 'NONE',  ( -1.000000000000000000, 0.000000000000000000, 0.000000000000000000 ) ) ;
#12002 = LINE ( 'NONE', #4817, #1094 ) ;
#12003 = CARTESIAN_POINT ( 'NONE',  ( 6.899999999999999467, -10.39230484541329247, 8.776157072412030708E-17 ) ) ;
#12004 = EDGE_CURVE ( 'NONE', #12022, #26711, #26880, .T. ) ;
#12005 = CARTESIAN_POINT ( 'NONE',  ( 0.000000000000000000, 0.000000000000000000, -1.500000000000000000 ) ) ;
#12006 = EDGE_LOOP ( 'NONE', ( #14464, #25704 ) ) ;
#12007 = EDGE_CURVE ( 'NONE', #8550, #24015, #8458, .T. ) ;
#12008 = CIRCLE ( 'NONE', #2548, 1.000000000000010436 ) ;
#12009 = CARTESIAN_POINT ( 'NONE',  ( -24.35970437652574105, -13.37404834226503247, -16.55003854064094426 ) ) ;
#12010 = DIRECTION ( 'NONE',  ( 0.000000000000000000, 0.000000000000000000, 1.000000000000000000 ) ) ;
#12011 = CIRCLE ( 'NONE', #21459, 1.447898107987198646 ) ;
#12012 = CARTESIAN_POINT ( 'NONE',  ( -2.555255504830907132, 9.131494062835638914, 1.500000000000001332 ) ) ;
#12013 = ORIENTED_EDGE ( 'NONE', *, *, #12392, .T. ) ;
#12014 = EDGE_LOOP ( 'NONE', ( #5387, #9223, #5996, #16685 ) ) ;
#12015 = CARTESIAN_POINT ( 'NONE',  ( -25.10445388623454477, -25.60065097860747585, 1.500000000000000000 ) ) ;
#12016 = FACE_OUTER_BOUND ( 'NONE', #28851, .T. ) ;
#12017 = CARTESIAN_POINT ( 'NONE',  ( 18.39103589699442054, -7.860502636612779703, 18.34869673959211767 ) ) ;
#12018 = CARTESIAN_POINT ( 'NONE',  ( -3.912171961292012057, -8.637616862297827325, 21.50000000000000000 ) ) ;
#12019 = CARTESIAN_POINT ( 'NONE',  ( -33.87117184736123221, -13.39279440468763660, 27.50000000000000711 ) ) ;
#12020 = EDGE_CURVE ( 'NONE', #26415, #22510, #10647, .T. ) ;
#12021 = CARTESIAN_POINT ( 'NONE',  ( -25.48568755041063838, 12.36160011285429583, 1.500000000000001332 ) ) ;
#12022 = VERTEX_POINT ( 'NONE', #8317 ) ;
#12023 = CARTESIAN_POINT ( 'NONE',  ( -4.082808312865499722, -39.26097399651455788, 34.49999999999998579 ) ) ;
#12024 = CARTESIAN_POINT ( 'NONE',  ( -18.04156136322730219, -8.631457789788591128, 18.34798005863226678 ) ) ;
#12025 = DIRECTION ( 'NONE',  ( 0.000000000000000000, 0.000000000000000000, -1.000000000000000000 ) ) ;
#12026 = ORIENTED_EDGE ( 'NONE', *, *, #6962, .F. ) ;
#12027 = CARTESIAN_POINT ( 'NONE',  ( 8.752572334588121450, -2.431858781452763019, -1.500000000000001998 ) ) ;
#12028 = ORIENTED_EDGE ( 'NONE', *, *, #9993, .F. ) ;
#12029 = FACE_BOUND ( 'NONE', #12466, .T. ) ;
#12030 = EDGE_CURVE ( 'NONE', #6265, #24299, #9527, .T. ) ;
#12031 = AXIS2_PLACEMENT_3D ( 'NONE', #30440, #11428, #21209 ) ;
#12032 = CARTESIAN_POINT ( 'NONE',  ( -22.86203465710450899, 36.41373663176752018, -16.50000000000000000 ) ) ;
#12033 = ORIENTED_EDGE ( 'NONE', *, *, #27367, .T. ) ;
#12034 = CARTESIAN_POINT ( 'NONE',  ( 35.16664802458688399, -8.537212109034927110, 27.50000000000000355 ) ) ;
#12035 = EDGE_CURVE ( 'NONE', #17814, #4181, #5757, .T. ) ;
#12036 = CARTESIAN_POINT ( 'NONE',  ( 3.903322525700887002, 49.84968173887558152, -40.50827906751979413 ) ) ;
#12037 = ADVANCED_FACE ( 'NONE', ( #2045 ), #16396, .F. ) ;
#12038 = CARTESIAN_POINT ( 'NONE',  ( 9.860909914091285700, -13.90333503830274253, 20.34789198813115263 ) ) ;
#12039 = CARTESIAN_POINT ( 'NONE',  ( 33.53985887099113228, -24.80926055130403896, -16.50000000000000000 ) ) ;
#12040 = DIRECTION ( 'NONE',  ( -1.000000000000000000, -0.000000000000000000, -0.000000000000000000 ) ) ;
#12041 = CARTESIAN_POINT ( 'NONE',  ( 33.56327786402390245, -10.34181101807379477, 39.87954049117192312 ) ) ;
#12042 = ORIENTED_EDGE ( 'NONE', *, *, #10466, .F. ) ;
#12043 = EDGE_CURVE ( 'NONE', #27530, #14763, #30585, .T. ) ;
#12044 = AXIS2_PLACEMENT_3D ( 'NONE', #21816, #28992, #5285 ) ;
#12045 = CARTESIAN_POINT ( 'NONE',  ( 24.03057240117690441, -26.57182937991349903, 26.54355021145562787 ) ) ;
#12046 = CARTESIAN_POINT ( 'NONE',  ( -13.22505861668333083, 42.10773672057167261, -19.50000000000000355 ) ) ;
#12047 = DIRECTION ( 'NONE',  ( 0.000000000000000000, 0.000000000000000000, 1.000000000000000000 ) ) ;
#12048 = ORIENTED_EDGE ( 'NONE', *, *, #4963, .T. ) ;
#12049 = CARTESIAN_POINT ( 'NONE',  ( 2.703030265324084080, -12.75514121382991384, 1.500000000000001332 ) ) ;
#12050 = CARTESIAN_POINT ( 'NONE',  ( -19.62935297797563905, -3.832558109936532009, 1.500000000000001332 ) ) ;
#12052 = EDGE_CURVE ( 'NONE', #11604, #14545, #6460, .T. ) ;
#12051 = CYLINDRICAL_SURFACE ( 'NONE', #7765, 9.482273699623480212 ) ;
#12053 = FACE_OUTER_BOUND ( 'NONE', #25390, .T. ) ;
#12054 = VECTOR ( 'NONE', #17878, 1000.000000000000000 ) ;
#12055 = CARTESIAN_POINT ( 'NONE',  ( 0.000000000000000000, 44.39187623478217404, -19.50000000000000355 ) ) ;
#12056 = EDGE_CURVE ( 'NONE', #10498, #21378, #19409, .T. ) ;
#12057 = VERTEX_POINT ( 'NONE', #28560 ) ;
#12058 = LINE ( 'NONE', #14393, #5435 ) ;
#12059 = EDGE_CURVE ( 'NONE', #1661, #16043, #19907, .T. ) ;
#12060 = CARTESIAN_POINT ( 'NONE',  ( 36.26666421214746094, 15.68564761223754900, 31.47842155818181809 ) ) ;
#12061 = CARTESIAN_POINT ( 'NONE',  ( -6.910239377218537093, 18.76835738875812964, 6.392525840300343987 ) ) ;
#12062 = ORIENTED_EDGE ( 'NONE', *, *, #27609, .F. ) ;
#12063 = ORIENTED_EDGE ( 'NONE', *, *, #13806, .T. ) ;
#12064 = CARTESIAN_POINT ( 'NONE',  ( 7.500000000000000000, 9.184850993605147944E-16, -16.50000000000000000 ) ) ;
#12065 = CARTESIAN_POINT ( 'NONE',  ( -28.34828976096172681, -29.18752572968383063, 1.500000000000000000 ) ) ;
#12066 = ORIENTED_EDGE ( 'NONE', *, *, #1417, .F. ) ;
#12067 = ORIENTED_EDGE ( 'NONE', *, *, #18492, .F. ) ;
#12068 = CARTESIAN_POINT ( 'NONE',  ( -10.39781135303995008, -17.08517550777068905, 5.652912763329821288 ) ) ;
#12069 = VECTOR ( 'NONE', #4108, 1000.000000000000000 ) ;
#12070 = ORIENTED_EDGE ( 'NONE', *, *, #26562, .T. ) ;
#12071 = ORIENTED_EDGE ( 'NONE', *, *, #23082, .F. ) ;
#12072 = VERTEX_POINT ( 'NONE', #13622 ) ;
#12073 = CARTESIAN_POINT ( 'NONE',  ( -0.1765357775187695322, -17.02148976770177669, 19.00652017443069752 ) ) ;
#12074 = EDGE_CURVE ( 'NONE', #21154, #17232, #27957, .T. ) ;
#12075 = ADVANCED_FACE ( 'NONE', ( #1744 ), #23704, .F. ) ;
#12076 = CARTESIAN_POINT ( 'NONE',  ( -10.33762405876901447, -17.14187335405548751, 7.627891251804737927 ) ) ;
#12077 = LINE ( 'NONE', #10042, #24300 ) ;
#12078 = ORIENTED_EDGE ( 'NONE', *, *, #8281, .F. ) ;
#12079 = CARTESIAN_POINT ( 'NONE',  ( 18.33793066653144521, -7.982499537706466697, 5.652196082369965069 ) ) ;
#12080 = B_SPLINE_CURVE_WITH_KNOTS ( 'NONE', 3,
 ( #15516, #13039, #10683, #29713, #1643, #22845, #1495, #8359, #30025, #11003, #11306, #17875, #3674, #30327, #13189, #11156, #30174, #20503 ),
 .UNSPECIFIED., .F., .F.,
 ( 4, 2, 2, 2, 2, 2, 2, 2, 4 ),
 ( 0.000000000000000000, 0.0003967869494442890772, 0.0007935738988885781544, 0.001190360848332867177, 0.001587147797777156309, 0.001983934747221445440, 0.002380721696665734355, 0.002777508646110023703, 0.003174295595554312618 ),
 .UNSPECIFIED. ) ;
#12081 = CARTESIAN_POINT ( 'NONE',  ( -23.07950435457407679, -11.50806656539752737, 44.96784366550136980 ) ) ;
#12082 = EDGE_CURVE ( 'NONE', #15261, #27429, #10945, .T. ) ;
#12083 = CARTESIAN_POINT ( 'NONE',  ( 11.92830948316210105, 12.20365889974008944, 20.13759033520874908 ) ) ;
#12084 = DIRECTION ( 'NONE',  ( 0.000000000000000000, -0.000000000000000000, 1.000000000000000000 ) ) ;
#12085 = VERTEX_POINT ( 'NONE', #4694 ) ;
#12086 = ADVANCED_FACE ( 'NONE', ( #2200 ), #1937, .T. ) ;
#12087 = CARTESIAN_POINT ( 'NONE',  ( 6.974883619896790954, 5.687793815610376669, 21.50000000000000000 ) ) ;
#12088 = CARTESIAN_POINT ( 'NONE',  ( 7.730328572437743517, -4.608906612435629491, 1.500000000000001332 ) ) ;
#12089 = CARTESIAN_POINT ( 'NONE',  ( 10.47960520055065992, -7.757439966934453146, 1.500000000000001332 ) ) ;
#12090 = VECTOR ( 'NONE', #11065, 1000.000000000000000 ) ;
#12091 = CARTESIAN_POINT ( 'NONE',  ( -19.84344116185557283, 2.497567387674354489, 7.652108011868850035 ) ) ;
#12092 = DIRECTION ( 'NONE',  ( 1.000000000000000000, 0.000000000000000000, 0.000000000000000000 ) ) ;
#12093 = ADVANCED_FACE ( 'NONE', ( #14518, #2820, #12029 ), #17159, .T. ) ;
#12094 = VECTOR ( 'NONE', #17463, 1000.000000000000000 ) ;
#12095 = DIRECTION ( 'NONE',  ( 0.000000000000000000, 0.000000000000000000, 1.000000000000000000 ) ) ;
#12096 = DIRECTION ( 'NONE',  ( -0.000000000000000000, -0.000000000000000000, 1.000000000000000000 ) ) ;
#12097 = VERTEX_POINT ( 'NONE', #24011 ) ;
#12098 = ORIENTED_EDGE ( 'NONE', *, *, #16475, .F. ) ;
#12099 = CARTESIAN_POINT ( 'NONE',  ( -29.99999999999933209, 1.755172820525642916E-14, 67.49999999999997158 ) ) ;
#12100 = CARTESIAN_POINT ( 'NONE',  ( -5.488535287689155773, 19.23255048776056952, 18.47110296274025387 ) ) ;
#12101 = DIRECTION ( 'NONE',  ( -0.000000000000000000, 0.000000000000000000, 1.000000000000000000 ) ) ;
#12102 = CARTESIAN_POINT ( 'NONE',  ( 18.58529988941437949, 7.388276390372287672, 24.50000000000000000 ) ) ;
#12103 = ORIENTED_EDGE ( 'NONE', *, *, #26915, .F. ) ;
#12104 = APPLICATION_PROTOCOL_DEFINITION ( 'draft international standard', 'automotive_design', 1998, #7195 ) ;
#12105 = CARTESIAN_POINT ( 'NONE',  ( 16.19468640091380607, -5.422205736210270466, 19.47952243369110548 ) ) ;
#12106 = CARTESIAN_POINT ( 'NONE',  ( 4.817555027346760887, 16.32979927342788784, 7.272049892295485485 ) ) ;
#12107 = ADVANCED_FACE ( 'NONE', ( #12343 ), #2664, .T. ) ;
#12108 = ORIENTED_EDGE ( 'NONE', *, *, #20624, .T. ) ;
#12109 = CARTESIAN_POINT ( 'NONE',  ( 4.874170568648001023, 16.31160065975151241, 19.87181966307587544 ) ) ;
#12110 = CARTESIAN_POINT ( 'NONE',  ( 14.21537200517654576, 14.09360477215025931, 6.892848776733236704 ) ) ;
#12111 = ADVANCED_FACE ( 'NONE', ( #26680 ), #481, .F. ) ;
#12112 = CARTESIAN_POINT ( 'NONE',  ( -22.86252527946696844, -36.41647737164041132, -16.50000000000000000 ) ) ;
#12113 = CARTESIAN_POINT ( 'NONE',  ( -36.66434526847238828, 7.899044488850192280, 37.50000000002572875 ) ) ;
#12114 = EDGE_LOOP ( 'NONE', ( #3393, #22028, #8268, #11193 ) ) ;
#12115 = CARTESIAN_POINT ( 'NONE',  ( -77.99999999999998579, -42.49999999999998579, 1.500000000000000222 ) ) ;
#12116 = AXIS2_PLACEMENT_3D ( 'NONE', #9310, #18836, #28353 ) ;
#12117 = VECTOR ( 'NONE', #22792, 1000.000000000000000 ) ;
#12118 = CARTESIAN_POINT ( 'NONE',  ( 18.91580660644371292, 38.99778335661734729, -16.50000000000000000 ) ) ;
#12119 = ORIENTED_EDGE ( 'NONE', *, *, #2901, .F. ) ;
#12120 = DIRECTION ( 'NONE',  ( 0.000000000000000000, -1.000000000000000000, 0.000000000000000000 ) ) ;
#12121 = CARTESIAN_POINT ( 'NONE',  ( -8.757878075398936701, -7.394122547431892123, 1.500000000000000000 ) ) ;
#12122 = CARTESIAN_POINT ( 'NONE',  ( 14.53509801925589784, 13.73847344395387537, 5.779535427900759359 ) ) ;
#12123 = CARTESIAN_POINT ( 'NONE',  ( -0.2311899301088659875, -17.01971842090038223, 6.755862304746362845 ) ) ;
#12124 = DIRECTION ( 'NONE',  ( -0.000000000000000000, -0.000000000000000000, 1.000000000000000000 ) ) ;
#12125 = DIRECTION ( 'NONE',  ( 1.000000000000000000, 0.000000000000000000, 0.000000000000000000 ) ) ;
#12126 = CARTESIAN_POINT ( 'NONE',  ( 36.00889349845778042, -16.33510104555887921, 16.99424500426727036 ) ) ;
#12127 = CARTESIAN_POINT ( 'NONE',  ( 9.999999999999959144, 1.510243460696181139E-14, -1.500000000000000000 ) ) ;
#12128 = ORIENTED_EDGE ( 'NONE', *, *, #20630, .T. ) ;
#12129 = DIRECTION ( 'NONE',  ( 1.000000000000000000, 0.000000000000000000, 0.000000000000000000 ) ) ;
#12130 = VECTOR ( 'NONE', #8097, 1000.000000000000000 ) ;
#12131 = LINE ( 'NONE', #11523, #1636 ) ;
#12132 = ORIENTED_EDGE ( 'NONE', *, *, #21025, .F. ) ;
#12133 = ORIENTED_EDGE ( 'NONE', *, *, #19250, .T. ) ;
#12134 = AXIS2_PLACEMENT_3D ( 'NONE', #30715, #21665, #11861 ) ;
#12135 = CARTESIAN_POINT ( 'NONE',  ( -15.97539537256529840, 12.03273630363204738, 6.788986777570705122 ) ) ;
#12136 = CARTESIAN_POINT ( 'NONE',  ( -14.20303051544474826, 47.94055110225200167, -50.15062527444063534 ) ) ;
#12137 = AXIS2_PLACEMENT_3D ( 'NONE', #18444, #20903, #4078 ) ;
#12138 = ORIENTED_EDGE ( 'NONE', *, *, #12602, .T. ) ;
#12139 = B_SPLINE_CURVE_WITH_KNOTS ( 'NONE', 3,
 ( #10656, #3028, #20014, #10192, #17676, #27195, #22040, #15326, #19700, #5517, #15019, #3495, #13008, #20165, #29686, #14527, #14205, #9852 ),
 .UNSPECIFIED., .F., .F.,
 ( 4, 2, 2, 2, 2, 2, 2, 2, 4 ),
 ( 0.003174295595554290066, 0.003570702171545513722, 0.003967108747536737812, 0.004363515323527961468, 0.004759921899519185123, 0.005156328475510408779, 0.005552735051501632435, 0.005949141627492856091, 0.006345548203484079747 ),
 .UNSPECIFIED. ) ;
#12140 = CARTESIAN_POINT ( 'NONE',  ( -13.93942108199721730, 16.65122935894503442, -1.500000000000000000 ) ) ;
#12141 = VERTEX_POINT ( 'NONE', #17320 ) ;
#12142 = CARTESIAN_POINT ( 'NONE',  ( 16.18939002998177301, -5.436351910499660711, 19.14333282897057842 ) ) ;
#12143 = CARTESIAN_POINT ( 'NONE',  ( 19.61674503250825197, 3.986191100139168775, 18.73743063545763121 ) ) ;
#12144 = EDGE_CURVE ( 'NONE', #10182, #8853, #10439, .T. ) ;
#12145 = CARTESIAN_POINT ( 'NONE',  ( -24.50429677314016175, 7.442113211156454078, 49.39104550111589020 ) ) ;
#12146 = VERTEX_POINT ( 'NONE', #19506 ) ;
#12147 = DIRECTION ( 'NONE',  ( -1.000000000000000000, 0.000000000000000000, 0.000000000000000000 ) ) ;
#12148 = VERTEX_POINT ( 'NONE', #29019 ) ;
#12149 = VERTEX_POINT ( 'NONE', #7659 ) ;
#12150 = CIRCLE ( 'NONE', #8688, 12.66227964008308682 ) ;
#12151 = AXIS2_PLACEMENT_3D ( 'NONE', #27837, #10839, #1777 ) ;
#12152 = CARTESIAN_POINT ( 'NONE',  ( 36.45295081748523103, 15.16267811623469974, 31.52271926598579199 ) ) ;
#12153 = CARTESIAN_POINT ( 'NONE',  ( -13.02230393242516371, 10.97666050933785797, 20.19668224736330941 ) ) ;
#12154 = CARTESIAN_POINT ( 'NONE',  ( -7.995704773938816956, -15.07639970738306268, 18.56793045041961321 ) ) ;
#12155 = CARTESIAN_POINT ( 'NONE',  ( 14.36006998371584054, 17.26937953831785677, 1.500000000000000000 ) ) ;
#12156 = CARTESIAN_POINT ( 'NONE',  ( -24.02386986937632685, 13.21681873352653014, 47.58048285248938214 ) ) ;
#12157 = DIRECTION ( 'NONE',  ( -0.000000000000000000, -0.000000000000000000, -1.000000000000000000 ) ) ;
#12158 = EDGE_LOOP ( 'NONE', ( #6099, #20443, #12932, #16322, #29734, #6788, #26475 ) ) ;
#12159 = CARTESIAN_POINT ( 'NONE',  ( -19.84673203616235071, 2.611426761413843778, 18.35377592296120497 ) ) ;
#12160 = CARTESIAN_POINT ( 'NONE',  ( -28.29426732178171378, 29.25030496633768706, 11.22274459460341234 ) ) ;
#12161 = DIRECTION ( 'NONE',  ( -0.000000000000000000, -0.000000000000000000, -1.000000000000000000 ) ) ;
#12162 = CARTESIAN_POINT ( 'NONE',  ( -70.00000000000000000, -65.00000000000000000, 12.49999999999999112 ) ) ;
#12163 = ORIENTED_EDGE ( 'NONE', *, *, #29642, .F. ) ;
#12164 = ORIENTED_EDGE ( 'NONE', *, *, #9150, .F. ) ;
#12165 = CARTESIAN_POINT ( 'NONE',  ( -39.52380524536136619, -7.028748154183644736, -11.49999999999999645 ) ) ;
#12166 = LINE ( 'NONE', #14501, #15098 ) ;
#12167 = DIRECTION ( 'NONE',  ( -0.5406408174555976665, 0.8412535328311810945, 0.000000000000000000 ) ) ;
#12168 = PRODUCT_DEFINITION_SHAPE ( 'NONE', 'NONE',  #30867 ) ;
#12169 = CARTESIAN_POINT ( 'NONE',  ( -4.863253556059215832, 16.31819504766686180, 18.63641924841378028 ) ) ;
#12170 = CARTESIAN_POINT ( 'NONE',  ( 11.75175153053879384, 12.38566219042179206, 7.158811349119584833 ) ) ;
#12171 = AXIS2_PLACEMENT_3D ( 'NONE', #9643, #19154, #7302 ) ;
#12172 = CARTESIAN_POINT ( 'NONE',  ( -10.18506332983503704, 29.04537757311073776, 1.500000000000001332 ) ) ;
#12173 = EDGE_LOOP ( 'NONE', ( #21910, #26795 ) ) ;
#12174 = VERTEX_POINT ( 'NONE', #1420 ) ;
#12175 = CARTESIAN_POINT ( 'NONE',  ( -33.18278998769607568, -15.34828001744181059, 34.50000000000000000 ) ) ;
#12176 = CARTESIAN_POINT ( 'NONE',  ( 0.000000000000000000, -2.435693370351110282E-15, 21.50000000000000355 ) ) ;
#12177 = DIRECTION ( 'NONE',  ( 0.000000000000000000, 1.000000000000000000, 0.000000000000000000 ) ) ;
#12178 = ORIENTED_EDGE ( 'NONE', *, *, #11284, .F. ) ;
#12179 = CARTESIAN_POINT ( 'NONE',  ( 12.71820101047899421, 11.32761398983758383, 7.500898271101006820 ) ) ;
#12180 = EDGE_LOOP ( 'NONE', ( #8949, #19217 ) ) ;
#12181 = CARTESIAN_POINT ( 'NONE',  ( 18.71162862491809875, -7.111980085401802931, 6.995624166085161910 ) ) ;
#12182 = CARTESIAN_POINT ( 'NONE',  ( 16.58239702338339683, 4.066005520117116134, 19.85459532544247452 ) ) ;
#12183 = DIRECTION ( 'NONE',  ( -0.000000000000000000, -0.000000000000000000, 1.000000000000000000 ) ) ;
#12184 = ORIENTED_EDGE ( 'NONE', *, *, #10922, .F. ) ;
#12185 = CARTESIAN_POINT ( 'NONE',  ( 18.58529988941437949, 7.388276390372287672, 24.50000000000000000 ) ) ;
#12186 = DIRECTION ( 'NONE',  ( -1.000000000000000000, -0.000000000000000000, -0.000000000000000000 ) ) ;
#12187 = ORIENTED_EDGE ( 'NONE', *, *, #23091, .T. ) ;
#12188 = CARTESIAN_POINT ( 'NONE',  ( 0.5595136366802740957, -4.349754824395941633, -9.000000000000000000 ) ) ;
#12189 = CIRCLE ( 'NONE', #8212, 11.46182693247429718 ) ;
#12190 = CARTESIAN_POINT ( 'NONE',  ( 0.000000000000000000, 5.590849009245238754, 1.500000000000000000 ) ) ;
#12191 = CARTESIAN_POINT ( 'NONE',  ( 6.187077094091595342, 11.47693674426096599, 1.500000000000001332 ) ) ;
#12192 = VERTEX_POINT ( 'NONE', #3752 ) ;
#12193 = CARTESIAN_POINT ( 'NONE',  ( -40.00000000000002842, 90.00000000000001421, 22.49999999999983302 ) ) ;
#12194 = CARTESIAN_POINT ( 'NONE',  ( 20.65888525914375862, -38.75220717792901581, -19.50000000000000355 ) ) ;
#12195 = DIRECTION ( 'NONE',  ( -0.3598999890241700306, -0.9329908884337522190, 0.000000000000000000 ) ) ;
#12196 = ORIENTED_EDGE ( 'NONE', *, *, #92, .T. ) ;
#12197 = DIRECTION ( 'NONE',  ( -0.000000000000000000, 1.132880637372608986E-16, -1.000000000000000000 ) ) ;
#12198 = CARTESIAN_POINT ( 'NONE',  ( 0.6237340761795171495, -8.999114229549588728, -1.500000000000002665 ) ) ;
#12199 = CARTESIAN_POINT ( 'NONE',  ( -15.57266529552203416, -38.96488032230103471, 1.500000000000000000 ) ) ;
#12200 = CARTESIAN_POINT ( 'NONE',  ( -40.89187623478217404, -5.790488632116337797, -19.50000000000000355 ) ) ;
#12201 = DIRECTION ( 'NONE',  ( 0.000000000000000000, -1.132880637372608986E-16, 1.000000000000000000 ) ) ;
#12202 = EDGE_CURVE ( 'NONE', #19224, #12146, #15433, .T. ) ;
#12203 = CARTESIAN_POINT ( 'NONE',  ( 35.55342103166282897, 11.99406784226782108, 37.49999999999405276 ) ) ;
#12204 = EDGE_CURVE ( 'NONE', #30019, #17362, #14303, .T. ) ;
#12205 = CARTESIAN_POINT ( 'NONE',  ( 5.352643706120463030, 7.827050521741900191, 21.50000000000000000 ) ) ;
#12206 = ORIENTED_EDGE ( 'NONE', *, *, #30686, .T. ) ;
#12207 = DIRECTION ( 'NONE',  ( 0.000000000000000000, 0.000000000000000000, 1.000000000000000000 ) ) ;
#12208 = ORIENTED_EDGE ( 'NONE', *, *, #7707, .F. ) ;
#12209 = CARTESIAN_POINT ( 'NONE',  ( -24.18511243334008043, -13.30669973338235401, 43.15324192430815486 ) ) ;
#12210 = CARTESIAN_POINT ( 'NONE',  ( -35.00000000000000000, 70.00000000000000000, 12.49999999999999112 ) ) ;
#12211 = ORIENTED_EDGE ( 'NONE', *, *, #28513, .F. ) ;
#12212 = AXIS2_PLACEMENT_3D ( 'NONE', #10490, #15469, #15625 ) ;
#12213 = VERTEX_POINT ( 'NONE', #22304 ) ;
#12214 = CARTESIAN_POINT ( 'NONE',  ( -10.29013980557132690, -17.15015428632897709, 7.626218077512938009 ) ) ;
#12215 = ADVANCED_FACE ( 'NONE', ( #20435 ), #1258, .F. ) ;
#12216 = ORIENTED_EDGE ( 'NONE', *, *, #18187, .F. ) ;
#12217 = VERTEX_POINT ( 'NONE', #20278 ) ;
#12218 = CARTESIAN_POINT ( 'NONE',  ( -0.6368756358441500787, -20.00777098345650984, 19.56050940960062690 ) ) ;
#12219 = EDGE_CURVE ( 'NONE', #16188, #13747, #8956, .T. ) ;
#12220 = CARTESIAN_POINT ( 'NONE',  ( -23.07950435457394889, 11.39182330144667432, 49.26235563386612171 ) ) ;
#12221 = CARTESIAN_POINT ( 'NONE',  ( -9.692246323650991258, -17.51472466453636656, 6.341840715582230281 ) ) ;
#12222 = DIRECTION ( 'NONE',  ( -0.000000000000000000, 1.132880637372608986E-16, -1.000000000000000000 ) ) ;
#12223 = EDGE_CURVE ( 'NONE', #13757, #20446, #26383, .T. ) ;
#12224 = CARTESIAN_POINT ( 'NONE',  ( 1.279633210264036425, -19.97671948047979029, 18.92976555901915603 ) ) ;
#12225 = ORIENTED_EDGE ( 'NONE', *, *, #5573, .T. ) ;
#12226 = CARTESIAN_POINT ( 'NONE',  ( -37.99999999999999289, 70.00000000000000000, -75.50000000000000000 ) ) ;
#12227 = ADVANCED_FACE ( 'NONE', ( #3912 ), #8407, .T. ) ;
#12228 = DIRECTION ( 'NONE',  ( -1.000000000000000000, 0.000000000000000000, 0.000000000000000000 ) ) ;
#12229 = CARTESIAN_POINT ( 'NONE',  ( 22.85867476669663745, -36.41545538135959958, -16.50000000000000000 ) ) ;
#12230 = CARTESIAN_POINT ( 'NONE',  ( 0.4831130459764284568, -19.99459506363783490, 20.34789198813115263 ) ) ;
#12231 = DIRECTION ( 'NONE',  ( 1.000000000000000000, 0.000000000000000000, 0.000000000000000000 ) ) ;
#12232 = VERTEX_POINT ( 'NONE', #5937 ) ;
#12233 = DIRECTION ( 'NONE',  ( -0.000000000000000000, -0.000000000000000000, -1.000000000000000000 ) ) ;
#12234 = DIRECTION ( 'NONE',  ( -1.000000000000000000, 0.000000000000000000, 0.000000000000000000 ) ) ;
#12235 = CARTESIAN_POINT ( 'NONE',  ( 1.000000000000008438, 13.00000000000001421, 1.500000000000001332 ) ) ;
#12236 = CIRCLE ( 'NONE', #5807, 9.482273699623480212 ) ;
#12237 = CARTESIAN_POINT ( 'NONE',  ( 0.000000000000000000, 0.000000000000000000, 9.000000000000000000 ) ) ;
#12238 = CARTESIAN_POINT ( 'NONE',  ( -18.20229063954116455, -8.330696590476666330, 18.39701043959520987 ) ) ;
#12239 = CARTESIAN_POINT ( 'NONE',  ( 22.94541271838008356, -35.03073867843704647, -6.500000000000000888 ) ) ;
#12240 = ORIENTED_EDGE ( 'NONE', *, *, #19068, .T. ) ;
#12241 = ORIENTED_EDGE ( 'NONE', *, *, #13222, .F. ) ;
#12242 = SURFACE_STYLE_FILL_AREA ( #21595 ) ;
#12243 = CARTESIAN_POINT ( 'NONE',  ( 32.74775157612609178, -27.21557300919356948, -19.50000000000000355 ) ) ;
#12244 = ADVANCED_FACE ( 'NONE', ( #3593 ), #25879, .T. ) ;
#12245 = CARTESIAN_POINT ( 'NONE',  ( -15.06643696584252368, 13.18059642443756907, 7.557577766377196582 ) ) ;
#12246 = EDGE_CURVE ( 'NONE', #438, #2953, #6399, .T. ) ;
#12247 = CARTESIAN_POINT ( 'NONE',  ( 25.64627119138473432, -23.40052582045089480, -16.50000000000000000 ) ) ;
#12248 = ORIENTED_EDGE ( 'NONE', *, *, #29224, .F. ) ;
#12249 = APPLICATION_PROTOCOL_DEFINITION ( 'draft international standard', 'automotive_design', 1998, #8205 ) ;
#12250 = EDGE_CURVE ( 'NONE', #27956, #1725, #13444, .T. ) ;
#12251 = FACE_OUTER_BOUND ( 'NONE', #23966, .T. ) ;
#12252 = AXIS2_PLACEMENT_3D ( 'NONE', #15488, #22361, #20331 ) ;
#12253 = EDGE_CURVE ( 'NONE', #18281, #22584, #28073, .T. ) ;
#12254 = DIRECTION ( 'NONE',  ( 0.4495526574063634095, 0.8932538319083086487, 0.000000000000000000 ) ) ;
#12255 = EDGE_LOOP ( 'NONE', ( #14802, #25650 ) ) ;
#12256 = CARTESIAN_POINT ( 'NONE',  ( 6.127899591227621734, 19.05688428395638923, 19.87181966307587544 ) ) ;
#12257 = EDGE_CURVE ( 'NONE', #6050, #21077, #13928, .T. ) ;
#12258 = LINE ( 'NONE', #17240, #17220 ) ;
#12259 = CARTESIAN_POINT ( 'NONE',  ( 0.8038475772933700858, -5.196152422706651564, 9.000000000000001776 ) ) ;
#12260 = CARTESIAN_POINT ( 'NONE',  ( -36.59094164303683527, -8.232679042141276327, 37.49999999998843947 ) ) ;
#12261 = VERTEX_POINT ( 'NONE', #8895 ) ;
#12262 = ADVANCED_FACE ( 'NONE', ( #6840 ), #18419, .F. ) ;
#12263 = DIRECTION ( 'NONE',  ( -0.000000000000000000, -0.000000000000000000, 1.000000000000000000 ) ) ;
#12264 = AXIS2_PLACEMENT_3D ( 'NONE', #23038, #22897, #22738 ) ;
#12265 = B_SPLINE_CURVE_WITH_KNOTS ( 'NONE', 3,
 ( #23176, #13990, #1532, #25849, #6361, #27579, #16330, #18668, #4481, #30214, #23027, #11042, #25688, #3870, #23487, #20400 ),
 .UNSPECIFIED., .F., .F.,
 ( 4, 2, 2, 2, 2, 2, 2, 4 ),
 ( 0.4999999999999999445, 0.6249999999999995559, 0.6874999999999994449, 0.7187499999999995559, 0.7499999999999997780, 0.8124999999999995559, 0.8749999999999993339, 1.000000000000000000 ),
 .UNSPECIFIED. ) ;
#12266 = EDGE_CURVE ( 'NONE', #4819, #13119, #24366, .T. ) ;
#12267 = CARTESIAN_POINT ( 'NONE',  ( -22.95669091611927826, 27.54300778121952220, 1.500000000000000000 ) ) ;
#12268 = AXIS2_PLACEMENT_3D ( 'NONE', #30401, #18413, #25873 ) ;
#12269 = FACE_OUTER_BOUND ( 'NONE', #12601, .T. ) ;
#12270 = EDGE_LOOP ( 'NONE', ( #21986, #11157, #20871, #1833 ) ) ;
#12271 = CARTESIAN_POINT ( 'NONE',  ( -18.45502384974594889, -7.754294478968726700, 6.974106381145714018 ) ) ;
#12272 = CARTESIAN_POINT ( 'NONE',  ( -4.390207617113899730, 7.856594496258241023, -3.621320343559650379 ) ) ;
#12273 = CARTESIAN_POINT ( 'NONE',  ( 1.000000000000008438, 13.00000000000001421, 1.500000000000001332 ) ) ;
#12274 = CARTESIAN_POINT ( 'NONE',  ( 0.1486850733125486546, -17.02875910996195685, 5.862424720655265098 ) ) ;
#12275 = AXIS2_PLACEMENT_3D ( 'NONE', #19743, #7283, #29272 ) ;
#12276 = DIRECTION ( 'NONE',  ( -0.000000000000000000, -0.000000000000000000, -1.000000000000000000 ) ) ;
#12277 = CARTESIAN_POINT ( 'NONE',  ( 3.118309183252346628, -17.14266753270391774, 1.500000000000000000 ) ) ;
#12278 = CARTESIAN_POINT ( 'NONE',  ( 37.85012425400401526, -10.24638405728790680, 11.80728464478693240 ) ) ;
#12279 = CYLINDRICAL_SURFACE ( 'NONE', #7922, 3.559164065751841743 ) ;
#12280 = ORIENTED_EDGE ( 'NONE', *, *, #1377, .T. ) ;
#12281 = ADVANCED_FACE ( 'NONE', ( #4198 ), #25869, .T. ) ;
#12282 = EDGE_CURVE ( 'NONE', #22753, #27284, #30099, .T. ) ;
#12283 = CARTESIAN_POINT ( 'NONE',  ( -1.073881485057738949, -0.9711784013061123266, 1.500000000000000000 ) ) ;
#12284 = ORIENTED_EDGE ( 'NONE', *, *, #24998, .T. ) ;
#12285 = VERTEX_POINT ( 'NONE', #18558 ) ;
#12286 = AXIS2_PLACEMENT_3D ( 'NONE', #3139, #10149, #9686 ) ;
#12287 = CYLINDRICAL_SURFACE ( 'NONE', #20602, 0.7500000000000006661 ) ;
#12288 = CARTESIAN_POINT ( 'NONE',  ( -4.163336342344337027E-14, 1.387778780781445676E-14, 35.37867965644034740 ) ) ;
#12289 = AXIS2_PLACEMENT_3D ( 'NONE', #2918, #2762, #2605 ) ;
#12290 = ORIENTED_EDGE ( 'NONE', *, *, #14908, .T. ) ;
#12291 = AXIS2_PLACEMENT_3D ( 'NONE', #16967, #7306, #26486 ) ;
#12292 = CARTESIAN_POINT ( 'NONE',  ( -8.159193615868369776, 3.993622308618967498, -1.500000000000001332 ) ) ;
#12293 = CARTESIAN_POINT ( 'NONE',  ( -8.835414383224247103, -14.56605378991199551, 7.595116371587256054 ) ) ;
#12294 = EDGE_LOOP ( 'NONE', ( #9559, #858, #2801, #21718 ) ) ;
#12295 = CARTESIAN_POINT ( 'NONE',  ( 16.16412758434836405, -5.502972621964707933, 18.92976555901915603 ) ) ;
#12296 = CARTESIAN_POINT ( 'NONE',  ( 19.58625041283695367, 4.133291823432034384, 19.69140814234746273 ) ) ;
#12297 = TOROIDAL_SURFACE ( 'NONE', #16277, 17.00000000000000000, 3.000000000000000000 ) ;
#12298 = DIRECTION ( 'NONE',  ( 0.000000000000000000, 0.000000000000000000, 1.000000000000000000 ) ) ;
#12299 = ORIENTED_EDGE ( 'NONE', *, *, #18725, .F. ) ;
#12300 = LINE ( 'NONE', #14478, #10842 ) ;
#12301 = ORIENTED_EDGE ( 'NONE', *, *, #10125, .T. ) ;
#12302 = CIRCLE ( 'NONE', #24806, 53.00000000000000711 ) ;
#12303 = CIRCLE ( 'NONE', #9312, 9.084132297865673777 ) ;
#12304 = EDGE_LOOP ( 'NONE', ( #28467, #22760, #14006, #12954 ) ) ;
#12305 = CIRCLE ( 'NONE', #16795, 0.7499999999999988898 ) ;
#12306 = CIRCLE ( 'NONE', #17792, 15.00000000000000000 ) ;
#12307 = CARTESIAN_POINT ( 'NONE',  ( 32.24119435725080507, -26.76047165977712794, -16.50000600000000262 ) ) ;
#12308 = CARTESIAN_POINT ( 'NONE',  ( -6.505190245242044256, 15.79074656234091201, 19.47783254395485031 ) ) ;
#12309 = CARTESIAN_POINT ( 'NONE',  ( -15.13676175850366334, 13.09931225869579308, 20.29090034784956131 ) ) ;
#12310 = CARTESIAN_POINT ( 'NONE',  ( 8.728722367416583694, -2.516121109503213216, -1.500000000000001998 ) ) ;
#12311 = CARTESIAN_POINT ( 'NONE',  ( -34.55261918705283364, 19.75278628345992260, 31.10207979175319437 ) ) ;
#12312 = CARTESIAN_POINT ( 'NONE',  ( 0.000000000000000000, 0.000000000000000000, 1.500000000000001332 ) ) ;
#12313 = DIRECTION ( 'NONE',  ( -0.8412535328311884220, -0.5406408174555862312, 0.000000000000000000 ) ) ;
#12314 = VERTEX_POINT ( 'NONE', #8732 ) ;
#12315 = ADVANCED_FACE ( 'NONE', ( #28063 ), #27923, .F. ) ;
#12316 = CARTESIAN_POINT ( 'NONE',  ( -29.19944802842337950, 28.17413647968741586, 9.732408078920970596 ) ) ;
#12317 = EDGE_CURVE ( 'NONE', #8309, #25705, #20393, .T. ) ;
#12318 = CARTESIAN_POINT ( 'NONE',  ( -15.40257881337302592, 12.78582346615752741, 7.652108011868850035 ) ) ;
#12319 = AXIS2_PLACEMENT_3D ( 'NONE', #14612, #24114, #7447 ) ;
#12320 = DIRECTION ( 'NONE',  ( 1.000000000000000000, 0.000000000000000000, 0.000000000000000000 ) ) ;
#12321 = VERTEX_POINT ( 'NONE', #6547 ) ;
#12322 = SHAPE_REPRESENTATION ( 'Cam Ring Elliptical Outer Ring', ( #7396 ), #1419 ) ;
#12323 = ORIENTED_EDGE ( 'NONE', *, *, #1622, .T. ) ;
#12324 = CARTESIAN_POINT ( 'NONE',  ( 8.884323311075775109, 1.438332125858202692, 1.500000000000001332 ) ) ;
#12325 = CARTESIAN_POINT ( 'NONE',  ( 28.34828976096171971, 29.18752572968384129, 1.500000000000000000 ) ) ;
#12326 = AXIS2_PLACEMENT_3D ( 'NONE', #8134, #17016, #10151 ) ;
#12327 = CARTESIAN_POINT ( 'NONE',  ( -4.935065328765587012, 16.29835470421561539, 7.429667576816606278 ) ) ;
#12328 = DIRECTION ( 'NONE',  ( -0.000000000000000000, -0.000000000000000000, 1.000000000000000000 ) ) ;
#12329 = AXIS2_PLACEMENT_3D ( 'NONE', #29954, #18095, #27613 ) ;
#12330 = B_SPLINE_CURVE_WITH_KNOTS ( 'NONE', 3,
 ( #1452, #3312, #5970, #27030, #20000, #8618, #1287, #25300, #12841, #10966, #17661, #29985, #27642, #15467 ),
 .UNSPECIFIED., .F., .F.,
 ( 4, 2, 2, 2, 2, 2, 4 ),
 ( 2.111164903073641426E-07, 0.0004668847526555941377, 0.0009335583888208808965, 0.001400232024986167601, 0.001866905661151454414, 0.002800252933482019584, 0.003733600205812584970 ),
 .UNSPECIFIED. ) ;
#12331 = AXIS2_PLACEMENT_3D ( 'NONE', #16244, #15633, #4095 ) ;
#12332 = CARTESIAN_POINT ( 'NONE',  ( 4.950437002841800198E-16, 0.4400770685579611374, -9.000000000000005329 ) ) ;
#12333 = ORIENTED_EDGE ( 'NONE', *, *, #3267, .T. ) ;
#12334 = ORIENTED_EDGE ( 'NONE', *, *, #12446, .F. ) ;
#12335 = AXIS2_PLACEMENT_3D ( 'NONE', #608, #19631, #17936 ) ;
#12336 = CARTESIAN_POINT ( 'NONE',  ( -26.87942847751985909, -26.27672867733070206, 34.50000000000000711 ) ) ;
#12337 = CARTESIAN_POINT ( 'NONE',  ( -17.68050765791476309, -9.349252870402535720, 19.96797677718664588 ) ) ;
#12338 = CYLINDRICAL_SURFACE ( 'NONE', #10978, 11.46182693247435935 ) ;
#12339 = ORIENTED_EDGE ( 'NONE', *, *, #24020, .F. ) ;
#12340 = CARTESIAN_POINT ( 'NONE',  ( 15.49551216414738875, 12.67315350590407697, 7.080843742048788414 ) ) ;
#12341 = ORIENTED_EDGE ( 'NONE', *, *, #17186, .T. ) ;
#12342 = CIRCLE ( 'NONE', #15329, 9.482273699623480212 ) ;
#12343 = FACE_OUTER_BOUND ( 'NONE', #10304, .T. ) ;
#12344 = PRODUCT_DEFINITION_CONTEXT ( 'detailed design', #8789, 'design' ) ;
#12345 = CARTESIAN_POINT ( 'NONE',  ( -2.959227181723746547, 8.499586724479465616, 21.50000000000000000 ) ) ;
#12346 = CYLINDRICAL_SURFACE ( 'NONE', #1602, 3.559164065751841743 ) ;
#12347 = ORIENTED_EDGE ( 'NONE', *, *, #11681, .F. ) ;
#12348 = CARTESIAN_POINT ( 'NONE',  ( 4.866781629985560187, 19.41732998781225916, 5.749491821935610147 ) ) ;
#12349 = DIRECTION ( 'NONE',  ( -0.000000000000000000, -0.000000000000000000, 1.000000000000000000 ) ) ;
#12350 = PLANE ( 'NONE',  #6360 ) ;
#12351 = CARTESIAN_POINT ( 'NONE',  ( 0.000000000000000000, 87.00000000000001421, 59.49999999999999289 ) ) ;
#12352 = AXIS2_PLACEMENT_3D ( 'NONE', #905, #5733, #3092 ) ;
#12353 = CIRCLE ( 'NONE', #11858, 9.084132297865673777 ) ;
#12354 = CARTESIAN_POINT ( 'NONE',  ( -26.36764545593178255, -31.31467416275353344, -1.500000000000000000 ) ) ;
#12355 = CARTESIAN_POINT ( 'NONE',  ( 11.11118388262826784, -16.62953976291649028, 18.34798005863226678 ) ) ;
#12356 = ORIENTED_EDGE ( 'NONE', *, *, #1794, .T. ) ;
#12357 = DIRECTION ( 'NONE',  ( 1.000000000000000000, 0.000000000000000000, 0.000000000000000000 ) ) ;
#12358 = CARTESIAN_POINT ( 'NONE',  ( -2.687479362164884034, -44.39187623478217404, -19.50000000000000355 ) ) ;
#12359 = DIRECTION ( 'NONE',  ( 1.000000000000000000, 0.000000000000000000, 0.000000000000000000 ) ) ;
#12360 = VERTEX_POINT ( 'NONE', #16058 ) ;
#12361 = CARTESIAN_POINT ( 'NONE',  ( -17.96415918337694961, -8.831719996762313230, 20.32367522806703874 ) ) ;
#12362 = CARTESIAN_POINT ( 'NONE',  ( -40.00000000000000711, 87.00000000000001421, 62.49999999999999289 ) ) ;
#12363 = DIRECTION ( 'NONE',  ( -0.000000000000000000, -0.000000000000000000, 1.000000000000000000 ) ) ;
#12364 = DIRECTION ( 'NONE',  ( 1.000000000000000000, 0.000000000000000000, 0.000000000000000000 ) ) ;
#12365 = AXIS2_PLACEMENT_3D ( 'NONE', #6455, #10984, #11439 ) ;
#12366 = CARTESIAN_POINT ( 'NONE',  ( 37.98493438987956949, 11.12428508576150143, -1.500000000000000000 ) ) ;
#12367 = AXIS2_PLACEMENT_3D ( 'NONE', #22119, #17135, #10267 ) ;
#12368 = PLANE ( 'NONE',  #21426 ) ;
#12369 = CARTESIAN_POINT ( 'NONE',  ( 39.00438428794741696, -0.1180012993332143073, 32.23357027876486569 ) ) ;
#12370 = CARTESIAN_POINT ( 'NONE',  ( 4.510281037539698445E-13, -4.926614671774132148E-13, 57.49999999999999289 ) ) ;
#12371 = ORIENTED_EDGE ( 'NONE', *, *, #8253, .T. ) ;
#12372 = CARTESIAN_POINT ( 'NONE',  ( 5.069257791428381843, -7.538175180318440027, 21.50000000000000000 ) ) ;
#12374 = ORIENTED_EDGE ( 'NONE', *, *, #25434, .F. ) ;
#12373 = CIRCLE ( 'NONE', #18853, 50.00000000000000000 ) ;
#12375 = CARTESIAN_POINT ( 'NONE',  ( -70.00000000000000000, -70.00000000000000000, -92.50000000000000000 ) ) ;
#12376 = DIRECTION ( 'NONE',  ( -0.000000000000000000, -1.000000000000000000, -0.000000000000000000 ) ) ;
#12377 = ORIENTED_EDGE ( 'NONE', *, *, #23477, .T. ) ;
#12378 = EDGE_LOOP ( 'NONE', ( #1087, #7184 ) ) ;
#12379 = LINE ( 'NONE', #26886, #22231 ) ;
#12380 = ORIENTED_EDGE ( 'NONE', *, *, #80, .F. ) ;
#12381 = ORIENTED_EDGE ( 'NONE', *, *, #7688, .F. ) ;
#12382 = EDGE_LOOP ( 'NONE', ( #20283, #16351, #6839, #5736 ) ) ;
#12383 = DIRECTION ( 'NONE',  ( -0.000000000000000000, -0.000000000000000000, -1.000000000000000000 ) ) ;
#12384 =( GEOMETRIC_REPRESENTATION_CONTEXT ( 3 ) GLOBAL_UNCERTAINTY_ASSIGNED_CONTEXT ( ( #7980 ) ) GLOBAL_UNIT_ASSIGNED_CONTEXT ( ( #8840, #16619, #30809 ) ) REPRESENTATION_CONTEXT ( 'NONE', 'WORKASPACE' ) );
#12385 = CARTESIAN_POINT ( 'NONE',  ( -33.18055756306304716, 15.32856214772949599, 34.49999999999999289 ) ) ;
#12386 = DIRECTION ( 'NONE',  ( 1.000000000000000000, 0.000000000000000000, 0.000000000000000000 ) ) ;
#12387 = AXIS2_PLACEMENT_3D ( 'NONE', #70, #2720, #19554 ) ;
#12388 = CARTESIAN_POINT ( 'NONE',  ( 4.176140024798157491, 16.52246432927137931, 20.34789198813115618 ) ) ;
#12389 = DIRECTION ( 'NONE',  ( 1.000000000000000000, 0.000000000000000000, 0.000000000000000000 ) ) ;
#12390 = AXIS2_PLACEMENT_3D ( 'NONE', #27878, #24912, #13684 ) ;
#12391 = ORIENTED_EDGE ( 'NONE', *, *, #3877, .T. ) ;
#12392 = EDGE_CURVE ( 'NONE', #27888, #23760, #6691, .T. ) ;
#12393 = DIRECTION ( 'NONE',  ( 0.000000000000000000, 1.000000000000000000, -0.000000000000000000 ) ) ;
#12394 = CARTESIAN_POINT ( 'NONE',  ( 9.585801206154414444, -42.83572092346827276, -16.50000000000000355 ) ) ;
#12395 = CARTESIAN_POINT ( 'NONE',  ( 12.25310179107605002, 11.85582831497230138, 18.35718225375110180 ) ) ;
#12396 = FACE_BOUND ( 'NONE', #9665, .T. ) ;
#12397 = EDGE_LOOP ( 'NONE', ( #22881, #26359 ) ) ;
#12398 = PRODUCT_RELATED_PRODUCT_CATEGORY ( 'part', '', ( #14916 ) ) ;
#12399 = AXIS2_PLACEMENT_3D ( 'NONE', #17901, #27415, #6034 ) ;
#12400 = CARTESIAN_POINT ( 'NONE',  ( -8.550548368345314287, -14.74545326172986570, 20.34789198813115263 ) ) ;
#12401 = EDGE_CURVE ( 'NONE', #27073, #24015, #25720, .T. ) ;
#12402 = LINE ( 'NONE', #2574, #7307 ) ;
#12403 = CARTESIAN_POINT ( 'NONE',  ( -5.549075634136965363, 16.11684027513961226, 18.34798005863078885 ) ) ;
#12404 = CARTESIAN_POINT ( 'NONE',  ( -6.364020599487750118, 6.482337650448473099, 13.22130136205108819 ) ) ;
#12405 = DIRECTION ( 'NONE',  ( 0.000000000000000000, 0.000000000000000000, 1.000000000000000000 ) ) ;
#12406 = EDGE_CURVE ( 'NONE', #23519, #25108, #25407, .T. ) ;
#12407 = DIRECTION ( 'NONE',  ( 0.000000000000000000, 0.000000000000000000, 1.000000000000000000 ) ) ;
#12408 = VERTEX_POINT ( 'NONE', #17578 ) ;
#12409 = ORIENTED_EDGE ( 'NONE', *, *, #20863, .F. ) ;
#12410 = CYLINDRICAL_SURFACE ( 'NONE', #12458, 7.500000000000000000 ) ;
#12411 = CARTESIAN_POINT ( 'NONE',  ( -7.852931496087791174, -15.15760027743181482, 7.269896094239230777 ) ) ;
#12412 = DIRECTION ( 'NONE',  ( 1.000000000000000000, 0.000000000000000000, 0.000000000000000000 ) ) ;
#12413 = DIRECTION ( 'NONE',  ( 0.000000000000000000, 0.000000000000000000, 1.000000000000000000 ) ) ;
#12414 = ORIENTED_EDGE ( 'NONE', *, *, #7510, .F. ) ;
#12415 = SHAPE_DEFINITION_REPRESENTATION ( #14407, #13696 ) ;
#12416 = DIRECTION ( 'NONE',  ( 1.000000000000000000, 0.000000000000000000, 0.000000000000000000 ) ) ;
#12417 = CIRCLE ( 'NONE', #13429, 9.482273699623480212 ) ;
#12418 = CARTESIAN_POINT ( 'NONE',  ( -0.7220001660363114526, -9.454746441592957851, 13.00000000000000178 ) ) ;
#12419 = EDGE_CURVE ( 'NONE', #26519, #23441, #18045, .T. ) ;
#12420 = ORIENTED_EDGE ( 'NONE', *, *, #16800, .F. ) ;
#12421 = CARTESIAN_POINT ( 'NONE',  ( 5.517068924551619347, 19.24285362756905471, 18.36582235739946611 ) ) ;
#12422 = CARTESIAN_POINT ( 'NONE',  ( -37.16608720827707657, -36.86186943028246787, 97.07879600563551037 ) ) ;
#12423 = AXIS2_PLACEMENT_3D ( 'NONE', #4686, #14040, #6870 ) ;
#12424 = CARTESIAN_POINT ( 'NONE',  ( -7.785146467922785085, -15.19543897951832889, 18.84329447212443753 ) ) ;
#12425 = CARTESIAN_POINT ( 'NONE',  ( -30.71432649547681137, -21.52377453480933056, 37.50000000000097344 ) ) ;
#12426 = ORIENTED_EDGE ( 'NONE', *, *, #7245, .F. ) ;
#12427 = CARTESIAN_POINT ( 'NONE',  ( -24.03448224033878944, 8.660042335149839232, 49.47829057475703962 ) ) ;
#12428 = CARTESIAN_POINT ( 'NONE',  ( 12.35846533491530685, 11.73919094685904341, 20.34789198813115263 ) ) ;
#12429 = AXIS2_PLACEMENT_3D ( 'NONE', #11538, #25428, #2164 ) ;
#12430 = DIRECTION ( 'NONE',  ( -0.000000000000000000, -0.000000000000000000, 1.000000000000000000 ) ) ;
#12431 = B_SPLINE_CURVE_WITH_KNOTS ( 'NONE', 3,
 ( #28888, #24655, #492, #17646, #5790, #960, #786, #3290, #19984, #29033, #22006, #3455, #12972, #29502, #10155, #7670 ),
 .UNSPECIFIED., .F., .F.,
 ( 4, 2, 2, 2, 2, 2, 2, 4 ),
 ( 2.980374332565958659E-07, 0.0009280375596593484246, 0.001391907320772401216, 0.001855777081885454224, 0.002319646842998507232, 0.002783516604111560024, 0.003247386365224613249, 0.003711256126337666040 ),
 .UNSPECIFIED. ) ;
#12432 = CYLINDRICAL_SURFACE ( 'NONE', #6293, 10.00000000000000000 ) ;
#12433 = EDGE_LOOP ( 'NONE', ( #28910, #927, #29209, #26085 ) ) ;
#12434 = DIRECTION ( 'NONE',  ( -0.000000000000000000, -0.000000000000000000, 1.000000000000000000 ) ) ;
#12435 = DIRECTION ( 'NONE',  ( -0.000000000000000000, -0.000000000000000000, 1.000000000000000000 ) ) ;
#12436 = EDGE_CURVE ( 'NONE', #1600, #2106, #20525, .T. ) ;
#12437 = LINE ( 'NONE', #7593, #10734 ) ;
#12438 = ADVANCED_FACE ( 'NONE', ( #27560 ), #13950, .F. ) ;
#12439 = FACE_OUTER_BOUND ( 'NONE', #9333, .T. ) ;
#12440 = VECTOR ( 'NONE', #23942, 1000.000000000000000 ) ;
#12441 = CYLINDRICAL_SURFACE ( 'NONE', #11272, 6.000000000000005329 ) ;
#12442 = DIRECTION ( 'NONE',  ( 0.000000000000000000, 0.000000000000000000, 1.000000000000000000 ) ) ;
#12443 = DIRECTION ( 'NONE',  ( -0.000000000000000000, 1.000000000000000000, -0.000000000000000000 ) ) ;
#12444 = FACE_OUTER_BOUND ( 'NONE', #8686, .T. ) ;
#12445 = ORIENTED_EDGE ( 'NONE', *, *, #12460, .F. ) ;
#12446 = EDGE_CURVE ( 'NONE', #6231, #19990, #28898, .T. ) ;
#12447 = DIRECTION ( 'NONE',  ( -0.000000000000000000, -0.000000000000000000, -1.000000000000000000 ) ) ;
#12448 = VECTOR ( 'NONE', #10097, 1000.000000000000000 ) ;
#12449 = CARTESIAN_POINT ( 'NONE',  ( -2.523760598493569596, 1.621922452366830747, 24.50000000000000000 ) ) ;
#12450 = EDGE_LOOP ( 'NONE', ( #9778, #19065, #4267, #16734 ) ) ;
#12451 = ORIENTED_EDGE ( 'NONE', *, *, #5172, .F. ) ;
#12452 = EDGE_CURVE ( 'NONE', #9573, #228, #24742, .T. ) ;
#12453 = LINE ( 'NONE', #17579, #1684 ) ;
#12454 = ADVANCED_FACE ( 'NONE', ( #22865 ), #20673, .F. ) ;
#12455 = CARTESIAN_POINT ( 'NONE',  ( -15.00022444080144091, 47.69688948748883206, -55.48551676194295368 ) ) ;
#12456 = B_SPLINE_CURVE_WITH_KNOTS ( 'NONE', 3,
 ( #23558, #26217, #18744, #21213, #30743, #2204 ),
 .UNSPECIFIED., .F., .F.,
 ( 4, 2, 4 ),
 ( 0.009719890944573148991, 0.01235036185894307706, 0.01498083277331300339 ),
 .UNSPECIFIED. ) ;
#12457 = EDGE_LOOP ( 'NONE', ( #21825, #4123, #15349 ) ) ;
#12458 = AXIS2_PLACEMENT_3D ( 'NONE', #16762, #229, #21746 ) ;
#12459 = CARTESIAN_POINT ( 'NONE',  ( 12.87427757126085837, 11.14157019477620914, 18.71435384576123440 ) ) ;
#12460 = EDGE_CURVE ( 'NONE', #19119, #23409, #26405, .T. ) ;
#12461 = CARTESIAN_POINT ( 'NONE',  ( -11.37242378808260668, -16.47377160145866171, 6.755862304746362845 ) ) ;
#12462 = ORIENTED_EDGE ( 'NONE', *, *, #19927, .F. ) ;
#12463 = DIRECTION ( 'NONE',  ( 0.000000000000000000, 0.000000000000000000, -1.000000000000000000 ) ) ;
#12464 = CARTESIAN_POINT ( 'NONE',  ( 19.66622914841314440, 3.734651121118245154, 18.50655187082627862 ) ) ;
#12465 = PLANE ( 'NONE',  #14475 ) ;
#12466 = EDGE_LOOP ( 'NONE', ( #3481, #14392 ) ) ;
#12467 = CARTESIAN_POINT ( 'NONE',  ( -0.6210184355500071307, 9.062880100047296494, -1.500000000000000666 ) ) ;
#12468 = ORIENTED_EDGE ( 'NONE', *, *, #13038, .T. ) ;
#12469 = AXIS2_PLACEMENT_3D ( 'NONE', #6111, #29522, #15626 ) ;
#12470 = EDGE_LOOP ( 'NONE', ( #6555, #29439, #14514 ) ) ;
#12471 = EDGE_CURVE ( 'NONE', #1853, #27034, #5989, .T. ) ;
#12472 = EDGE_CURVE ( 'NONE', #886, #27348, #22896, .T. ) ;
#12473 = CARTESIAN_POINT ( 'NONE',  ( 7.628653938386951161, 41.77449438652679703, 28.90251124119662762 ) ) ;
#12474 = CARTESIAN_POINT ( 'NONE',  ( -6.842536740270960038, 18.81187820119070508, 19.79423548914561692 ) ) ;
#12475 = CARTESIAN_POINT ( 'NONE',  ( -14.79144470604038020, 13.48820156989937225, 18.80699882434806369 ) ) ;
#12476 = DIRECTION ( 'NONE',  ( -0.000000000000000000, -0.000000000000000000, 1.000000000000000000 ) ) ;
#12477 = CARTESIAN_POINT ( 'NONE',  ( -23.60134417525909001, -33.84107530290921062, 29.65494239027400525 ) ) ;
#12478 = DIRECTION ( 'NONE',  ( 0.000000000000000000, 0.000000000000000000, 1.000000000000000000 ) ) ;
#12479 = DIRECTION ( 'NONE',  ( -0.000000000000000000, 1.132880637372608986E-16, -1.000000000000000000 ) ) ;
#12480 = ORIENTED_EDGE ( 'NONE', *, *, #9543, .F. ) ;
#12481 = CARTESIAN_POINT ( 'NONE',  ( 10.26788185420488553, -17.18392197670719668, 6.530762810602277924 ) ) ;
#12482 = CARTESIAN_POINT ( 'NONE',  ( -28.22318188663881600, 29.33129562425243009, 14.53116935034356061 ) ) ;
#12483 = CARTESIAN_POINT ( 'NONE',  ( 19.76377475971901632, 3.067715173639373294, 5.651480102388687143 ) ) ;
#12484 = ORIENTED_EDGE ( 'NONE', *, *, #5236, .F. ) ;
#12485 = VERTEX_POINT ( 'NONE', #27708 ) ;
#12486 = CARTESIAN_POINT ( 'NONE',  ( -35.41742430504425698, 80.00000000000001421, 50.49999999999998579 ) ) ;
#12487 = CARTESIAN_POINT ( 'NONE',  ( 43.34097750826426676, -11.89502811014148698, 1.500000000000000444 ) ) ;
#12488 = DIRECTION ( 'NONE',  ( 0.000000000000000000, 0.000000000000000000, 1.000000000000000000 ) ) ;
#12489 = CARTESIAN_POINT ( 'NONE',  ( -15.16307827826492627, -7.786259562520722710, 5.652196082368482699 ) ) ;
#12490 = AXIS2_PLACEMENT_3D ( 'NONE', #2784, #8232, #29601 ) ;
#12491 = FACE_OUTER_BOUND ( 'NONE', #10740, .T. ) ;
#12492 = CARTESIAN_POINT ( 'NONE',  ( 5.549407557472018304, 19.21507098571442995, 7.626647697317578078 ) ) ;
#12493 = ORIENTED_EDGE ( 'NONE', *, *, #20040, .T. ) ;
#12494 = DIRECTION ( 'NONE',  ( 0.000000000000000000, 0.000000000000000000, 1.000000000000000000 ) ) ;
#12495 = CYLINDRICAL_SURFACE ( 'NONE', #21159, 20.00000000000000000 ) ;
#12496 = CARTESIAN_POINT ( 'NONE',  ( 16.77777292147014876, 2.975267875541940832, 5.670038381137163519 ) ) ;
#12497 = EDGE_LOOP ( 'NONE', ( #11110, #14403, #22918, #19652 ) ) ;
#12498 = PLANE ( 'NONE',  #14311 ) ;
#12499 = VERTEX_POINT ( 'NONE', #10870 ) ;
#12500 = EDGE_CURVE ( 'NONE', #25827, #26330, #27096, .T. ) ;
#12501 = CARTESIAN_POINT ( 'NONE',  ( 8.860628911697515875, 8.184276679720483116, 1.500000000000000000 ) ) ;
#12502 = ADVANCED_FACE ( 'NONE', ( #25371, #27246, #8382, #4001, #20069, #23009 ), #15213, .T. ) ;
#12503 = DIRECTION ( 'NONE',  ( 1.000000000000000000, 0.000000000000000000, 0.000000000000000000 ) ) ;
#12504 = DIRECTION ( 'NONE',  ( 1.000000000000000000, 0.000000000000000000, 0.000000000000000000 ) ) ;
#12505 = ORIENTED_EDGE ( 'NONE', *, *, #8876, .T. ) ;
#12506 = CYLINDRICAL_SURFACE ( 'NONE', #26761, 1.000000000000000888 ) ;
#12507 = CIRCLE ( 'NONE', #11013, 7.500000000000013323 ) ;
#12508 = CARTESIAN_POINT ( 'NONE',  ( -4.163336342344337027E-14, -1.387778780781445676E-14, -1.500000000000000000 ) ) ;
#12509 = DIRECTION ( 'NONE',  ( -0.2817325568414293380, -0.9594929736144974797, 0.000000000000000000 ) ) ;
#12510 = CARTESIAN_POINT ( 'NONE',  ( 25.22106791543724924, 28.20183085419529334, 34.49999999999999289 ) ) ;
#12511 = CIRCLE ( 'NONE', #16483, 9.084132297865673777 ) ;
#12512 =( BOUNDED_SURFACE ( )  B_SPLINE_SURFACE ( 3, 1, ( 
 ( #3248, #14953 ),
 ( #8101, #12628 ),
 ( #22118, #745 ),
 ( #10265, #12774 ) ),
 .UNSPECIFIED., .F., .F., .F. ) 
 B_SPLINE_SURFACE_WITH_KNOTS ( ( 4, 4 ),
 ( 2, 2 ),
 ( 0.000000000000000000, 1.000000000000000000 ),
 ( 0.000000000000000000, 1.000000000000000000 ),
 .UNSPECIFIED. ) 
 GEOMETRIC_REPRESENTATION_ITEM ( )  RATIONAL_B_SPLINE_SURFACE ( (
 ( 1.000000000000000000, 1.000000000000000000),
 ( 0.3333333333333333703, 0.3333333333333333703),
 ( 0.3333333333333333703, 0.3333333333333333703),
 ( 1.000000000000000000, 1.000000000000000000) ) ) 
 REPRESENTATION_ITEM ( '' )  SURFACE ( )  );
#12513 = CARTESIAN_POINT ( 'NONE',  ( 0.000000000000000000, 0.000000000000000000, 21.50000000000000000 ) ) ;
#12514 = DIRECTION ( 'NONE',  ( 0.000000000000000000, -0.5000000000000012212, 0.8660254037844380415 ) ) ;
#12515 = CARTESIAN_POINT ( 'NONE',  ( 10.27753383451899261, -17.15735655630020773, 19.08232364404840808 ) ) ;
#12516 = VERTEX_POINT ( 'NONE', #17722 ) ;
#12517 = DIRECTION ( 'NONE',  ( 1.000000000000000000, 0.000000000000000000, -0.000000000000000000 ) ) ;
#12518 = CARTESIAN_POINT ( 'NONE',  ( -34.07766914599911701, 21.40380666528009002, -1.500000000000000000 ) ) ;
#12519 = DIRECTION ( 'NONE',  ( -0.000000000000000000, -0.000000000000000000, 1.000000000000000000 ) ) ;
#12520 = CARTESIAN_POINT ( 'NONE',  ( 29.41946586498233529, -27.90099047827807510, 9.493481885648451524 ) ) ;
#12521 = FACE_OUTER_BOUND ( 'NONE', #329, .T. ) ;
#12522 = DIRECTION ( 'NONE',  ( -1.000000000000000000, 0.000000000000000000, 0.000000000000000000 ) ) ;
#12523 = FACE_OUTER_BOUND ( 'NONE', #3202, .T. ) ;
#12524 = CARTESIAN_POINT ( 'NONE',  ( 31.18700685317022803, -26.11823559933272421, -1.500000000000000000 ) ) ;
#12525 = LINE ( 'NONE', #29047, #19946 ) ;
#12526 = CARTESIAN_POINT ( 'NONE',  ( 16.81773250897607141, 2.696729702855183763, 5.774779864094944593 ) ) ;
#12527 = DIRECTION ( 'NONE',  ( 0.000000000000000000, -0.000000000000000000, -1.000000000000000000 ) ) ;
#12528 = ORIENTED_EDGE ( 'NONE', *, *, #7287, .F. ) ;
#12529 = VECTOR ( 'NONE', #25471, 1000.000000000000000 ) ;
#12530 = DIRECTION ( 'NONE',  ( -9.830099697201897928E-15, 1.000000000000000000, 0.000000000000000000 ) ) ;
#12531 = ORIENTED_EDGE ( 'NONE', *, *, #4260, .T. ) ;
#12532 = B_SPLINE_CURVE_WITH_KNOTS ( 'NONE', 3,
 ( #21423, #12388, #23917, #24064, #9884, #26104, #2715, #9432, #21256, #21889, #21573, #24215, #14567, #4734, #19551, #19401, #29067, #7711, #28919, #209 ),
 .UNSPECIFIED., .F., .F.,
 ( 4, 2, 2, 2, 2, 2, 2, 2, 2, 4 ),
 ( 0.000000000000000000, 0.06250000000000170697, 0.1250000000000034139, 0.1875000000000051070, 0.2187500000000052736, 0.2500000000000054401, 0.3125000000000041078, 0.3750000000000027200, 0.4375000000000013878, 0.5000000000000000000 ),
 .UNSPECIFIED. ) ;
#12533 = CARTESIAN_POINT ( 'NONE',  ( 0.000000000000000000, 0.000000000000000000, 1.500000000000000000 ) ) ;
#12534 = CARTESIAN_POINT ( 'NONE',  ( -43.34097750826426676, 11.89502811014148698, -1.500000000000000444 ) ) ;
#12535 = ORIENTED_EDGE ( 'NONE', *, *, #18370, .F. ) ;
#12536 = VERTEX_POINT ( 'NONE', #22409 ) ;
#12537 = CARTESIAN_POINT ( 'NONE',  ( -40.00000000000000000, 87.00000000000001421, 22.49999999999999289 ) ) ;
#12538 = ADVANCED_FACE ( 'NONE', ( #5879 ), #15382, .F. ) ;
#12539 = ORIENTED_EDGE ( 'NONE', *, *, #5452, .T. ) ;
#12540 = ORIENTED_EDGE ( 'NONE', *, *, #412, .T. ) ;
#12541 = CARTESIAN_POINT ( 'NONE',  ( -27.03074382657074182, -6.449748410230987439, 47.21042702067970964 ) ) ;
#12542 = ADVANCED_FACE ( 'NONE', ( #1206 ), #10708, .T. ) ;
#12543 = FACE_OUTER_BOUND ( 'NONE', #19998, .T. ) ;
#12544 = VECTOR ( 'NONE', #18533, 1000.000000000000227 ) ;
#12545 = CARTESIAN_POINT ( 'NONE',  ( -6.812559277181930106, 5.881244434206302607, -3.621320343559650379 ) ) ;
#12546 = LINE ( 'NONE', #10653, #3400 ) ;
#12547 = CARTESIAN_POINT ( 'NONE',  ( -15.57266529552203416, -38.96488032230103471, 1.500000000000000000 ) ) ;
#12548 = ORIENTED_EDGE ( 'NONE', *, *, #22496, .F. ) ;
#12549 = FACE_OUTER_BOUND ( 'NONE', #4346, .T. ) ;
#12550 = CARTESIAN_POINT ( 'NONE',  ( -6.224883619896829146, -5.687793815610328707, -1.500000000000002220 ) ) ;
#12551 = CARTESIAN_POINT ( 'NONE',  ( 14.89737979318874928, 13.37085219355980747, 20.34789198813115263 ) ) ;
#12552 = DIRECTION ( 'NONE',  ( -0.000000000000000000, -0.000000000000000000, -1.000000000000000000 ) ) ;
#12553 = ORIENTED_EDGE ( 'NONE', *, *, #6125, .F. ) ;
#12554 = AXIS2_PLACEMENT_3D ( 'NONE', #30655, #6972, #24719 ) ;
#12555 = DIRECTION ( 'NONE',  ( 0.000000000000000000, 0.000000000000000000, -1.000000000000000000 ) ) ;
#12556 = CARTESIAN_POINT ( 'NONE',  ( -15.13023987665973458, -7.854877310202119212, 5.652605728828375753 ) ) ;
#12557 = CARTESIAN_POINT ( 'NONE',  ( -9.169883732660077058, -9.268939115642981008, 24.50000000000000000 ) ) ;
#12558 = CARTESIAN_POINT ( 'NONE',  ( -15.57266529552203416, -38.96488032230103471, -1.500000000000000000 ) ) ;
#12559 = DIRECTION ( 'NONE',  ( -0.000000000000000000, -0.000000000000000000, 1.000000000000000000 ) ) ;
#12560 = VERTEX_POINT ( 'NONE', #27871 ) ;
#12561 = VERTEX_POINT ( 'NONE', #25977 ) ;
#12562 = DIRECTION ( 'NONE',  ( -0.000000000000000000, -0.000000000000000000, -1.000000000000000000 ) ) ;
#12563 = CARTESIAN_POINT ( 'NONE',  ( -8.550548372801092256, -14.74545326687210611, 7.652108011868850923 ) ) ;
#12564 = CARTESIAN_POINT ( 'NONE',  ( -14.99868389510897160, 13.25752457422374775, 7.500898271101006820 ) ) ;
#12566 = AXIS2_PLACEMENT_3D ( 'NONE', #16882, #15247, #14384 ) ;
#12565 = LINE ( 'NONE', #693, #21606 ) ;
#12567 = VERTEX_POINT ( 'NONE', #25673 ) ;
#12568 = APPLICATION_PROTOCOL_DEFINITION ( 'draft international standard', 'automotive_design', 1998, #2417 ) ;
#12569 = CARTESIAN_POINT ( 'NONE',  ( 15.67696945782692097, -6.669264855739880815, 18.39701043959520987 ) ) ;
#12570 = CARTESIAN_POINT ( 'NONE',  ( 5.881244434206234217, 6.812559277181991391, -3.621320343559650379 ) ) ;
#12571 = B_SPLINE_CURVE_WITH_KNOTS ( 'NONE', 3,
 ( #27664, #8783, #27973, #18614, #18309, #30454 ),
 .UNSPECIFIED., .F., .F.,
 ( 4, 2, 4 ),
 ( 2.380730968223702541E-07, 0.002629065763328367403, 0.005257893453559912313 ),
 .UNSPECIFIED. ) ;
#12572 = VERTEX_POINT ( 'NONE', #2426 ) ;
#12573 = LINE ( 'NONE', #701, #4832 ) ;
#12574 = DIRECTION ( 'NONE',  ( 0.000000000000000000, 0.000000000000000000, 1.000000000000000000 ) ) ;
#12575 = AXIS2_PLACEMENT_3D ( 'NONE', #5160, #3719, #320 ) ;
#12576 = CARTESIAN_POINT ( 'NONE',  ( 0.01899995639454664029, -7.352259170992735626, 5.265513565426390485 ) ) ;
#12577 = CARTESIAN_POINT ( 'NONE',  ( -21.73953648291186269, -30.57930865885014882, 37.49999999997677236 ) ) ;
#12578 = ORIENTED_EDGE ( 'NONE', *, *, #29610, .F. ) ;
#12579 = CARTESIAN_POINT ( 'NONE',  ( -28.34828976096172681, -29.18752572968383419, -1.500000000000000000 ) ) ;
#12580 = EDGE_CURVE ( 'NONE', #9872, #23362, #13467, .T. ) ;
#12581 = CARTESIAN_POINT ( 'NONE',  ( -5.729465025513086419E-13, 44.07656359094158915, -16.50000000000000000 ) ) ;
#12582 = CARTESIAN_POINT ( 'NONE',  ( -19.69217677393683630, 3.495450461901489447, 19.47728749465737863 ) ) ;
#12583 = VERTEX_POINT ( 'NONE', #18811 ) ;
#12584 =( REPRESENTATION_RELATIONSHIP ('NONE','NONE', #19885, #20057 ) REPRESENTATION_RELATIONSHIP_WITH_TRANSFORMATION ( #9068 )SHAPE_REPRESENTATION_RELATIONSHIP( ) );
#12585 = DIRECTION ( 'NONE',  ( -0.000000000000000000, -0.000000000000000000, -1.000000000000000000 ) ) ;
#12586 = FACE_OUTER_BOUND ( 'NONE', #28498, .T. ) ;
#12587 = CARTESIAN_POINT ( 'NONE',  ( 15.81416692036122917, -6.360574302898113430, 5.652196082368483587 ) ) ;
#12588 = VECTOR ( 'NONE', #14430, 1000.000000000000000 ) ;
#12589 = LINE ( 'NONE', #8209, #8310 ) ;
#12590 = FACE_OUTER_BOUND ( 'NONE', #18427, .T. ) ;
#12591 = DIRECTION ( 'NONE',  ( 0.000000000000000000, -0.000000000000000000, -1.000000000000000000 ) ) ;
#12592 = CARTESIAN_POINT ( 'NONE',  ( 37.98801336486642555, -9.618861032953940793, 13.08357279190622791 ) ) ;
#12593 = DIRECTION ( 'NONE',  ( 0.000000000000000000, -1.132880637372608986E-16, 1.000000000000000000 ) ) ;
#12594 = ORIENTED_EDGE ( 'NONE', *, *, #11311, .T. ) ;
#12595 = FACE_OUTER_BOUND ( 'NONE', #18334, .T. ) ;
#12596 = CYLINDRICAL_SURFACE ( 'NONE', #5117, 20.00000000000000355 ) ;
#12597 = ORIENTED_EDGE ( 'NONE', *, *, #20998, .F. ) ;
#12598 = ORIENTED_EDGE ( 'NONE', *, *, #22737, .F. ) ;
#12599 = DIRECTION ( 'NONE',  ( -0.000000000000000000, 0.000000000000000000, 1.000000000000000000 ) ) ;
#12600 = DIRECTION ( 'NONE',  ( 0.000000000000000000, -0.000000000000000000, -1.000000000000000000 ) ) ;
#12601 = EDGE_LOOP ( 'NONE', ( #11353, #5683 ) ) ;
#12602 = EDGE_CURVE ( 'NONE', #20557, #16079, #16157, .T. ) ;
#12603 = CARTESIAN_POINT ( 'NONE',  ( -34.24107012425980656, -12.20860444836018388, 27.50000000000000355 ) ) ;
#12604 = CARTESIAN_POINT ( 'NONE',  ( 15.18428249823343990, 13.04421712177833648, 18.44501272782439827 ) ) ;
#12605 = AXIS2_PLACEMENT_3D ( 'NONE', #17600, #18220, #20092 ) ;
#12606 = EDGE_CURVE ( 'NONE', #12720, #19956, #20969, .T. ) ;
#12607 = ORIENTED_EDGE ( 'NONE', *, *, #3704, .F. ) ;
#12608 = VECTOR ( 'NONE', #8182, 1000.000000000000000 ) ;
#12609 = CARTESIAN_POINT ( 'NONE',  ( -16.82187727961404278, 2.603938281378752162, 6.974106381145714018 ) ) ;
#12610 = CARTESIAN_POINT ( 'NONE',  ( 16.60164139905474201, 3.971857776421114483, 19.97651184436794125 ) ) ;
#12611 = EDGE_CURVE ( 'NONE', #8309, #27352, #2985, .T. ) ;
#12612 = DIRECTION ( 'NONE',  ( 2.312964634635743450E-15, 1.000000000000000000, 0.000000000000000000 ) ) ;
#12613 = ORIENTED_EDGE ( 'NONE', *, *, #12681, .T. ) ;
#12614 = DIRECTION ( 'NONE',  ( 1.000000000000000000, -2.396195514597832977E-15, 0.000000000000000000 ) ) ;
#12615 = ADVANCED_FACE ( 'NONE', ( #4606 ), #3986, .T. ) ;
#12616 = CARTESIAN_POINT ( 'NONE',  ( 16.55859027208438405, 35.07752759152815258, 27.50000000000000355 ) ) ;
#12617 = EDGE_LOOP ( 'NONE', ( #24318, #13132, #23982 ) ) ;
#12618 = EDGE_CURVE ( 'NONE', #25532, #21023, #9452, .T. ) ;
#12619 = CARTESIAN_POINT ( 'NONE',  ( 38.44330510386382826, -7.601442456462468300, 32.05526165865716592 ) ) ;
#12620 = B_SPLINE_SURFACE_WITH_KNOTS ( 'NONE', 3, 1, ( 
 ( #19004, #9793 ),
 ( #5112, #21016 ),
 ( #2300, #4796 ),
 ( #30539, #30683 ),
 ( #6992, #26167 ),
 ( #11825, #21326 ),
 ( #14302, #5431 ),
 ( #435, #577 ),
 ( #26639, #2941 ),
 ( #9952, #3231 ),
 ( #10415, #10094 ),
 ( #21947, #19760 ),
 ( #26805, #17584 ),
 ( #19931, #5266 ),
 ( #27253, #19458 ),
 ( #29595, #12753 ),
 ( #3085, #3392 ),
 ( #24443, #14773 ),
 ( #19609, #14934 ),
 ( #7764, #27102 ),
 ( #29289, #12459 ),
 ( #15075, #8227 ),
 ( #29129, #22257 ),
 ( #28975, #12920 ),
 ( #12604, #24292 ),
 ( #17272, #22097 ),
 ( #728, #5723 ),
 ( #895, #7608 ),
 ( #24591, #17728 ),
 ( #10245, #29445 ),
 ( #17116, #7933 ) ),
 .UNSPECIFIED., .F., .F., .F.,
 ( 4, 3, 3, 3, 3, 3, 3, 3, 3, 3, 4 ),
 ( 2, 2 ),
 ( 0.000000000000000000, 0.05425176834609614362, 0.1085332949128348518, 0.1623767749169379715, 0.2157504826133058717, 0.2688657508888169789, 0.3218907763505471364, 0.3749548578363334772, 0.4282048033836237666, 0.4818374082110496448, 0.4999999999131653494 ),
 ( 0.000000000000000000, 1.000000000000000000 ),
 .UNSPECIFIED. ) ;
#12621 = CARTESIAN_POINT ( 'NONE',  ( -6.290842788517063688, 19.00387417064636608, 20.29915277494337644 ) ) ;
#12622 = CARTESIAN_POINT ( 'NONE',  ( -14.70379955820389206, 13.58362208154139772, 19.56050940960062690 ) ) ;
#12623 = ADVANCED_FACE ( 'NONE', ( #30493 ), #2257, .F. ) ;
#12624 = CARTESIAN_POINT ( 'NONE',  ( 9.185733585337910512, -2.352830851074146246, 13.00000000000000178 ) ) ;
#12625 = EDGE_CURVE ( 'NONE', #27915, #20124, #23324, .T. ) ;
#12626 = CARTESIAN_POINT ( 'NONE',  ( -35.09604417355253503, 18.57963138642829293, 31.21515930947347428 ) ) ;
#12627 = CIRCLE ( 'NONE', #4134, 9.482273699623480212 ) ;
#12628 = CARTESIAN_POINT ( 'NONE',  ( 77.99999999999998579, -42.50000000000002132, 27.50000000000000711 ) ) ;
#12629 = CYLINDRICAL_SURFACE ( 'NONE', #5886, 9.084132297865673777 ) ;
#12630 = VERTEX_POINT ( 'NONE', #9134 ) ;
#12631 = CIRCLE ( 'NONE', #30055, 9.482273699623480212 ) ;
#12632 = CARTESIAN_POINT ( 'NONE',  ( -17.00515754968434479, 1.312003563659741134, 5.704143890883081269 ) ) ;
#12633 = CARTESIAN_POINT ( 'NONE',  ( 33.18263104983779499, -15.34882887482265090, 34.49999999999998579 ) ) ;
#12634 = CARTESIAN_POINT ( 'NONE',  ( -3.662523238938586001, -12.47340865698848056, 24.50000000000000000 ) ) ;
#12635 = ORIENTED_EDGE ( 'NONE', *, *, #7510, .T. ) ;
#12636 = VERTEX_POINT ( 'NONE', #8834 ) ;
#12637 = CARTESIAN_POINT ( 'NONE',  ( 28.34828976096172681, -29.18752572968383419, 1.500000000000000000 ) ) ;
#12638 = LINE ( 'NONE', #469, #1183 ) ;
#12639 = DIRECTION ( 'NONE',  ( 0.000000000000000000, 0.000000000000000000, 1.000000000000000000 ) ) ;
#12640 = EDGE_LOOP ( 'NONE', ( #15903, #16998, #15381, #26816 ) ) ;
#12641 = DIRECTION ( 'NONE',  ( 1.000000000000000000, 0.000000000000000000, 0.000000000000000000 ) ) ;
#12642 = DIRECTION ( 'NONE',  ( -0.000000000000000000, -0.000000000000000000, 1.000000000000000000 ) ) ;
#12643 = EDGE_CURVE ( 'NONE', #4157, #3062, #16612, .T. ) ;
#12644 = DIRECTION ( 'NONE',  ( -0.000000000000000000, -0.000000000000000000, -1.000000000000000000 ) ) ;
#12645 = ORIENTED_EDGE ( 'NONE', *, *, #22971, .T. ) ;
#12646 = EDGE_CURVE ( 'NONE', #3764, #14781, #6954, .T. ) ;
#12647 = VECTOR ( 'NONE', #13810, 1000.000000000000000 ) ;
#12648 = CARTESIAN_POINT ( 'NONE',  ( -9.748913725731210178, -17.46314199939011047, 18.84486140012299060 ) ) ;
#12649 = CYLINDRICAL_SURFACE ( 'NONE', #13232, 1.000000000000004441 ) ;
#12650 = EDGE_CURVE ( 'NONE', #26027, #15172, #21120, .T. ) ;
#12651 = CARTESIAN_POINT ( 'NONE',  ( 19.88727842228974652, 2.283828795636142495, 7.080843742048788414 ) ) ;
#12652 = ORIENTED_EDGE ( 'NONE', *, *, #7691, .F. ) ;
#12653 = CARTESIAN_POINT ( 'NONE',  ( 15.42025756663164948, 12.76459690492384702, 7.272049892295485485 ) ) ;
#12654 = VECTOR ( 'NONE', #27447, 1000.000000000000000 ) ;
#12655 = VERTEX_POINT ( 'NONE', #4753 ) ;
#12656 = CARTESIAN_POINT ( 'NONE',  ( 18.43859109590531276, -7.792859017390147969, 7.627891251804737927 ) ) ;
#12657 = EDGE_CURVE ( 'NONE', #8571, #3296, #9406, .T. ) ;
#12658 = LINE ( 'NONE', #775, #27852 ) ;
#12659 = CARTESIAN_POINT ( 'NONE',  ( -25.07174449839133601, 6.739288358966158299, 44.79593483594015169 ) ) ;
#12660 = ORIENTED_EDGE ( 'NONE', *, *, #29964, .F. ) ;
#12661 = ADVANCED_FACE ( 'NONE', ( #6789 ), #13678, .F. ) ;
#12662 = CARTESIAN_POINT ( 'NONE',  ( 0.8038475772931101826, -5.196152422707025487, -9.000000000000000000 ) ) ;
#12663 = CARTESIAN_POINT ( 'NONE',  ( -12.54846374865995706, -9.550116103605041928, 1.500000000000001332 ) ) ;
#12664 = EDGE_LOOP ( 'NONE', ( #18550, #25345, #4730, #27220, #3873, #16981 ) ) ;
#12665 = CARTESIAN_POINT ( 'NONE',  ( 10.02323409478514726, 38.00094089691386046, 34.49999999999999289 ) ) ;
#12666 = CYLINDRICAL_SURFACE ( 'NONE', #19861, 1.447898107987198646 ) ;
#12667 = CARTESIAN_POINT ( 'NONE',  ( -23.17581250239728519, -34.50630206824672541, -1.499999999999999778 ) ) ;
#12668 = CARTESIAN_POINT ( 'NONE',  ( 10.89102995336899582, -16.77499580993352879, 18.37250658438899009 ) ) ;
#12669 = VERTEX_POINT ( 'NONE', #2108 ) ;
#12670 = CARTESIAN_POINT ( 'NONE',  ( -25.41654339919794836, -6.509636863629522097, 48.76343458312125279 ) ) ;
#12671 = CARTESIAN_POINT ( 'NONE',  ( -15.97838715008244748, 12.05808207567199197, 19.14333282897057842 ) ) ;
#12672 = CARTESIAN_POINT ( 'NONE',  ( -4.163336342344337027E-14, 1.387778780781445676E-14, 52.50000000000000000 ) ) ;
#12673 = EDGE_LOOP ( 'NONE', ( #21341, #28278 ) ) ;
#12674 = AXIS2_PLACEMENT_3D ( 'NONE', #15154, #27493, #15624 ) ;
#12675 = AXIS2_PLACEMENT_3D ( 'NONE', #27294, #12952, #5924 ) ;
#12676 = CARTESIAN_POINT ( 'NONE',  ( 29.91322502737726552, -27.27054877340401973, 9.054183611633645157 ) ) ;
#12677 = DIRECTION ( 'NONE',  ( 1.000000000000000000, 5.125319360840571077E-16, -0.000000000000000000 ) ) ;
#12678 = EDGE_CURVE ( 'NONE', #19313, #20257, #25829, .T. ) ;
#12679 = DIRECTION ( 'NONE',  ( 0.000000000000000000, 0.000000000000000000, -1.000000000000000000 ) ) ;
#12680 = CARTESIAN_POINT ( 'NONE',  ( 7.500000000000000000, 4.336808689942017736E-15, -17.99999999999998224 ) ) ;
#12681 = EDGE_CURVE ( 'NONE', #17738, #946, #23937, .T. ) ;
#12682 = CARTESIAN_POINT ( 'NONE',  ( 4.336808689942017736E-16, 42.50000000000000000, -1.500000000000000000 ) ) ;
#12683 = DIRECTION ( 'NONE',  ( -0.000000000000000000, -0.000000000000000000, -1.000000000000000000 ) ) ;
#12684 = CARTESIAN_POINT ( 'NONE',  ( 16.76419345869466326, 3.064929150614125408, 7.652108011868850035 ) ) ;
#12685 = CARTESIAN_POINT ( 'NONE',  ( 19.69872561633593477, 3.460482060625765133, 5.679672709359371297 ) ) ;
#12686 = EDGE_LOOP ( 'NONE', ( #13571, #15038, #7121, #17770 ) ) ;
#12687 = FACE_OUTER_BOUND ( 'NONE', #24807, .T. ) ;
#12688 = CARTESIAN_POINT ( 'NONE',  ( -33.03678684150562361, -25.60268807474236752, -16.50000000000000000 ) ) ;
#12689 = DIRECTION ( 'NONE',  ( -0.000000000000000000, -0.000000000000000000, -1.000000000000000000 ) ) ;
#12690 = ORIENTED_EDGE ( 'NONE', *, *, #22911, .T. ) ;
#12691 = ORIENTED_EDGE ( 'NONE', *, *, #18157, .T. ) ;
#12692 = FACE_OUTER_BOUND ( 'NONE', #14819, .T. ) ;
#12693 = ORIENTED_EDGE ( 'NONE', *, *, #27295, .T. ) ;
#12694 = PRODUCT_DEFINITION_SHAPE ( 'NONE', 'NONE',  #18311 ) ;
#12695 = EDGE_LOOP ( 'NONE', ( #10147, #11039, #6694, #21440 ) ) ;
#12696 = LINE ( 'NONE', #2666, #7906 ) ;
#12697 = VECTOR ( 'NONE', #14470, 1000.000000000000227 ) ;
#12698 = CARTESIAN_POINT ( 'NONE',  ( -28.99877614713496499, 23.42512202833223256, 34.50000000000000711 ) ) ;
#12699 = CARTESIAN_POINT ( 'NONE',  ( -30.31220697679117393, 11.23460505553742550, -1.500000000000000000 ) ) ;
#12700 = FACE_OUTER_BOUND ( 'NONE', #9294, .T. ) ;
#12701 = CARTESIAN_POINT ( 'NONE',  ( -8.817355867515827228, -2.185336383880175593, 13.22130136205108819 ) ) ;
#12702 = ORIENTED_EDGE ( 'NONE', *, *, #6331, .T. ) ;
#12703 = DIRECTION ( 'NONE',  ( 1.000000000000000000, 0.000000000000000000, 0.000000000000000000 ) ) ;
#12704 = FACE_OUTER_BOUND ( 'NONE', #17436, .T. ) ;
#12705 = PRESENTATION_STYLE_ASSIGNMENT (( #19702 ) ) ;
#12706 = DIRECTION ( 'NONE',  ( -0.000000000000000000, 1.000000000000000000, -0.000000000000000000 ) ) ;
#12707 = ORIENTED_EDGE ( 'NONE', *, *, #13569, .T. ) ;
#12708 = CARTESIAN_POINT ( 'NONE',  ( -17.82234029294485111, -9.114408740892772087, 7.500147780736496017 ) ) ;
#12709 = FACE_OUTER_BOUND ( 'NONE', #5505, .T. ) ;
#12710 = CARTESIAN_POINT ( 'NONE',  ( 11.92709382895865389, -16.07640909887372516, 6.892848776733236704 ) ) ;
#12711 = CARTESIAN_POINT ( 'NONE',  ( -20.65888525914364493, -38.75220717792906555, -19.50000000000000355 ) ) ;
#12712 = DIRECTION ( 'NONE',  ( -0.000000000000000000, 0.000000000000000000, 1.000000000000000000 ) ) ;
#12713 = ORIENTED_EDGE ( 'NONE', *, *, #4434, .T. ) ;
#12714 = ORIENTED_EDGE ( 'NONE', *, *, #2134, .T. ) ;
#12715 =( LENGTH_UNIT ( ) NAMED_UNIT ( * ) SI_UNIT ( .MILLI., .METRE. ) );
#12716 = AXIS2_PLACEMENT_3D ( 'NONE', #25378, #8548, #20838 ) ;
#12717 = CARTESIAN_POINT ( 'NONE',  ( -5.485816626893757153, 19.23332246807784074, 20.22277707861862694 ) ) ;
#12718 = CARTESIAN_POINT ( 'NONE',  ( -12.74837729798237618, 11.28012212083751287, 6.310736198168394928 ) ) ;
#12719 = PLANE ( 'NONE',  #13660 ) ;
#12720 = VERTEX_POINT ( 'NONE', #17075 ) ;
#12721 = SHAPE_DEFINITION_REPRESENTATION ( #12694, #19885 ) ;
#12722 = CARTESIAN_POINT ( 'NONE',  ( 18.30707599941031560, -8.097116190180058126, 18.35377592296120497 ) ) ;
#12723 = LINE ( 'NONE', #24710, #5228 ) ;
#12724 = ORIENTED_EDGE ( 'NONE', *, *, #25792, .F. ) ;
#12725 = CARTESIAN_POINT ( 'NONE',  ( 5.818449564404028607, 19.15386117387415865, 18.49267272388512140 ) ) ;
#12726 = DIRECTION ( 'NONE',  ( 0.000000000000000000, -0.000000000000000000, 1.000000000000000000 ) ) ;
#12727 = CARTESIAN_POINT ( 'NONE',  ( -7.322557715923444732, 14.41080185948837311, 1.500000000000000000 ) ) ;
#12728 = CARTESIAN_POINT ( 'NONE',  ( -34.05631088549311869, -20.75780206758287605, 34.71020314001439289 ) ) ;
#12729 = VERTEX_POINT ( 'NONE', #5073 ) ;
#12730 = CYLINDRICAL_SURFACE ( 'NONE', #29293, 1.447898107987170890 ) ;
#12731 = B_SPLINE_CURVE_WITH_KNOTS ( 'NONE', 3,
 ( #8678, #8825, #6633, #15997, #16146, #18346, #25664, #30483, #27860, #1956, #20959 ),
 .UNSPECIFIED., .F., .F.,
 ( 4, 1, 1, 1, 1, 1, 1, 1, 4 ),
 ( 3.141592653589793116, 3.534291735288517255, 3.926990816987241395, 4.319689898685965090, 4.712388980384689674, 5.105088062083414258, 5.497787143782137953, 5.890486225480861648, 6.283185307179586232 ),
 .UNSPECIFIED. ) ;
#12732 = DIRECTION ( 'NONE',  ( 0.000000000000000000, 0.000000000000000000, 1.000000000000000000 ) ) ;
#12733 = DIRECTION ( 'NONE',  ( 0.000000000000000000, 0.000000000000000000, -1.000000000000000000 ) ) ;
#12734 = CARTESIAN_POINT ( 'NONE',  ( -19.69701826448871174, 3.468437286170584333, 19.08232364404839743 ) ) ;
#12735 = ORIENTED_EDGE ( 'NONE', *, *, #6915, .T. ) ;
#12736 = CARTESIAN_POINT ( 'NONE',  ( -15.30652580117162209, -7.480423316612006879, 5.701226463332907279 ) ) ;
#12737 = AXIS2_PLACEMENT_3D ( 'NONE', #18590, #8931, #2040 ) ;
#12738 = CARTESIAN_POINT ( 'NONE',  ( 12.35846533491530685, 11.73919094685904341, 20.34789198813115263 ) ) ;
#12739 = CARTESIAN_POINT ( 'NONE',  ( 37.99999999999999289, 65.00000000000000000, -0.000000000000000000 ) ) ;
#12740 = DIRECTION ( 'NONE',  ( -0.000000000000000000, 0.000000000000000000, 1.000000000000000000 ) ) ;
#12741 = CARTESIAN_POINT ( 'NONE',  ( 35.00000000000000000, 90.00000000000001421, -22.50000000000002487 ) ) ;
#12742 = CARTESIAN_POINT ( 'NONE',  ( 49.99999999999998579, -50.00000000000000000, 12.49999999999999112 ) ) ;
#12743 = DIRECTION ( 'NONE',  ( 1.000000000000000000, 0.000000000000000000, 0.000000000000000000 ) ) ;
#12744 = ORIENTED_EDGE ( 'NONE', *, *, #23256, .F. ) ;
#12745 = FACE_OUTER_BOUND ( 'NONE', #6107, .T. ) ;
#12746 = CARTESIAN_POINT ( 'NONE',  ( -11.86767874445213167, -1.850092897552710225, 1.500000000000001332 ) ) ;
#12747 = COLOUR_RGB ( '',0.7921568627450980005, 0.8196078431372548767, 0.9333333333333333481 ) ;
#12748 = ORIENTED_EDGE ( 'NONE', *, *, #20311, .F. ) ;
#12749 = ORIENTED_EDGE ( 'NONE', *, *, #18906, .T. ) ;
#12750 = LINE ( 'NONE', #15071, #7161 ) ;
#12751 = CARTESIAN_POINT ( 'NONE',  ( -48.64405085385531891, -18.29172496293576700, 24.50000000000000355 ) ) ;
#12752 = CARTESIAN_POINT ( 'NONE',  ( -34.89093055204507010, -9.806398194637136356, 27.50000000000000355 ) ) ;
#12753 = CARTESIAN_POINT ( 'NONE',  ( 13.00882613046785075, 10.97723423515712859, 19.22654678686458141 ) ) ;
#12754 = AXIS2_PLACEMENT_3D ( 'NONE', #5397, #26613, #9916 ) ;
#12755 = ORIENTED_EDGE ( 'NONE', *, *, #4988, .T. ) ;
#12756 = CARTESIAN_POINT ( 'NONE',  ( -16.96496223448355067, 1.652369715233091396, 7.652108011868850035 ) ) ;
#12757 = CARTESIAN_POINT ( 'NONE',  ( -3.858906612435654804, -7.730328572437724866, -1.500000000000002665 ) ) ;
#12758 = AXIS2_PLACEMENT_3D ( 'NONE', #29967, #20447, #30112 ) ;
#12759 = CARTESIAN_POINT ( 'NONE',  ( 40.57601884795947456, 0.2711064951079322771, -16.50000000000000000 ) ) ;
#12760 = VERTEX_POINT ( 'NONE', #2890 ) ;
#12761 = CARTESIAN_POINT ( 'NONE',  ( -4.953525029936337809, 16.29343450965543738, 18.54473042795395443 ) ) ;
#12762 = VERTEX_POINT ( 'NONE', #3042 ) ;
#12763 = FACE_OUTER_BOUND ( 'NONE', #22711, .T. ) ;
#12764 = AXIS2_PLACEMENT_3D ( 'NONE', #19916, #3373, #15203 ) ;
#12765 = ORIENTED_EDGE ( 'NONE', *, *, #22329, .F. ) ;
#12766 =( NAMED_UNIT ( * ) PLANE_ANGLE_UNIT ( ) SI_UNIT ( $, .RADIAN. ) );
#12767 = CARTESIAN_POINT ( 'NONE',  ( 38.99896367101428041, 0.7149996954306816477, 32.23183565673390660 ) ) ;
#12768 = CARTESIAN_POINT ( 'NONE',  ( 16.63005575832080041, 3.830191698062872074, 5.872146474157316831 ) ) ;
#12769 = CARTESIAN_POINT ( 'NONE',  ( -14.93957691572895818, 13.32381478560234456, 20.12545155307891065 ) ) ;
#12770 = CARTESIAN_POINT ( 'NONE',  ( 1.043163081472838760, -17.02278858106119586, 7.652108011868851811 ) ) ;
#12771 = EDGE_CURVE ( 'NONE', #21044, #29096, #19717, .T. ) ;
#12772 = CIRCLE ( 'NONE', #6771, 0.7499999999999988898 ) ;
#12773 = CARTESIAN_POINT ( 'NONE',  ( -20.59122450303579299, 36.11886001072432606, 29.42821036418931868 ) ) ;
#12774 = CARTESIAN_POINT ( 'NONE',  ( 0.000000000000000000, 42.50000000000000000, 27.50000000000000355 ) ) ;
#12775 = CARTESIAN_POINT ( 'NONE',  ( -37.16608720827707657, -65.00000000000000000, 57.49999999999999289 ) ) ;
#12776 = ORIENTED_EDGE ( 'NONE', *, *, #23258, .T. ) ;
#12777 = PRODUCT_DEFINITION ( 'UNKNOWN', '', #9906, #27005 ) ;
#12779 = AXIS2_PLACEMENT_3D ( 'NONE', #26730, #24532, #10043 ) ;
#12778 = CARTESIAN_POINT ( 'NONE',  ( 10.26079415706018771, -17.18817258638080503, 6.755862304746362845 ) ) ;
#12780 = CARTESIAN_POINT ( 'NONE',  ( -31.07284318477800866, 25.68762719043657583, 8.372895414906505351 ) ) ;
#12781 = CIRCLE ( 'NONE', #26712, 9.482273699623480212 ) ;
#12782 = DIRECTION ( 'NONE',  ( -1.000000000000000000, 0.000000000000000000, 0.000000000000000000 ) ) ;
#12783 = ADVANCED_FACE ( 'NONE', ( #5533 ), #12410, .F. ) ;
#12784 = ORIENTED_EDGE ( 'NONE', *, *, #30141, .F. ) ;
#12785 = ORIENTED_EDGE ( 'NONE', *, *, #3472, .T. ) ;
#12786 = CARTESIAN_POINT ( 'NONE',  ( -1.687027447297492211, -8.840471615930066918, -1.500000000000002665 ) ) ;
#12787 = DIRECTION ( 'NONE',  ( 0.000000000000000000, -1.132880637372608986E-16, 1.000000000000000000 ) ) ;
#12788 = ADVANCED_FACE ( 'NONE', ( #16925 ), #17228, .F. ) ;
#12789 = DIRECTION ( 'NONE',  ( 0.000000000000000000, -1.000000000000000000, 0.000000000000000000 ) ) ;
#12790 = VERTEX_POINT ( 'NONE', #4915 ) ;
#12791 = DIRECTION ( 'NONE',  ( 1.000000000000000000, 0.000000000000000000, -0.000000000000000000 ) ) ;
#12792 = CIRCLE ( 'NONE', #20265, 0.7500000000000006661 ) ;
#12793 = LINE ( 'NONE', #13106, #3219 ) ;
#12794 =( GEOMETRIC_REPRESENTATION_CONTEXT ( 3 ) GLOBAL_UNCERTAINTY_ASSIGNED_CONTEXT ( ( #14519 ) ) GLOBAL_UNIT_ASSIGNED_CONTEXT ( ( #14066, #23125, #4564 ) ) REPRESENTATION_CONTEXT ( 'NONE', 'WORKASPACE' ) );
#12795 = CARTESIAN_POINT ( 'NONE',  ( 5.419676874198345651, 19.25213680916389691, 5.651480102388686255 ) ) ;
#12796 = VERTEX_POINT ( 'NONE', #10207 ) ;
#12797 = LINE ( 'NONE', #5625, #25190 ) ;
#12798 = EDGE_CURVE ( 'NONE', #4256, #12192, #4494, .T. ) ;
#12799 = DIRECTION ( 'NONE',  ( 1.000000000000000000, 0.000000000000000000, 0.000000000000000000 ) ) ;
#12800 = CARTESIAN_POINT ( 'NONE',  ( 19.88570912806761370, 2.296683858978091575, 6.211014596808754007 ) ) ;
#12801 = VERTEX_POINT ( 'NONE', #14888 ) ;
#12803 = EDGE_CURVE ( 'NONE', #2701, #18086, #25885, .T. ) ;
#12802 = CIRCLE ( 'NONE', #30224, 9.084132297865673777 ) ;
#12804 = LINE ( 'NONE', #17789, #25283 ) ;
#12805 = VERTEX_POINT ( 'NONE', #17389 ) ;
#12806 = CARTESIAN_POINT ( 'NONE',  ( 19.18576292979354747, 22.55620591602726677, 1.500000000000001332 ) ) ;
#12807 = AXIS2_PLACEMENT_3D ( 'NONE', #14532, #21691, #18755 ) ;
#12808 = DIRECTION ( 'NONE',  ( 0.6707505147970023174, 0.7416830501633134842, 0.000000000000000000 ) ) ;
#12809 = AXIS2_PLACEMENT_3D ( 'NONE', #1728, #1885, #20900 ) ;
#12810 = ORIENTED_EDGE ( 'NONE', *, *, #5745, .T. ) ;
#12811 = CARTESIAN_POINT ( 'NONE',  ( 16.74250988114178185, 3.198928528055117848, 5.652196082368483587 ) ) ;
#12812 = LINE ( 'NONE', #488, #26534 ) ;
#12813 = DIRECTION ( 'NONE',  ( -0.000000000000000000, -1.000000000000000000, -0.000000000000000000 ) ) ;
#12814 = CARTESIAN_POINT ( 'NONE',  ( 22.58267429318970443, -26.57182937991349903, -6.499999999999999112 ) ) ;
#12815 = CARTESIAN_POINT ( 'NONE',  ( -35.99999999999995026, -1.782879839938830147, 34.75735931288075165 ) ) ;
#12816 = CARTESIAN_POINT ( 'NONE',  ( 10.42711161940499487, -17.06705191410861744, 19.96302680909625238 ) ) ;
#12817 = EDGE_CURVE ( 'NONE', #30377, #29282, #5227, .T. ) ;
#12818 = EDGE_LOOP ( 'NONE', ( #16540, #15117, #19184, #12071, #926, #27568 ) ) ;
#12819 = EDGE_CURVE ( 'NONE', #21250, #20491, #19930, .T. ) ;
#12820 = CARTESIAN_POINT ( 'NONE',  ( -32.28307784207223108, 8.475829241206282560, 41.62281023987520001 ) ) ;
#12821 = VECTOR ( 'NONE', #23169, 1000.000000000000000 ) ;
#12822 =( REPRESENTATION_RELATIONSHIP ('NONE','NONE', #19885, #10307 ) REPRESENTATION_RELATIONSHIP_WITH_TRANSFORMATION ( #25456 )SHAPE_REPRESENTATION_RELATIONSHIP( ) );
#12823 = CARTESIAN_POINT ( 'NONE',  ( -13.47895127716181207, 10.44112259311556556, 18.35718225375110180 ) ) ;
#12824 = CARTESIAN_POINT ( 'NONE',  ( 24.44496207165490631, -7.595930209050163029, 49.40206402021031096 ) ) ;
#12825 = VERTEX_POINT ( 'NONE', #12099 ) ;
#12826 = VECTOR ( 'NONE', #23148, 1000.000000000000114 ) ;
#12827 = CARTESIAN_POINT ( 'NONE',  ( 28.85400505702477858, -28.59354210116202211, 15.81854097348012544 ) ) ;
#12828 = CARTESIAN_POINT ( 'NONE',  ( 127.5000000000000000, 6.167321280506070407E-16, -5.035999999999999588 ) ) ;
#12829 = EDGE_CURVE ( 'NONE', #25657, #26575, #1498, .T. ) ;
#12830 = MANIFOLD_SOLID_BREP ( 'Boss-Extrude4', #15814 ) ;
#12831 = CARTESIAN_POINT ( 'NONE',  ( 12.53355205349238233, 11.54212474472216776, 7.626437579292366209 ) ) ;
#12832 = CARTESIAN_POINT ( 'NONE',  ( 0.000000000000000000, 1.699320956058915452E-16, -1.500000000000001776 ) ) ;
#12833 = AXIS2_PLACEMENT_3D ( 'NONE', #24782, #5759, #29321 ) ;
#12834 = DIRECTION ( 'NONE',  ( -0.000000000000000000, 0.000000000000000000, 1.000000000000000000 ) ) ;
#12835 = ADVANCED_FACE ( 'NONE', ( #388 ), #29087, .F. ) ;
#12836 = CARTESIAN_POINT ( 'NONE',  ( 19.54193581524819479, 36.78865913394601961, 34.51621032707691938 ) ) ;
#12837 = CIRCLE ( 'NONE', #30252, 0.7500000000000002220 ) ;
#12838 = EDGE_CURVE ( 'NONE', #21094, #1001, #690, .T. ) ;
#12839 = ORIENTED_EDGE ( 'NONE', *, *, #12004, .F. ) ;
#12840 = VECTOR ( 'NONE', #25628, 1000.000000000000000 ) ;
#12841 = CARTESIAN_POINT ( 'NONE',  ( -33.37783937289808733, -9.491076832576640143, 36.05646065681573020 ) ) ;
#12842 = AXIS2_PLACEMENT_3D ( 'NONE', #6634, #19102, #4595 ) ;
#12843 = CARTESIAN_POINT ( 'NONE',  ( 3.196529495465388226, 8.413215745755008967, 1.500000000000001332 ) ) ;
#12844 = ORIENTED_EDGE ( 'NONE', *, *, #6776, .F. ) ;
#12845 = ORIENTED_EDGE ( 'NONE', *, *, #19867, .T. ) ;
#12846 = CIRCLE ( 'NONE', #10838, 1.000000000000007772 ) ;
#12847 = CARTESIAN_POINT ( 'NONE',  ( 49.99999999999998579, 70.00000000000000000, 22.49999999999999289 ) ) ;
#12848 = AXIS2_PLACEMENT_3D ( 'NONE', #6236, #3438, #15742 ) ;
#12849 = ORIENTED_EDGE ( 'NONE', *, *, #26444, .F. ) ;
#12850 = PLANE ( 'NONE',  #28318 ) ;
#12851 = CIRCLE ( 'NONE', #23291, 0.7500000000000011102 ) ;
#12852 = ADVANCED_FACE ( 'NONE', ( #10372 ), #24702, .F. ) ;
#12853 = CARTESIAN_POINT ( 'NONE',  ( -18.22639394488086140, 34.06491890574931602, 34.50000000000000000 ) ) ;
#12854 = DIRECTION ( 'NONE',  ( 1.000000000000000000, 0.000000000000000000, 0.000000000000000000 ) ) ;
#12855 = AXIS2_PLACEMENT_3D ( 'NONE', #8202, #29264, #29720 ) ;
#12856 = CARTESIAN_POINT ( 'NONE',  ( -37.97827203760240877, 9.664683007568301676, 12.65335581815688748 ) ) ;
#12857 = CARTESIAN_POINT ( 'NONE',  ( -4.390207617113899730, 7.856594496258241023, 21.50000000000000000 ) ) ;
#12858 = DIRECTION ( 'NONE',  ( 0.000000000000000000, 1.132880637372608986E-16, -1.000000000000000000 ) ) ;
#12859 = DIRECTION ( 'NONE',  ( 0.000000000000000000, 0.000000000000000000, 1.000000000000000000 ) ) ;
#12860 = LINE ( 'NONE', #10355, #15739 ) ;
#12861 = DIRECTION ( 'NONE',  ( 0.000000000000000000, 1.000000000000000000, 0.000000000000000000 ) ) ;
#12862 = EDGE_CURVE ( 'NONE', #353, #24053, #1316, .T. ) ;
#12863 = AXIS2_PLACEMENT_3D ( 'NONE', #24561, #7584, #7431 ) ;
#12864 = VERTEX_POINT ( 'NONE', #27378 ) ;
#12865 = EDGE_CURVE ( 'NONE', #30279, #24466, #3810, .T. ) ;
#12866 = AXIS2_PLACEMENT_3D ( 'NONE', #13735, #20450, #10951 ) ;
#12867 = AXIS2_PLACEMENT_3D ( 'NONE', #10116, #29148, #7783 ) ;
#12868 = CARTESIAN_POINT ( 'NONE',  ( -9.356685943497542013, -14.22000274044911805, 19.66989035740801839 ) ) ;
#12869 = DIRECTION ( 'NONE',  ( -1.000000000000000000, 0.000000000000000000, 0.000000000000000000 ) ) ;
#12870 = CARTESIAN_POINT ( 'NONE',  ( -40.00000000000000000, 0.000000000000000000, 52.49999999999999289 ) ) ;
#12871 = CARTESIAN_POINT ( 'NONE',  ( 11.55802067824463109, -16.34381896053850269, 7.500147780736496017 ) ) ;
#12872 = CARTESIAN_POINT ( 'NONE',  ( -32.74775157610760346, -27.21557300919352329, -19.50000000000000355 ) ) ;
#12873 = CARTESIAN_POINT ( 'NONE',  ( 19.62935297797556444, -3.832558109936519575, 1.500000000000001332 ) ) ;
#12874 = VECTOR ( 'NONE', #7939, 1000.000000000000114 ) ;
#12875 = ORIENTED_EDGE ( 'NONE', *, *, #1487, .T. ) ;
#12876 = CIRCLE ( 'NONE', #19824, 0.7441270634457337607 ) ;
#12877 = CARTESIAN_POINT ( 'NONE',  ( -32.14097302481091134, 14.40131566728161161, 35.53783135158884221 ) ) ;
#12878 = CARTESIAN_POINT ( 'NONE',  ( -40.89187623478217404, -5.790488632116337797, -19.50000000000000355 ) ) ;
#12879 = CARTESIAN_POINT ( 'NONE',  ( 1.897190766380719928, -42.45663748335544341, 28.84347297178204528 ) ) ;
#12880 = CARTESIAN_POINT ( 'NONE',  ( -0.2301049870084636018, -17.01973991014544296, 6.519181285484531685 ) ) ;
#12881 = VERTEX_POINT ( 'NONE', #20343 ) ;
#12882 = CARTESIAN_POINT ( 'NONE',  ( 0.000000000000000000, 0.000000000000000000, 1.500000000000001332 ) ) ;
#12883 = DIRECTION ( 'NONE',  ( -0.000000000000000000, -0.000000000000000000, 1.000000000000000000 ) ) ;
#12884 = CIRCLE ( 'NONE', #6398, 20.00000000000000000 ) ;
#12885 = ORIENTED_EDGE ( 'NONE', *, *, #20, .T. ) ;
#12886 = CARTESIAN_POINT ( 'NONE',  ( 5.984782097461517125, 19.10229623552459088, 18.63641924841378028 ) ) ;
#12887 = AXIS2_PLACEMENT_3D ( 'NONE', #14713, #4738, #14570 ) ;
#12888 = VECTOR ( 'NONE', #6699, 1000.000000000000114 ) ;
#12889 = LINE ( 'NONE', #26769, #889 ) ;
#12890 = CARTESIAN_POINT ( 'NONE',  ( -39.02782386566561001, 2.105345730448363373, 35.08203289608308495 ) ) ;
#12891 = ORIENTED_EDGE ( 'NONE', *, *, #29834, .T. ) ;
#12892 = CARTESIAN_POINT ( 'NONE',  ( -28.20443790117967708, -1.387778780781445676E-14, 1.500000000000000000 ) ) ;
#12893 = EDGE_CURVE ( 'NONE', #7139, #20169, #29417, .T. ) ;
#12894 = DIRECTION ( 'NONE',  ( 0.000000000000000000, 1.000000000000000000, 0.000000000000000000 ) ) ;
#12895 = EDGE_CURVE ( 'NONE', #6285, #20644, #26355, .T. ) ;
#12896 = PLANE ( 'NONE',  #10345 ) ;
#12897 = CIRCLE ( 'NONE', #30310, 0.7500000000000006661 ) ;
#12898 = DIRECTION ( 'NONE',  ( -1.000000000000000000, 0.000000000000000000, 0.000000000000000000 ) ) ;
#12899 = ORIENTED_EDGE ( 'NONE', *, *, #26014, .T. ) ;
#12900 = CARTESIAN_POINT ( 'NONE',  ( -9.169883732660077058, -9.268939115642981008, 1.500000000000001332 ) ) ;
#12901 = CARTESIAN_POINT ( 'NONE',  ( -14.41708049311053053, 17.22181377296911720, 1.500000000000000000 ) ) ;
#12902 = CARTESIAN_POINT ( 'NONE',  ( -16.65122935894506639, -13.93942108199812324, -1.500000000000000000 ) ) ;
#12903 = LINE ( 'NONE', #29430, #20715 ) ;
#12904 = DIRECTION ( 'NONE',  ( 1.000000000000000000, 0.000000000000000000, 0.000000000000000000 ) ) ;
#12905 = FACE_OUTER_BOUND ( 'NONE', #1896, .T. ) ;
#12906 = LINE ( 'NONE', #22547, #30812 ) ;
#12907 = ORIENTED_EDGE ( 'NONE', *, *, #22685, .T. ) ;
#12908 = AXIS2_PLACEMENT_3D ( 'NONE', #28334, #1969, #2742 ) ;
#12909 = VECTOR ( 'NONE', #19517, 1000.000000000000000 ) ;
#12910 = DIRECTION ( 'NONE',  ( -1.000000000000000000, 0.000000000000000000, 0.000000000000000000 ) ) ;
#12911 = CARTESIAN_POINT ( 'NONE',  ( -4.390207617113899730, 7.856594496258241023, 21.50000000000000000 ) ) ;
#12912 = VERTEX_POINT ( 'NONE', #27060 ) ;
#12913 = VECTOR ( 'NONE', #22706, 1000.000000000000000 ) ;
#12914 = ORIENTED_EDGE ( 'NONE', *, *, #3881, .F. ) ;
#12915 = DIRECTION ( 'NONE',  ( -1.000000000000000000, 0.000000000000000000, -0.000000000000000000 ) ) ;
#12916 = LINE ( 'NONE', #29440, #15124 ) ;
#12917 = CARTESIAN_POINT ( 'NONE',  ( 0.000000000000000000, -2.435693370351110282E-15, 21.50000000000000355 ) ) ;
#12918 = CIRCLE ( 'NONE', #19359, 20.00000000000000000 ) ;
#12919 = FACE_OUTER_BOUND ( 'NONE', #26885, .T. ) ;
#12920 = CARTESIAN_POINT ( 'NONE',  ( 12.71123406193363081, 11.33589958720536650, 18.49267272388512140 ) ) ;
#12921 = EDGE_LOOP ( 'NONE', ( #13822, #6942 ) ) ;
#12922 = EDGE_LOOP ( 'NONE', ( #23429, #6936, #14762, #28139 ) ) ;
#12923 = CARTESIAN_POINT ( 'NONE',  ( -16.84919502704011052, 2.444546520875935158, 7.272049892295485485 ) ) ;
#12924 = AXIS2_PLACEMENT_3D ( 'NONE', #23580, #9250, #13784 ) ;
#12925 = CARTESIAN_POINT ( 'NONE',  ( 0.000000000000000000, -67.00000000000000000, 59.49999999999999289 ) ) ;
#12926 = B_SPLINE_CURVE_WITH_KNOTS ( 'NONE', 3,
 ( #6017, #8975, #1502, #11316, #6480, #3990, #13807, #27692, #4133, #6321, #11010, #11470, #1648, #20511, #18491, #3685 ),
 .UNSPECIFIED., .F., .F.,
 ( 4, 2, 2, 2, 2, 2, 2, 4 ),
 ( 0.5000000000000000000, 0.6250000000000021094, 0.6875000000000026645, 0.7187500000000029976, 0.7500000000000033307, 0.8125000000000023315, 0.8750000000000013323, 1.000000000000000000 ),
 .UNSPECIFIED. ) ;
#12927 = CARTESIAN_POINT ( 'NONE',  ( 40.53201937462365123, -2.366163742593401231, -16.50000000000000355 ) ) ;
#12928 = ORIENTED_EDGE ( 'NONE', *, *, #22, .T. ) ;
#12929 = CYLINDRICAL_SURFACE ( 'NONE', #20795, 21.71568325578193637 ) ;
#12930 = DIRECTION ( 'NONE',  ( 0.000000000000000000, 1.000000000000000000, 0.000000000000000000 ) ) ;
#12931 = CIRCLE ( 'NONE', #30350, 2.061368542273053883 ) ;
#12932 = ORIENTED_EDGE ( 'NONE', *, *, #18006, .T. ) ;
#12933 = CARTESIAN_POINT ( 'NONE',  ( -40.00000000000002842, 90.00000000000001421, 52.50000000000014921 ) ) ;
#12934 = CARTESIAN_POINT ( 'NONE',  ( 2.593413279260996074, -42.50000000000001421, 28.83974596215560027 ) ) ;
#12935 = LINE ( 'NONE', #15236, #9651 ) ;
#12936 = AXIS2_PLACEMENT_3D ( 'NONE', #18241, #22908, #4189 ) ;
#12937 = DIRECTION ( 'NONE',  ( 0.000000000000000000, 0.000000000000000000, 1.000000000000000000 ) ) ;
#12938 = CARTESIAN_POINT ( 'NONE',  ( -34.20814422162067814, -20.42093422158073679, 31.03595515439071306 ) ) ;
#12939 = DIRECTION ( 'NONE',  ( -0.000000000000000000, -0.000000000000000000, -1.000000000000000000 ) ) ;
#12940 = DIRECTION ( 'NONE',  ( 0.000000000000000000, 0.000000000000000000, 1.000000000000000000 ) ) ;
#12941 = ORIENTED_EDGE ( 'NONE', *, *, #10742, .F. ) ;
#12942 = CARTESIAN_POINT ( 'NONE',  ( 9.025811419443956041, -14.43167044742872207, 6.420335371522007506 ) ) ;
#12943 = AXIS2_PLACEMENT_3D ( 'NONE', #25112, #10767, #7979 ) ;
#12944 = PLANE ( 'NONE',  #23004 ) ;
#12945 = ORIENTED_EDGE ( 'NONE', *, *, #30388, .F. ) ;
#12946 = ORIENTED_EDGE ( 'NONE', *, *, #12406, .T. ) ;
#12947 = CARTESIAN_POINT ( 'NONE',  ( 18.12802117124498835, -8.449244086891157579, 20.22277707861862339 ) ) ;
#12948 = DIRECTION ( 'NONE',  ( 0.000000000000000000, 0.000000000000000000, 1.000000000000000000 ) ) ;
#12949 = CARTESIAN_POINT ( 'NONE',  ( -5.010690217951878189, 19.38064900392119227, 6.530762810602277924 ) ) ;
#12950 = ORIENTED_EDGE ( 'NONE', *, *, #16117, .T. ) ;
#12951 = CARTESIAN_POINT ( 'NONE',  ( -37.99999999999999289, 90.00000000000001421, -40.50000000000000000 ) ) ;
#12952 = DIRECTION ( 'NONE',  ( 0.000000000000000000, 0.000000000000000000, 1.000000000000000000 ) ) ;
#12953 = CYLINDRICAL_SURFACE ( 'NONE', #15920, 12.66227964008308682 ) ;
#12954 = ORIENTED_EDGE ( 'NONE', *, *, #22307, .T. ) ;
#12955 = CARTESIAN_POINT ( 'NONE',  ( 20.71335220384823117, 27.86167394782616213, -6.500000000000000888 ) ) ;
#12956 = CARTESIAN_POINT ( 'NONE',  ( 11.98626544954001005, 12.14249340222027840, 5.810767894563978686 ) ) ;
#12957 = CARTESIAN_POINT ( 'NONE',  ( 16.84609478243855563, 2.477959627222518613, 7.359006845440219102 ) ) ;
#12958 = EDGE_LOOP ( 'NONE', ( #6884, #16055 ) ) ;
#12959 = LINE ( 'NONE', #1100, #8351 ) ;
#12960 = ORIENTED_EDGE ( 'NONE', *, *, #26381, .F. ) ;
#12961 = CARTESIAN_POINT ( 'NONE',  ( 3.469446951953614189E-15, 30.50000000000000000, 1.500000000000001332 ) ) ;
#12962 = DIRECTION ( 'NONE',  ( -0.000000000000000000, 0.000000000000000000, 1.000000000000000000 ) ) ;
#12963 = AXIS2_PLACEMENT_3D ( 'NONE', #15851, #8687, #1663 ) ;
#12964 = ORIENTED_EDGE ( 'NONE', *, *, #17222, .T. ) ;
#12965 = ADVANCED_FACE ( 'NONE', ( #10993 ), #5998, .F. ) ;
#12966 = CARTESIAN_POINT ( 'NONE',  ( 5.089453839167154214, 19.35995229554825769, 7.627891251804737927 ) ) ;
#12967 = EDGE_CURVE ( 'NONE', #24377, #26649, #25331, .T. ) ;
#12968 = CARTESIAN_POINT ( 'NONE',  ( 33.56327786402390245, 10.22184702512350540, 39.91486591007065954 ) ) ;
#12969 = CARTESIAN_POINT ( 'NONE',  ( 5.291489565152559749, 19.28730510418394672, 18.34798005863226678 ) ) ;
#12970 = CARTESIAN_POINT ( 'NONE',  ( -4.677126025380957230, 39.24912351428227453, 34.80090346875804386 ) ) ;
#12971 = CARTESIAN_POINT ( 'NONE',  ( -15.57266529552202883, -38.96488032230103471, -1.500000000000000000 ) ) ;
#12972 = CARTESIAN_POINT ( 'NONE',  ( 31.89119714134807637, 14.79609055705961929, 39.84392849735361608 ) ) ;
#12973 = EDGE_LOOP ( 'NONE', ( #24538, #9634 ) ) ;
#12974 = DIRECTION ( 'NONE',  ( -0.000000000000000000, 1.132880637372608986E-16, -1.000000000000000000 ) ) ;
#12975 = CIRCLE ( 'NONE', #11483, 0.7500000000000007772 ) ;
#12976 = CARTESIAN_POINT ( 'NONE',  ( -15.80654879600848162, 12.28271411401623503, 20.06253562465620632 ) ) ;
#12977 = DIRECTION ( 'NONE',  ( 0.7557495743542582689, -0.6548607339452849896, 0.000000000000000000 ) ) ;
#12978 = CARTESIAN_POINT ( 'NONE',  ( -3.662523238938586001, -12.47340865698848056, 1.500000000000001332 ) ) ;
#12979 = VERTEX_POINT ( 'NONE', #3511 ) ;
#12980 = EDGE_CURVE ( 'NONE', #18536, #13653, #29125, .T. ) ;
#12981 = CARTESIAN_POINT ( 'NONE',  ( 32.04644741952905918, -24.22584960208014948, 8.083507045776100242 ) ) ;
#12982 = CARTESIAN_POINT ( 'NONE',  ( -42.73636061667930619, 67.00059800727392201, 62.14018330172965676 ) ) ;
#12983 = CARTESIAN_POINT ( 'NONE',  ( -14.69500743155267486, 13.56684717634543347, 19.08232364404840098 ) ) ;
#12984 = DIRECTION ( 'NONE',  ( -0.000000000000000000, 0.000000000000000000, 1.000000000000000000 ) ) ;
#12985 = FACE_OUTER_BOUND ( 'NONE', #3250, .T. ) ;
#12986 = DIRECTION ( 'NONE',  ( -1.000000000000000000, 0.000000000000000000, -0.000000000000000000 ) ) ;
#12987 = CARTESIAN_POINT ( 'NONE',  ( 16.78337223357194574, 2.938206247955208905, 5.676815824193228721 ) ) ;
#12988 = ORIENTED_EDGE ( 'NONE', *, *, #18687, .T. ) ;
#12989 = CYLINDRICAL_SURFACE ( 'NONE', #3623, 1.000000000000010436 ) ;
#12990 = ORIENTED_EDGE ( 'NONE', *, *, #24261, .T. ) ;
#12991 = CARTESIAN_POINT ( 'NONE',  ( 9.216505592218814158, -7.781333699927420966, -1.500000000000000000 ) ) ;
#12992 = CARTESIAN_POINT ( 'NONE',  ( 33.03677034811506275, 25.60271145924337688, -16.50000000000000000 ) ) ;
#12993 = ORIENTED_EDGE ( 'NONE', *, *, #21531, .F. ) ;
#12994 = EDGE_CURVE ( 'NONE', #5751, #3636, #17691, .T. ) ;
#12995 = ORIENTED_EDGE ( 'NONE', *, *, #27856, .T. ) ;
#12996 = EDGE_CURVE ( 'NONE', #4388, #19078, #1460, .T. ) ;
#12997 = CARTESIAN_POINT ( 'NONE',  ( -19.77413607932156481, 2.999736578675605170, 7.526993102356318133 ) ) ;
#12998 = VECTOR ( 'NONE', #13689, 1000.000000000000000 ) ;
#12999 = CARTESIAN_POINT ( 'NONE',  ( 6.899999999999999467, 9.000000000000000000, 0.000000000000000000 ) ) ;
#13000 = VERTEX_POINT ( 'NONE', #849 ) ;
#13001 = CARTESIAN_POINT ( 'NONE',  ( 0.3158150563615978457, -20.01532941283344158, 18.34777357837151968 ) ) ;
#13002 = EDGE_CURVE ( 'NONE', #27498, #4581, #13025, .T. ) ;
#13003 = CARTESIAN_POINT ( 'NONE',  ( 1.837104849652355830E-15, 50.00000000000000000, -70.00000000000000000 ) ) ;
#13004 = EDGE_CURVE ( 'NONE', #4107, #19828, #29516, .T. ) ;
#13005 = DIRECTION ( 'NONE',  ( 2.312964634635740689E-15, 1.000000000000000000, 0.000000000000000000 ) ) ;
#13006 = CARTESIAN_POINT ( 'NONE',  ( -23.27838112031802709, -36.10018649381529343, -16.50000600000000262 ) ) ;
#13007 = LINE ( 'NONE', #22497, #17312 ) ;
#13008 = CARTESIAN_POINT ( 'NONE',  ( -11.19063532726251609, -16.57644352599300319, 6.033082186765053478 ) ) ;
#13009 = DIRECTION ( 'NONE',  ( 1.000000000000000000, 0.000000000000000000, 0.000000000000000000 ) ) ;
#13010 = CARTESIAN_POINT ( 'NONE',  ( 0.3541522971493289429, -20.01464067411589198, 5.652196082364321583 ) ) ;
#13011 = CARTESIAN_POINT ( 'NONE',  ( 0.000000000000000000, 0.000000000000000000, -6.500000000000000888 ) ) ;
#13012 = EDGE_CURVE ( 'NONE', #6382, #15984, #29701, .T. ) ;
#13013 = ORIENTED_EDGE ( 'NONE', *, *, #21930, .F. ) ;
#13014 = EDGE_CURVE ( 'NONE', #984, #23438, #11291, .T. ) ;
#13015 = DIRECTION ( 'NONE',  ( 0.000000000000000000, -0.000000000000000000, -1.000000000000000000 ) ) ;
#13016 = CARTESIAN_POINT ( 'NONE',  ( -6.575147850411299899, 18.90724948634255753, 7.441806358946449151 ) ) ;
#13017 = ADVANCED_FACE ( 'NONE', ( #18770 ), #15971, .F. ) ;
#13018 = CARTESIAN_POINT ( 'NONE',  ( 10.57816699686867601, -13.40145493435145774, 6.131018562779544823 ) ) ;
#13019 = AXIS2_PLACEMENT_3D ( 'NONE', #26103, #28606, #16740 ) ;
#13020 = CARTESIAN_POINT ( 'NONE',  ( 13.22505861668094340, 42.10773672057246841, -19.50000000000000355 ) ) ;
#13021 = AXIS2_PLACEMENT_3D ( 'NONE', #17292, #19480, #919 ) ;
#13022 = DIRECTION ( 'NONE',  ( -0.000000000000000000, -0.000000000000000000, -1.000000000000000000 ) ) ;
#13023 = ORIENTED_EDGE ( 'NONE', *, *, #20259, .F. ) ;
#13024 = EDGE_LOOP ( 'NONE', ( #16779, #4525, #14551, #1049 ) ) ;
#13025 = LINE ( 'NONE', #17541, #5945 ) ;
#13026 = CARTESIAN_POINT ( 'NONE',  ( -32.74775157610760346, -27.21557300919352329, -19.50000000000000355 ) ) ;
#13027 = CARTESIAN_POINT ( 'NONE',  ( -12.71685080539083934, 11.31419172277363749, 6.530762810602277924 ) ) ;
#13028 = CARTESIAN_POINT ( 'NONE',  ( 2.959227181723801170, -8.499586724479446076, 21.50000000000000000 ) ) ;
#13029 = ORIENTED_EDGE ( 'NONE', *, *, #9962, .T. ) ;
#13030 = CARTESIAN_POINT ( 'NONE',  ( 0.000000000000000000, 0.000000000000000000, 1.500000000000001332 ) ) ;
#13031 = CARTESIAN_POINT ( 'NONE',  ( -8.795879380940577974, -2.270234684139648351, 21.50000000000000000 ) ) ;
#13032 = CARTESIAN_POINT ( 'NONE',  ( -9.321015140911132590, -14.24452793913984650, 7.080843742048788414 ) ) ;
#13033 = EDGE_CURVE ( 'NONE', #21717, #19170, #13910, .T. ) ;
#13034 = ORIENTED_EDGE ( 'NONE', *, *, #25344, .F. ) ;
#13035 = CARTESIAN_POINT ( 'NONE',  ( 4.654893560761752980, 16.38086414125080736, 18.55820869691756769 ) ) ;
#13036 = EDGE_CURVE ( 'NONE', #15693, #12097, #18474, .T. ) ;
#13037 = PLANE ( 'NONE',  #5369 ) ;
#13038 = EDGE_CURVE ( 'NONE', #22613, #1600, #18408, .T. ) ;
#13039 = CARTESIAN_POINT ( 'NONE',  ( 19.72123249184183180, 3.330269068327009752, 18.34869673959212122 ) ) ;
#13040 = ORIENTED_EDGE ( 'NONE', *, *, #12829, .F. ) ;
#13041 = CARTESIAN_POINT ( 'NONE',  ( 5.296161872597630271, 19.28602264385380849, 7.652108011868850035 ) ) ;
#13042 = EDGE_CURVE ( 'NONE', #10258, #15172, #13423, .T. ) ;
#13043 = DIRECTION ( 'NONE',  ( 0.000000000000000000, 0.000000000000000000, 1.000000000000000000 ) ) ;
#13044 = VECTOR ( 'NONE', #17323, 1000.000000000000000 ) ;
#13045 = CARTESIAN_POINT ( 'NONE',  ( 8.999114229549594057, -0.1262659238204522361, 21.50000000000000000 ) ) ;
#13046 = CARTESIAN_POINT ( 'NONE',  ( -19.84404562991029763, 2.492760124447683800, 18.34798005863226678 ) ) ;
#13047 = ORIENTED_EDGE ( 'NONE', *, *, #4662, .F. ) ;
#13048 = DIRECTION ( 'NONE',  ( 0.000000000000000000, 0.000000000000000000, 1.000000000000000000 ) ) ;
#13049 = CARTESIAN_POINT ( 'NONE',  ( 31.46019086465473436, 15.19107625323260891, 35.82171084658595817 ) ) ;
#13050 = CARTESIAN_POINT ( 'NONE',  ( 19.54426622602689179, 37.07991288358296345, -1.499999999999999778 ) ) ;
#13051 = EDGE_CURVE ( 'NONE', #18178, #20109, #25432, .T. ) ;
#13052 = DIRECTION ( 'NONE',  ( 1.000000000000000000, 0.000000000000000000, 0.000000000000000000 ) ) ;
#13053 = CARTESIAN_POINT ( 'NONE',  ( -40.22788059446288145, 5.869150616580578905, -16.50000000000000000 ) ) ;
#13054 = PLANE ( 'NONE',  #26293 ) ;
#13055 = DIRECTION ( 'NONE',  ( 1.000000000000000000, 0.000000000000000000, 0.000000000000000000 ) ) ;
#13056 = CARTESIAN_POINT ( 'NONE',  ( 11.82521593960875173, 5.400395169024529984, 1.500000000000001332 ) ) ;
#13057 = ORIENTED_EDGE ( 'NONE', *, *, #22730, .T. ) ;
#13058 = CIRCLE ( 'NONE', #25982, 0.7500000000000006661 ) ;
#13059 = CARTESIAN_POINT ( 'NONE',  ( 32.60608336680204644, -8.625548295239456209, 41.27238065709471471 ) ) ;
#13060 = CARTESIAN_POINT ( 'NONE',  ( 28.79137815760242702, -9.331429872129930914, 1.500000000000000000 ) ) ;
#13061 = ORIENTED_EDGE ( 'NONE', *, *, #16965, .F. ) ;
#13062 = ORIENTED_EDGE ( 'NONE', *, *, #3310, .F. ) ;
#13063 = EDGE_CURVE ( 'NONE', #11604, #2413, #462, .T. ) ;
#13064 = CARTESIAN_POINT ( 'NONE',  ( 0.000000000000000000, 0.000000000000000000, 1.500000000000001332 ) ) ;
#13065 = CARTESIAN_POINT ( 'NONE',  ( 1.964582201835905151, 2.267248723062786908, 24.50000000000000000 ) ) ;
#13066 = EDGE_CURVE ( 'NONE', #26044, #19148, #15965, .T. ) ;
#13067 = CARTESIAN_POINT ( 'NONE',  ( -50.00000000000000000, -70.00000000000000000, 59.49999999999999289 ) ) ;
#13068 = ORIENTED_EDGE ( 'NONE', *, *, #5389, .F. ) ;
#13069 = ADVANCED_FACE ( 'NONE', ( #28130, #13646, #27978 ), #20934, .T. ) ;
#13070 = CIRCLE ( 'NONE', #30471, 4.999999999999997335 ) ;
#13071 = CARTESIAN_POINT ( 'NONE',  ( 16.47768670952434178, 14.41708049311048789, 1.500000000000000000 ) ) ;
#13072 = DIRECTION ( 'NONE',  ( 1.000000000000000000, 0.000000000000000000, 0.000000000000000000 ) ) ;
#13073 = ORIENTED_EDGE ( 'NONE', *, *, #30330, .T. ) ;
#13074 = ORIENTED_EDGE ( 'NONE', *, *, #2312, .F. ) ;
#13075 = CARTESIAN_POINT ( 'NONE',  ( 16.02044690728354936, -5.868896442471950081, 20.19593175699879595 ) ) ;
#13076 = CARTESIAN_POINT ( 'NONE',  ( 39.99999999999998579, 90.00000000000001421, 47.49999999999999289 ) ) ;
#13077 = CARTESIAN_POINT ( 'NONE',  ( -8.917851762035226670, -14.51287734179233446, 18.44501272782439827 ) ) ;
#13078 = FACE_BOUND ( 'NONE', #22985, .T. ) ;
#13079 = ORIENTED_EDGE ( 'NONE', *, *, #4571, .T. ) ;
#13080 = DIRECTION ( 'NONE',  ( 0.000000000000000000, -0.000000000000000000, -1.000000000000000000 ) ) ;
#13081 = ORIENTED_EDGE ( 'NONE', *, *, #10365, .T. ) ;
#13082 = VECTOR ( 'NONE', #1627, 1000.000000000000000 ) ;
#13083 = DIRECTION ( 'NONE',  ( 0.000000000000000000, 0.000000000000000000, 1.000000000000000000 ) ) ;
#13084 = ORIENTED_EDGE ( 'NONE', *, *, #29150, .T. ) ;
#13085 = CARTESIAN_POINT ( 'NONE',  ( -6.809999484610175458, 18.80496293131997732, 19.85730954408918336 ) ) ;
#13086 = CARTESIAN_POINT ( 'NONE',  ( -27.86235613436986114, 14.72519157938688750, 39.24389099736758624 ) ) ;
#13087 = CARTESIAN_POINT ( 'NONE',  ( 19.70572240696341026, 3.522277800415036353, 7.603368798681074736 ) ) ;
#13088 = CARTESIAN_POINT ( 'NONE',  ( -15.30875331599079736, 12.89789204219718854, 18.34969686940296185 ) ) ;
#13089 = CARTESIAN_POINT ( 'NONE',  ( -8.423436389728852447, -14.82351904252668717, 20.33971507717571114 ) ) ;
#13090 = CARTESIAN_POINT ( 'NONE',  ( -16.96496224101209194, 1.652369717150043549, 20.34789198813115263 ) ) ;
#13091 = DIRECTION ( 'NONE',  ( -0.000000000000000000, -0.000000000000000000, -1.000000000000000000 ) ) ;
#13092 = DIRECTION ( 'NONE',  ( 0.7557495743542582689, -0.6548607339452849896, 0.000000000000000000 ) ) ;
#13093 = ORIENTED_EDGE ( 'NONE', *, *, #25344, .T. ) ;
#13094 = CARTESIAN_POINT ( 'NONE',  ( -13.83213539500865785, 7.758783772730382111, 24.50000000000000000 ) ) ;
#13095 = CARTESIAN_POINT ( 'NONE',  ( 10.57816699686867068, -13.40145493435145063, 18.82680253904184298 ) ) ;
#13096 = CARTESIAN_POINT ( 'NONE',  ( 39.99999999999998579, 90.00000000000001421, 15.49999999999999289 ) ) ;
#13097 = VERTEX_POINT ( 'NONE', #23282 ) ;
#13098 = ORIENTED_EDGE ( 'NONE', *, *, #25359, .T. ) ;
#13099 = CARTESIAN_POINT ( 'NONE',  ( 46.42112861060978446, 69.67901318393784038, 14.82662894843562107 ) ) ;
#13100 = CIRCLE ( 'NONE', #19563, 32.32717498572581860 ) ;
#13101 = DIRECTION ( 'NONE',  ( -0.000000000000000000, -0.000000000000000000, -1.000000000000000000 ) ) ;
#13102 = AXIS2_PLACEMENT_3D ( 'NONE', #12911, #22247, #5420 ) ;
#13103 = CYLINDRICAL_SURFACE ( 'NONE', #11870, 0.7499999999999997780 ) ;
#13104 = VERTEX_POINT ( 'NONE', #4568 ) ;
#13105 = FACE_OUTER_BOUND ( 'NONE', #27440, .T. ) ;
#13106 = CARTESIAN_POINT ( 'NONE',  ( 50.00000000000045475, -4.865382331816764069E-13, 82.49999999999998579 ) ) ;
#13107 = ADVANCED_FACE ( 'NONE', ( #11143, #6606, #13492 ), #30458, .T. ) ;
#13108 = CARTESIAN_POINT ( 'NONE',  ( 5.524309650260771143, -7.706848733600969226, 1.500000000000001332 ) ) ;
#13109 = EDGE_LOOP ( 'NONE', ( #29509, #299, #18217, #3207 ) ) ;
#13110 = CARTESIAN_POINT ( 'NONE',  ( 1.836970198721034716E-15, -15.00000000000005862, 117.5000000000000000 ) ) ;
#13111 = CARTESIAN_POINT ( 'NONE',  ( 12.05308393316171944, 12.07205540120323128, 5.749491821935610147 ) ) ;
#13112 = CARTESIAN_POINT ( 'NONE',  ( 19.85228648261877282, 2.570616772381430604, 5.862424720655265098 ) ) ;
#13113 = VERTEX_POINT ( 'NONE', #30158 ) ;
#13114 = CARTESIAN_POINT ( 'NONE',  ( 14.91976180470934388, 13.34593040386456408, 5.651989602109218858 ) ) ;
#13115 = ORIENTED_EDGE ( 'NONE', *, *, #4928, .F. ) ;
#13116 = CARTESIAN_POINT ( 'NONE',  ( -13.97970881677390587, 9.806700574777895696, 19.02573955821369367 ) ) ;
#13117 = DIRECTION ( 'NONE',  ( 0.2972711322815261292, 0.9547931052914340189, 0.000000000000000000 ) ) ;
#13118 = EDGE_LOOP ( 'NONE', ( #25070, #9435, #13584, #4801 ) ) ;
#13119 = VERTEX_POINT ( 'NONE', #21236 ) ;
#13120 = CIRCLE ( 'NONE', #655, 15.00000000000000000 ) ;
#13121 = CARTESIAN_POINT ( 'NONE',  ( 4.318335944327696296, 19.54627428603377126, 6.782048567692550378 ) ) ;
#13122 = DIRECTION ( 'NONE',  ( -0.000000000000000000, -0.000000000000000000, 1.000000000000000000 ) ) ;
#13123 = CARTESIAN_POINT ( 'NONE',  ( -7.869584159753960861, 10.39565510934976977, 1.500000000000001332 ) ) ;
#13124 = CARTESIAN_POINT ( 'NONE',  ( -32.31576317091163730, 17.59561277345963504, 34.80090346875804386 ) ) ;
#13125 = LINE ( 'NONE', #5947, #18313 ) ;
#13126 = FACE_OUTER_BOUND ( 'NONE', #27982, .T. ) ;
#13127 = ORIENTED_EDGE ( 'NONE', *, *, #28866, .T. ) ;
#13128 = CARTESIAN_POINT ( 'NONE',  ( -16.81263688882341967, 2.656251026639211865, 19.33715507985239412 ) ) ;
#13129 = CARTESIAN_POINT ( 'NONE',  ( 17.94887244118349301, -8.863227448567840838, 6.310736198168394928 ) ) ;
#13130 = CARTESIAN_POINT ( 'NONE',  ( -13.88241978398541576, 9.934084310449183164, 18.73743063545763121 ) ) ;
#13131 = CARTESIAN_POINT ( 'NONE',  ( 45.88720470728337375, 69.36824064663011313, 60.58574961613483367 ) ) ;
#13132 = ORIENTED_EDGE ( 'NONE', *, *, #22557, .F. ) ;
#13133 = ORIENTED_EDGE ( 'NONE', *, *, #21956, .T. ) ;
#13134 = CARTESIAN_POINT ( 'NONE',  ( 28.54797212025346909, -28.95590790227160483, 10.69245695584030997 ) ) ;
#13135 = CARTESIAN_POINT ( 'NONE',  ( 0.000000000000000000, 0.000000000000000000, 1.500000000000001332 ) ) ;
#13136 = B_SPLINE_SURFACE_WITH_KNOTS ( 'NONE', 1, 3, ( 
 ( #11909, #30603, #6751, #14067, #2382, #18768, #6911, #23578, #2221, #41, #6604, #23898, #4874, #11289, #20783, #8957, #18472, #16121, #11447, #11739, #14688, #24191, #5497, #8001, #7835, #29045, #28899, #14998, #184, #24511, #12200, #19675, #2844, #10168, #19212, #26557, #24360, #3156, #17034, #17347, #19840, #12055 ),
 ( #12682, #9865, #22174, #802, #7687, #14846, #5336, #9703, #2690, #12366, #10324, #16886, #3006, #27025, #12524, #26873, #21548, #26706, #21700, #29196, #7534, #19379, #24040, #5185, #29363, #21869, #22017, #17505, #5653, #15148, #2541, #653, #28741, #19532, #7378, #26406, #342, #5030, #14544, #503, #10023, #17185 ) ),
 .UNSPECIFIED., .F., .T., .F.,
 ( 2, 2 ),
 ( 4, 2, 2, 2, 2, 2, 2, 2, 2, 2, 2, 2, 2, 2, 2, 2, 2, 2, 2, 2, 4 ),
 ( 0.000000000000000000, 1.000000000000000000 ),
 ( 0.000000000000000000, 0.1963495408493620697, 0.3926990816987241395, 0.7853981633974482790, 1.178097245096172418, 1.570796326794896558, 1.963495408493620697, 2.356194490192344837, 2.748893571891068976, 2.945243112740430824, 3.141592653589793116, 3.337942194439155408, 3.534291735288517255, 3.926990816987241395, 4.319689898685965090, 4.712388980384689674, 5.105088062083414258, 5.497787143782137953, 5.890486225480861648, 6.086835766330223940, 6.283185307179586232 ),
 .UNSPECIFIED. ) ;
#13137 = CARTESIAN_POINT ( 'NONE',  ( 12.99618331673367244, 10.99290767929104540, 6.385774490351133537 ) ) ;
#13138 = AXIS2_PLACEMENT_3D ( 'NONE', #14875, #8333, #10509 ) ;
#13139 = CARTESIAN_POINT ( 'NONE',  ( 39.99999999999998579, 80.00000000000001421, 52.49999999999999289 ) ) ;
#13140 = LINE ( 'NONE', #5806, #15886 ) ;
#13141 = CIRCLE ( 'NONE', #20576, 3.000000000000002665 ) ;
#13142 = CARTESIAN_POINT ( 'NONE',  ( 16.87927834490895052, 2.194149605794860847, 6.714907520933423690 ) ) ;
#13143 = AXIS2_PLACEMENT_3D ( 'NONE', #15582, #29630, #6071 ) ;
#13144 = ORIENTED_EDGE ( 'NONE', *, *, #17753, .T. ) ;
#13145 = DIRECTION ( 'NONE',  ( -0.000000000000000000, -0.000000000000000000, 1.000000000000000000 ) ) ;
#13146 = CARTESIAN_POINT ( 'NONE',  ( 32.60829997825918980, 13.18983524832148646, 39.84356070656653515 ) ) ;
#13147 = DIRECTION ( 'NONE',  ( 1.000000000000000000, 0.000000000000000000, 0.000000000000000000 ) ) ;
#13148 = ORIENTED_EDGE ( 'NONE', *, *, #14699, .F. ) ;
#13149 = EDGE_LOOP ( 'NONE', ( #22107, #8974 ) ) ;
#13150 = DIRECTION ( 'NONE',  ( 0.000000000000000000, -1.000000000000000000, 0.000000000000000000 ) ) ;
#13151 = CARTESIAN_POINT ( 'NONE',  ( -5.687793815610304726, 6.974883619896852238, 21.50000000000000000 ) ) ;
#13152 = ORIENTED_EDGE ( 'NONE', *, *, #11664, .T. ) ;
#13153 = DIRECTION ( 'NONE',  ( 0.000000000000000000, 0.000000000000000000, 1.000000000000000000 ) ) ;
#13154 = CARTESIAN_POINT ( 'NONE',  ( 0.4912064067415030100, 50.00000000000000000, -70.00000000000001421 ) ) ;
#13155 = DIRECTION ( 'NONE',  ( -1.000000000000000000, 0.000000000000000000, 0.000000000000000000 ) ) ;
#13156 = CARTESIAN_POINT ( 'NONE',  ( -37.17124714164319244, 12.87530473911888151, 15.75708911316455918 ) ) ;
#13157 = CARTESIAN_POINT ( 'NONE',  ( 0.000000000000000000, 0.000000000000000000, 21.50000000000000000 ) ) ;
#13158 = CARTESIAN_POINT ( 'NONE',  ( -8.499586724479453181, -2.959227181723774525, 21.50000000000000000 ) ) ;
#13159 = CARTESIAN_POINT ( 'NONE',  ( -1.687027447297492211, -8.840471615930066918, 1.500000000000001332 ) ) ;
#13160 = CARTESIAN_POINT ( 'NONE',  ( -3.395021109945016491, -30.50000000000000355, 24.50000000000000000 ) ) ;
#13161 = ORIENTED_EDGE ( 'NONE', *, *, #2096, .T. ) ;
#13162 = AXIS2_PLACEMENT_3D ( 'NONE', #20441, #18103, #6242 ) ;
#13163 = CARTESIAN_POINT ( 'NONE',  ( -11.24586906513001772, -16.56046035145272199, 18.80699882434806369 ) ) ;
#13164 = DIRECTION ( 'NONE',  ( -0.000000000000000000, -0.000000000000000000, -1.000000000000000000 ) ) ;
#13165 = CARTESIAN_POINT ( 'NONE',  ( -5.544451647051929832, 16.11829164193972019, 7.652108011868850923 ) ) ;
#13166 = CARTESIAN_POINT ( 'NONE',  ( 9.864935476092966837, -13.90063640548121171, 5.652196082364323360 ) ) ;
#13167 = PRODUCT_RELATED_PRODUCT_CATEGORY ( 'part', '', ( #4430 ) ) ;
#13168 = DIRECTION ( 'NONE',  ( 0.000000000000000000, 0.000000000000000000, -1.000000000000000000 ) ) ;
#13169 = DIRECTION ( 'NONE',  ( -0.000000000000000000, -0.000000000000000000, 1.000000000000000000 ) ) ;
#13170 = ORIENTED_EDGE ( 'NONE', *, *, #22924, .T. ) ;
#13171 = VERTEX_POINT ( 'NONE', #16425 ) ;
#13172 = CARTESIAN_POINT ( 'NONE',  ( -30.74201181684193784, 15.50830195949553314, 36.32560960729297506 ) ) ;
#13173 = CARTESIAN_POINT ( 'NONE',  ( -34.07766914599908148, -21.40380666528021081, -1.500000000000000000 ) ) ;
#13174 = CARTESIAN_POINT ( 'NONE',  ( -12.78170796079387195, 11.24374406685325134, 6.211014596808754007 ) ) ;
#13175 = B_SPLINE_CURVE_WITH_KNOTS ( 'NONE', 3,
 ( #28396, #7176, #2497, #26048, #16689, #26196, #4828, #14344, #23853, #22129 ),
 .UNSPECIFIED., .F., .F.,
 ( 4, 2, 2, 2, 4 ),
 ( 0.1536962897835600916, 0.3652722173376700687, 0.5768481448917800458, 0.7884240724458899674, 1.000000000000000000 ),
 .UNSPECIFIED. ) ;
#13176 = EDGE_CURVE ( 'NONE', #863, #17560, #17245, .T. ) ;
#13177 = FACE_OUTER_BOUND ( 'NONE', #25872, .T. ) ;
#13178 = EDGE_LOOP ( 'NONE', ( #10786, #16686, #18097, #20701 ) ) ;
#13179 = CARTESIAN_POINT ( 'NONE',  ( 3.190007960661453534, 16.77295862815147842, 7.158811349119584833 ) ) ;
#13180 = CARTESIAN_POINT ( 'NONE',  ( 23.96732207937828463, 33.98584080152456011, -1.500000000000000000 ) ) ;
#13181 = CARTESIAN_POINT ( 'NONE',  ( -10.90225941753887362, -16.78887681002774812, 7.557577766377196582 ) ) ;
#13182 = VECTOR ( 'NONE', #3624, 1000.000000000000000 ) ;
#13183 = AXIS2_PLACEMENT_3D ( 'NONE', #1667, #18051, #3709 ) ;
#13184 = EDGE_CURVE ( 'NONE', #27848, #28528, #30340, .T. ) ;
#13185 = ORIENTED_EDGE ( 'NONE', *, *, #11681, .T. ) ;
#13186 = EDGE_CURVE ( 'NONE', #1048, #3168, #12525, .T. ) ;
#13187 = EDGE_CURVE ( 'NONE', #20644, #21650, #6501, .T. ) ;
#13188 = CARTESIAN_POINT ( 'NONE',  ( -23.07950435457407679, -11.50806656539752737, 49.21048435262065368 ) ) ;
#13189 = CARTESIAN_POINT ( 'NONE',  ( 19.65639872822723078, 3.693339721720559687, 20.22386025856690139 ) ) ;
#13190 = EDGE_LOOP ( 'NONE', ( #1069, #29762, #15650, #1430 ) ) ;
#13191 = DIRECTION ( 'NONE',  ( -0.4154150130018972598, -0.9096319953545133341, 0.000000000000000000 ) ) ;
#13192 = EDGE_CURVE ( 'NONE', #544, #22552, #20872, .T. ) ;
#13193 = VECTOR ( 'NONE', #27383, 1000.000000000000000 ) ;
#13194 = CARTESIAN_POINT ( 'NONE',  ( -37.16608720827707657, 65.00000000000000000, 12.49999999999999112 ) ) ;
#13195 = ORIENTED_EDGE ( 'NONE', *, *, #12829, .T. ) ;
#13196 = FACE_OUTER_BOUND ( 'NONE', #19163, .T. ) ;
#13197 = CARTESIAN_POINT ( 'NONE',  ( 23.17581250239729940, 34.50630206824671831, -1.499999999999999778 ) ) ;
#13198 = CARTESIAN_POINT ( 'NONE',  ( 27.03074382657074537, -6.449748410230991880, -16.55003854064094426 ) ) ;
#13199 = CARTESIAN_POINT ( 'NONE',  ( 0.000000000000000000, 0.000000000000000000, 1.500000000000000000 ) ) ;
#13200 = FACE_OUTER_BOUND ( 'NONE', #15711, .T. ) ;
#13201 = CIRCLE ( 'NONE', #30614, 0.7500000000000006661 ) ;
#13202 = CYLINDRICAL_SURFACE ( 'NONE', #4565, 0.7500000000000003331 ) ;
#13203 = DIRECTION ( 'NONE',  ( -0.000000000000000000, -0.000000000000000000, 1.000000000000000000 ) ) ;
#13204 = EDGE_CURVE ( 'NONE', #8467, #20812, #11427, .T. ) ;
#13205 = ADVANCED_FACE ( 'NONE', ( #14848 ), #17036, .F. ) ;
#13206 = EDGE_CURVE ( 'NONE', #2106, #24485, #10024, .T. ) ;
#13207 = CARTESIAN_POINT ( 'NONE',  ( 9.340794358757445792, -14.23940931083286898, 7.453286057244485008 ) ) ;
#13208 = CARTESIAN_POINT ( 'NONE',  ( 33.56327786402393087, -10.22184951998668190, 39.91486517541614631 ) ) ;
#13209 = CYLINDRICAL_SURFACE ( 'NONE', #23514, 12.18947652193948272 ) ;
#13210 = ORIENTED_EDGE ( 'NONE', *, *, #26439, .T. ) ;
#13211 = EDGE_CURVE ( 'NONE', #17470, #14477, #30822, .T. ) ;
#13212 = ORIENTED_EDGE ( 'NONE', *, *, #30546, .T. ) ;
#13213 = DIRECTION ( 'NONE',  ( 1.000000000000000000, 0.000000000000000000, -1.369518533665900065E-16 ) ) ;
#13214 = CARTESIAN_POINT ( 'NONE',  ( -10.64374042650075403, -42.96126232887726815, -19.50000000000000355 ) ) ;
#13215 = CARTESIAN_POINT ( 'NONE',  ( -8.413215745754975217, 3.196529495465474380, 21.50000000000000000 ) ) ;
#13216 = ADVANCED_FACE ( 'NONE', ( #2543 ), #12368, .F. ) ;
#13217 = VERTEX_POINT ( 'NONE', #654 ) ;
#13218 = CIRCLE ( 'NONE', #29144, 0.7500000000000002220 ) ;
#13219 = PLANE ( 'NONE',  #22844 ) ;
#13220 = CYLINDRICAL_SURFACE ( 'NONE', #19657, 0.7500000000000006661 ) ;
#13221 = EDGE_CURVE ( 'NONE', #28571, #28301, #44, .T. ) ;
#13222 = EDGE_CURVE ( 'NONE', #2571, #15921, #12058, .T. ) ;
#13223 = ORIENTED_EDGE ( 'NONE', *, *, #17404, .T. ) ;
#13224 = ORIENTED_EDGE ( 'NONE', *, *, #16230, .T. ) ;
#13225 = CARTESIAN_POINT ( 'NONE',  ( -16.87560513830565867, 2.281487909151090232, 7.429667576816606278 ) ) ;
#13226 = B_SPLINE_CURVE_WITH_KNOTS ( 'NONE', 3,
 ( #16971, #11995, #19616, #26489, #14942, #26814, #14782, #24452, #5123, #14634, #24135, #131 ),
 .UNSPECIFIED., .F., .F.,
 ( 4, 2, 2, 2, 2, 4 ),
 ( 2.975096543230397156E-07, 0.0009689891193463222828, 0.001937680729038321684, 0.002906372338730320651, 0.003390718143576315364, 0.003875063948422309643 ),
 .UNSPECIFIED. ) ;
#13227 = CARTESIAN_POINT ( 'NONE',  ( 19.63374410927882963, 3.902325345048615279, 20.06253562465620632 ) ) ;
#13228 = CARTESIAN_POINT ( 'NONE',  ( -8.643687819870514488, -14.68753251638875490, 18.35377592296120497 ) ) ;
#13229 = CARTESIAN_POINT ( 'NONE',  ( -11.92482408165411556, 35.57293605924007096, 37.49999999996230571 ) ) ;
#13230 = VERTEX_POINT ( 'NONE', #7381 ) ;
#13231 = CYLINDRICAL_SURFACE ( 'NONE', #21303, 0.7500000000000006661 ) ;
#13232 = AXIS2_PLACEMENT_3D ( 'NONE', #14815, #29012, #14660 ) ;
#13233 = ORIENTED_EDGE ( 'NONE', *, *, #6711, .T. ) ;
#13234 = DIRECTION ( 'NONE',  ( 1.000000000000000000, 0.000000000000000000, 0.000000000000000000 ) ) ;
#13235 = DIRECTION ( 'NONE',  ( 0.000000000000000000, 0.000000000000000000, -1.000000000000000000 ) ) ;
#13236 = ORIENTED_EDGE ( 'NONE', *, *, #11664, .F. ) ;
#13237 = ADVANCED_FACE ( 'NONE', ( #26707 ), #9555, .F. ) ;
#13239 = MANIFOLD_SOLID_BREP ( 'CirPattern4', #22286 ) ;
#13238 = FACE_OUTER_BOUND ( 'NONE', #372, .T. ) ;
#13240 = CARTESIAN_POINT ( 'NONE',  ( 19.57650873258265989, 4.179294809495486263, 6.447548852708279377 ) ) ;
#13241 = CARTESIAN_POINT ( 'NONE',  ( -12.96684546537104588, 11.03909700805841965, 18.55820869691756769 ) ) ;
#13242 = ADVANCED_FACE ( 'NONE', ( #5654 ), #28900, .F. ) ;
#13243 = VECTOR ( 'NONE', #8242, 1000.000000000000000 ) ;
#13244 = CARTESIAN_POINT ( 'NONE',  ( 22.58267429318971864, 26.57182937991349903, -1.500000000000000000 ) ) ;
#13245 = CARTESIAN_POINT ( 'NONE',  ( -17.06384985643509822, 0.6725948717545796596, 19.08844262864049313 ) ) ;
#13246 = CARTESIAN_POINT ( 'NONE',  ( -8.774062814044063074, -14.60569725947857833, 7.626437579292365321 ) ) ;
#13247 = DIRECTION ( 'NONE',  ( -0.000000000000000000, -0.000000000000000000, 1.000000000000000000 ) ) ;
#13248 = ORIENTED_EDGE ( 'NONE', *, *, #13033, .T. ) ;
#13249 = EDGE_CURVE ( 'NONE', #4645, #19042, #13140, .T. ) ;
#13250 = CARTESIAN_POINT ( 'NONE',  ( 10.65192122195201385, -13.34697535456211703, 19.03762469184452755 ) ) ;
#13251 = CARTESIAN_POINT ( 'NONE',  ( 28.55068628633582861, -24.19494186940697844, 34.80090346875809360 ) ) ;
#13252 = ORIENTED_EDGE ( 'NONE', *, *, #21561, .T. ) ;
#13253 = VERTEX_POINT ( 'NONE', #14999 ) ;
#13254 = CIRCLE ( 'NONE', #22683, 0.7441270634457181066 ) ;
#13255 = CARTESIAN_POINT ( 'NONE',  ( 45.62014130220955366, 69.51663404683095848, 14.22215358659609130 ) ) ;
#13256 = FACE_OUTER_BOUND ( 'NONE', #21321, .T. ) ;
#13257 = CARTESIAN_POINT ( 'NONE',  ( -4.786560543001539436, 16.33923032321832736, 6.018569869498933578 ) ) ;
#13258 = ORIENTED_EDGE ( 'NONE', *, *, #24444, .T. ) ;
#13259 = FACE_BOUND ( 'NONE', #6351, .T. ) ;
#13260 = CIRCLE ( 'NONE', #12268, 9.084132297865673777 ) ;
#13261 = CARTESIAN_POINT ( 'NONE',  ( -24.35970437652574105, 13.37404834226503247, 47.21042702067971675 ) ) ;
#13262 = DIRECTION ( 'NONE',  ( 0.000000000000000000, 1.000000000000000000, 1.193512090021232842E-16 ) ) ;
#13263 = ORIENTED_EDGE ( 'NONE', *, *, #28425, .T. ) ;
#13264 = CARTESIAN_POINT ( 'NONE',  ( -2.094186647214681063, 9.248129367672087042, 13.00000000000000178 ) ) ;
#13265 = AXIS2_PLACEMENT_3D ( 'NONE', #30338, #25514, #4136 ) ;
#13266 = CARTESIAN_POINT ( 'NONE',  ( -19.18576292979354392, -22.55620591602727742, 1.500000000000000000 ) ) ;
#13267 = CARTESIAN_POINT ( 'NONE',  ( -33.51229671200703564, -9.872960191568498800, 40.06382167421666907 ) ) ;
#13268 = VERTEX_POINT ( 'NONE', #29517 ) ;
#13269 = CARTESIAN_POINT ( 'NONE',  ( 12.64536614603776066, 11.41255465792765555, 5.749228751562096562 ) ) ;
#13270 = ORIENTED_EDGE ( 'NONE', *, *, #2096, .F. ) ;
#13271 = CARTESIAN_POINT ( 'NONE',  ( 10.18506332983503349, -29.04537757311073420, 24.50000000000000000 ) ) ;
#13272 = ORIENTED_EDGE ( 'NONE', *, *, #10346, .F. ) ;
#13273 = ORIENTED_EDGE ( 'NONE', *, *, #20978, .F. ) ;
#13274 = AXIS2_PLACEMENT_3D ( 'NONE', #26632, #26948, #3073 ) ;
#13275 = CARTESIAN_POINT ( 'NONE',  ( 4.365174083970719821, 19.53587658871429156, 6.341840715582230281 ) ) ;
#13276 = ADVANCED_FACE ( 'NONE', ( #22633 ), #17823, .F. ) ;
#13277 = CARTESIAN_POINT ( 'NONE',  ( 33.41082347385297169, 9.568393510027426885, 40.24615645622728266 ) ) ;
#13278 = CARTESIAN_POINT ( 'NONE',  ( -40.00000000000000000, 87.00000000000001421, 22.49999999999999289 ) ) ;
#13279 = VERTEX_POINT ( 'NONE', #3619 ) ;
#13280 = VECTOR ( 'NONE', #57, 1000.000000000000000 ) ;
#13281 = CARTESIAN_POINT ( 'NONE',  ( 10.66524827722686197, -16.94040236790928944, 18.49267272388512140 ) ) ;
#13282 = CARTESIAN_POINT ( 'NONE',  ( 19.86411046155384952, 2.477959627222519057, 20.05479082170252525 ) ) ;
#13283 = VERTEX_POINT ( 'NONE', #19842 ) ;
#13284 = CARTESIAN_POINT ( 'NONE',  ( -16.84919502704010696, 2.444546520875934270, 19.96783386855779341 ) ) ;
#13285 = CARTESIAN_POINT ( 'NONE',  ( 15.39534585122291332, -7.260971684546494664, 6.420335371522007506 ) ) ;
#13286 = CARTESIAN_POINT ( 'NONE',  ( -13.47385700491362570, 10.44730466805193281, 20.33971507717571114 ) ) ;
#13287 = CIRCLE ( 'NONE', #27732, 23.20393738267338790 ) ;
#13288 = CARTESIAN_POINT ( 'NONE',  ( 3.728348255937726563, 16.64288108867316396, 20.29915277494337644 ) ) ;
#13289 = ORIENTED_EDGE ( 'NONE', *, *, #15251, .F. ) ;
#13290 = EDGE_LOOP ( 'NONE', ( #12652, #16659, #763, #19807 ) ) ;
#13291 = CARTESIAN_POINT ( 'NONE',  ( -24.03057240117691862, 26.57182937991349903, -6.500000000000000888 ) ) ;
#13292 = CIRCLE ( 'NONE', #16763, 15.00000000000000000 ) ;
#13293 = DIRECTION ( 'NONE',  ( -0.000000000000000000, -0.000000000000000000, 1.000000000000000000 ) ) ;
#13294 = FACE_OUTER_BOUND ( 'NONE', #5588, .T. ) ;
#13295 = FACE_BOUND ( 'NONE', #24371, .T. ) ;
#13296 = LINE ( 'NONE', #6424, #12117 ) ;
#13297 = CARTESIAN_POINT ( 'NONE',  ( -7.706848733600990542, -5.524309650260742721, 1.500000000000001332 ) ) ;
#13298 = CIRCLE ( 'NONE', #10794, 0.7500000000000015543 ) ;
#13299 = CARTESIAN_POINT ( 'NONE',  ( -9.056472324687613096, -0.7083562926194844067, 13.22130136205108819 ) ) ;
#13300 = EDGE_LOOP ( 'NONE', ( #2222, #18376, #15849, #3917 ) ) ;
#13301 = VECTOR ( 'NONE', #11972, 1000.000000000000114 ) ;
#13302 = AXIS2_PLACEMENT_3D ( 'NONE', #29082, #21737, #10054 ) ;
#13303 = DIRECTION ( 'NONE',  ( 0.000000000000000000, -1.132880637372608986E-16, 1.000000000000000000 ) ) ;
#13304 = CARTESIAN_POINT ( 'NONE',  ( -33.56834390605528995, 10.30393839426307423, 39.88609648707288358 ) ) ;
#13305 = ORIENTED_EDGE ( 'NONE', *, *, #17028, .T. ) ;
#13306 = ORIENTED_EDGE ( 'NONE', *, *, #2750, .T. ) ;
#13307 = CARTESIAN_POINT ( 'NONE',  ( -19.71440049134193728, 3.368233808196386292, 6.144783687052523646 ) ) ;
#13308 = UNCERTAINTY_MEASURE_WITH_UNIT (LENGTH_MEASURE( 1.000000000000000082E-05 ), #10564, 'distance_accuracy_value', 'NONE');
#13309 = B_SPLINE_CURVE_WITH_KNOTS ( 'NONE', 3,
 ( #12738, #19912, #29426, #3368, #20366, #3832, #17563, #1338, #24726, #10856, #22236, #8060, #15200, #25814, #15834, #9119, #20661, #4446, #11165, #11471 ),
 .UNSPECIFIED., .F., .F.,
 ( 4, 2, 2, 2, 2, 2, 2, 2, 2, 4 ),
 ( 0.000000000000000000, 0.06250000000000194289, 0.1250000000000038858, 0.1875000000000058287, 0.2187500000000059119, 0.2500000000000059952, 0.3125000000000044964, 0.3750000000000029976, 0.4375000000000014988, 0.5000000000000000000 ),
 .UNSPECIFIED. ) ;
#13310 = CARTESIAN_POINT ( 'NONE',  ( -19.84404562991029763, 2.492760124447683800, 18.34798005863226678 ) ) ;
#13311 = ORIENTED_EDGE ( 'NONE', *, *, #17165, .F. ) ;
#13312 = CARTESIAN_POINT ( 'NONE',  ( -22.94541271838176755, -35.03073867844241818, -6.500000000000000888 ) ) ;
#13313 = CARTESIAN_POINT ( 'NONE',  ( -38.00000000000000000, 80.00000000000000000, -7.533656238527846826E-15 ) ) ;
#13314 = CARTESIAN_POINT ( 'NONE',  ( 37.16608720827707657, 65.00000000000000000, 97.07879600563551037 ) ) ;
#13315 = DIRECTION ( 'NONE',  ( 0.000000000000000000, 0.000000000000000000, 1.000000000000000000 ) ) ;
#13316 = VECTOR ( 'NONE', #6435, 1000.000000000000000 ) ;
#13317 = CARTESIAN_POINT ( 'NONE',  ( 7.730328572437743517, -4.608906612435629491, -3.621320343559650379 ) ) ;
#13318 = VECTOR ( 'NONE', #12120, 1000.000000000000000 ) ;
#13319 = CARTESIAN_POINT ( 'NONE',  ( 49.99999999999998579, -50.00000000000000000, -87.50000000000000000 ) ) ;
#13320 = CARTESIAN_POINT ( 'NONE',  ( 0.4984457374290394149, -20.01168570850557415, 7.643931100913408550 ) ) ;
#13321 = CARTESIAN_POINT ( 'NONE',  ( -16.84831847205055411, 2.450595478048609444, 7.267659094423558841 ) ) ;
#13322 = ORIENTED_EDGE ( 'NONE', *, *, #15478, .F. ) ;
#13323 = AXIS2_PLACEMENT_3D ( 'NONE', #445, #14181, #2646 ) ;
#13324 = CARTESIAN_POINT ( 'NONE',  ( -9.002647793593395065, -14.45788447640154040, 18.49267272388512140 ) ) ;
#13325 = DIRECTION ( 'NONE',  ( 1.000000000000000000, 0.000000000000000000, 0.000000000000000000 ) ) ;
#13326 = CARTESIAN_POINT ( 'NONE',  ( -22.58267429318970443, -26.57182937991348481, -1.500000000000001332 ) ) ;
#13327 = CARTESIAN_POINT ( 'NONE',  ( 10.13630142350640817, -13.71646693216191082, 7.603368798681074736 ) ) ;
#13328 = CARTESIAN_POINT ( 'NONE',  ( 32.74775157611827581, 27.21557300921217859, -19.50000000000000355 ) ) ;
#13329 = CIRCLE ( 'NONE', #10830, 0.7441270634457181066 ) ;
#13330 = CARTESIAN_POINT ( 'NONE',  ( -33.56834390605528995, 10.30393839426307423, 35.64345579995360680 ) ) ;
#13331 = AXIS2_PLACEMENT_3D ( 'NONE', #1275, #3461, #3295 ) ;
#13332 = ORIENTED_EDGE ( 'NONE', *, *, #10715, .T. ) ;
#13333 = DIRECTION ( 'NONE',  ( 1.000000000000000000, 0.000000000000000000, 0.000000000000000000 ) ) ;
#13334 = CARTESIAN_POINT ( 'NONE',  ( 37.98493438987956949, 11.12428508576150143, -1.500000000000000000 ) ) ;
#13335 = CARTESIAN_POINT ( 'NONE',  ( -0.1851967867237511445, -37.50414277995155743, 37.50000000001682565 ) ) ;
#13336 = LINE ( 'NONE', #20180, #6113 ) ;
#13337 = ORIENTED_EDGE ( 'NONE', *, *, #8669, .T. ) ;
#13338 = LINE ( 'NONE', #15507, #20378 ) ;
#13339 = CIRCLE ( 'NONE', #19797, 9.482273699623480212 ) ;
#13340 = CARTESIAN_POINT ( 'NONE',  ( 37.98493438987956949, 11.12428508576150143, -1.500000000000000000 ) ) ;
#13341 = CARTESIAN_POINT ( 'NONE',  ( -8.611567383417474630, -14.70762963579928773, 5.653912893140659257 ) ) ;
#13342 = AXIS2_PLACEMENT_3D ( 'NONE', #10256, #29300, #7941 ) ;
#13343 = ORIENTED_EDGE ( 'NONE', *, *, #22555, .F. ) ;
#13344 = VECTOR ( 'NONE', #20767, 1000.000000000000000 ) ;
#13345 = CARTESIAN_POINT ( 'NONE',  ( -23.07950435457408389, -11.74770253185616298, 49.10355149311385503 ) ) ;
#13346 = CARTESIAN_POINT ( 'NONE',  ( -11.92114224723059124, -40.47287111344137145, 29.01828771891121761 ) ) ;
#13347 = EDGE_CURVE ( 'NONE', #2272, #29438, #21340, .T. ) ;
#13348 = VERTEX_POINT ( 'NONE', #20308 ) ;
#13349 = CARTESIAN_POINT ( 'NONE',  ( -26.12638453225885726, -6.310846377660610074, 43.87962907655882105 ) ) ;
#13350 = AXIS2_PLACEMENT_3D ( 'NONE', #23791, #11791, #7119 ) ;
#13351 = VECTOR ( 'NONE', #25778, 1000.000000000000000 ) ;
#13352 = DIRECTION ( 'NONE',  ( -0.000000000000000000, -0.000000000000000000, 1.000000000000000000 ) ) ;
#13353 = AXIS2_PLACEMENT_3D ( 'NONE', #3218, #24275, #12442 ) ;
#13354 = EDGE_LOOP ( 'NONE', ( #25568, #14106 ) ) ;
#13355 = DIRECTION ( 'NONE',  ( -0.000000000000000000, 1.000000000000000000, -0.000000000000000000 ) ) ;
#13356 = CARTESIAN_POINT ( 'NONE',  ( 31.57476163834522964, 15.10795358447669479, 35.75454235600946618 ) ) ;
#13357 = CARTESIAN_POINT ( 'NONE',  ( -3.196529495465446402, -8.413215745754985875, 1.500000000000001332 ) ) ;
#13358 = ADVANCED_FACE ( 'NONE', ( #29837 ), #8154, .F. ) ;
#13359 = CARTESIAN_POINT ( 'NONE',  ( -42.09461541023539155, 68.37430988400880949, 12.71698366717900619 ) ) ;
#13360 = CIRCLE ( 'NONE', #22806, 9.084132297865673777 ) ;
#13361 = CARTESIAN_POINT ( 'NONE',  ( -17.05621956093816749, 0.7704973847036212797, 7.158811349119585721 ) ) ;
#13362 = AXIS2_PLACEMENT_3D ( 'NONE', #9578, #26257, #2239 ) ;
#13363 = DIRECTION ( 'NONE',  ( 1.000000000000000000, 0.000000000000000000, 0.000000000000000000 ) ) ;
#13364 = CYLINDRICAL_SURFACE ( 'NONE', #26964, 0.7500000000000002220 ) ;
#13365 = CARTESIAN_POINT ( 'NONE',  ( 2.959227181723801170, -8.499586724479446076, -1.500000000000002665 ) ) ;
#13366 = CARTESIAN_POINT ( 'NONE',  ( 32.82330813384209023, -22.94799032726822929, -1.500000000000000000 ) ) ;
#13367 = CARTESIAN_POINT ( 'NONE',  ( 35.78336344873347485, -4.414649291701021383, 34.71346399078482392 ) ) ;
#13368 = FACE_OUTER_BOUND ( 'NONE', #30841, .T. ) ;
#13369 = ORIENTED_EDGE ( 'NONE', *, *, #7480, .F. ) ;
#13370 = VERTEX_POINT ( 'NONE', #25134 ) ;
#13371 = EDGE_CURVE ( 'NONE', #6597, #26415, #2933, .T. ) ;
#13372 = DIRECTION ( 'NONE',  ( -1.000000000000000000, 0.000000000000000000, 0.000000000000000000 ) ) ;
#13373 = CARTESIAN_POINT ( 'NONE',  ( -39.83602371821034183, 11.57901747687032490, -19.50000000000000355 ) ) ;
#13374 = AXIS2_PLACEMENT_3D ( 'NONE', #18724, #28236, #6866 ) ;
#13375 = CARTESIAN_POINT ( 'NONE',  ( -4.163336342344337027E-14, 1.387778780781445676E-14, 1.500000000000000000 ) ) ;
#13376 = EDGE_LOOP ( 'NONE', ( #14469, #5424, #29606, #12713 ) ) ;
#13377 = SHAPE_REPRESENTATION_RELATIONSHIP ( 'NONE' , 'NONE' ,  #19685, #23278 ) ;
#13378 = AXIS2_PLACEMENT_3D ( 'NONE', #19133, #23800, #9930 ) ;
#13379 = CARTESIAN_POINT ( 'NONE',  ( -4.163336342344337027E-14, 1.387778780781445676E-14, -1.500000000000000000 ) ) ;
#13380 = CIRCLE ( 'NONE', #22822, 10.00000000000000000 ) ;
#13381 = DIRECTION ( 'NONE',  ( 0.000000000000000000, 0.000000000000000000, 1.000000000000000000 ) ) ;
#13382 = ORIENTED_EDGE ( 'NONE', *, *, #14434, .T. ) ;
#13383 = ORIENTED_EDGE ( 'NONE', *, *, #27045, .T. ) ;
#13384 = CARTESIAN_POINT ( 'NONE',  ( -16.90598708042469056, 2.083096162940500484, 5.749228751562096562 ) ) ;
#13385 = CARTESIAN_POINT ( 'NONE',  ( 0.000000000000000000, 1.699320956058915452E-16, -1.500000000000001776 ) ) ;
#13386 = CARTESIAN_POINT ( 'NONE',  ( 15.40745978470623534, 12.75221478727798896, 6.033082186765058808 ) ) ;
#13387 = CARTESIAN_POINT ( 'NONE',  ( -6.224883619896829146, -5.687793815610328707, -3.621320343559650379 ) ) ;
#13388 = ORIENTED_EDGE ( 'NONE', *, *, #9033, .T. ) ;
#13389 = LINE ( 'NONE', #22880, #384 ) ;
#13390 = EDGE_CURVE ( 'NONE', #5509, #26574, #14498, .T. ) ;
#13391 = VERTEX_POINT ( 'NONE', #13297 ) ;
#13392 = ADVANCED_FACE ( 'NONE', ( #804 ), #3305, .F. ) ;
#13393 = DIRECTION ( 'NONE',  ( -0.000000000000000000, -0.000000000000000000, 1.000000000000000000 ) ) ;
#13394 = CARTESIAN_POINT ( 'NONE',  ( -16.93131609043274821, 1.909234121842923626, 18.37259980046034613 ) ) ;
#13395 = ORIENTED_EDGE ( 'NONE', *, *, #3494, .T. ) ;
#13396 = CARTESIAN_POINT ( 'NONE',  ( -6.742350454026563078, 18.82948505227175318, 18.73377938172348678 ) ) ;
#13397 = AXIS2_PLACEMENT_3D ( 'NONE', #8999, #9457, #2113 ) ;
#13398 = EDGE_CURVE ( 'NONE', #191, #4424, #1939, .T. ) ;
#13399 = DIRECTION ( 'NONE',  ( 0.000000000000000000, 0.000000000000000000, -1.000000000000000000 ) ) ;
#13400 = B_SPLINE_CURVE_WITH_KNOTS ( 'NONE', 3,
 ( #20298, #10475, #24659, #5956, #15454, #15292, #7996, #24822, #19988, #8466, #24972, #13131, #22010, #22625, #794, #10316 ),
 .UNSPECIFIED., .F., .F.,
 ( 4, 2, 2, 2, 2, 2, 2, 4 ),
 ( -2.365086329950664848E-05, 0.002543131582615900527, 0.005109914028531307648, 0.006393305251489012943, 0.007676696474446719105, 0.008318392085925573054, 0.008960087697404424401, 0.01024347892036214444 ),
 .UNSPECIFIED. ) ;
#13401 = B_SPLINE_SURFACE_WITH_KNOTS ( 'NONE', 3, 1, ( 
 ( #20589, #9202 ),
 ( #30114, #13888 ),
 ( #29969, #2027 ),
 ( #25592, #8745 ),
 ( #4069, #25446 ),
 ( #13597, #22933 ),
 ( #11552, #3930 ),
 ( #18716, #8607 ),
 ( #18113, #15607 ),
 ( #28225, #25125 ),
 ( #4212, #23075 ),
 ( #20733, #27787 ),
 ( #3768, #6414 ),
 ( #27628, #1880 ),
 ( #23225, #1585 ),
 ( #30266, #8912 ),
 ( #11403, #6252 ),
 ( #15763, #18575 ),
 ( #20895, #18435 ),
 ( #27937, #6564 ),
 ( #16076, #30420 ),
 ( #9057, #4674 ),
 ( #6858, #21354 ),
 ( #11408, #4522 ),
 ( #14338, #16683 ),
 ( #9663, #14176 ),
 ( #24150, #26042 ),
 ( #21823, #14031 ),
 ( #11696, #23535 ),
 ( #12318, #464 ),
 ( #4983, #28695 ) ),
 .UNSPECIFIED., .F., .F., .F.,
 ( 4, 3, 3, 3, 3, 3, 3, 3, 3, 3, 4 ),
 ( 2, 2 ),
 ( 0.4999999998345682206, 0.5360336730431942698, 0.5907651151589017324, 0.6456034593241839481, 0.6998270958050443191, 0.7529536536315944995, 0.8052385063053264513, 0.8575343587103996246, 0.9106564858195047574, 0.9648414833209688624, 1.000000006602610014 ),
 ( 0.000000000000000000, 1.000000000000000000 ),
 .UNSPECIFIED. ) ;
#13402 = CARTESIAN_POINT ( 'NONE',  ( -0.08122345276805190140, -17.02407875822364147, 7.176035686813569292 ) ) ;
#13403 = AXIS2_PLACEMENT_3D ( 'NONE', #14832, #24653, #22618 ) ;
#13404 = CIRCLE ( 'NONE', #3411, 9.482273699623480212 ) ;
#13405 = AXIS2_PLACEMENT_3D ( 'NONE', #16470, #4922, #21448 ) ;
#13406 = CARTESIAN_POINT ( 'NONE',  ( 19.74251403343738076, 3.198927889078825970, 5.652196082369965069 ) ) ;
#13407 = ADVANCED_FACE ( 'NONE', ( #10485, #27176, #20460, #29365, #29980, #8003 ), #26875, .F. ) ;
#13408 = DIRECTION ( 'NONE',  ( 0.000000000000000000, 1.000000000000000000, 0.000000000000000000 ) ) ;
#13409 = CARTESIAN_POINT ( 'NONE',  ( -17.04337418722499820, 0.9225192032720760382, 18.64703902303423178 ) ) ;
#13410 = FACE_BOUND ( 'NONE', #17935, .T. ) ;
#13411 = ORIENTED_EDGE ( 'NONE', *, *, #6483, .T. ) ;
#13412 = EDGE_CURVE ( 'NONE', #27939, #7334, #22478, .T. ) ;
#13413 = CARTESIAN_POINT ( 'NONE',  ( -70.00000000000000000, 50.00000000000000000, -92.50000000000000000 ) ) ;
#13414 = CIRCLE ( 'NONE', #15386, 9.084132297865673777 ) ;
#13415 = CARTESIAN_POINT ( 'NONE',  ( 11.52197458429824550, -37.50933785548061650, 27.50000000000000355 ) ) ;
#13416 = EDGE_LOOP ( 'NONE', ( #2030, #9713, #19202, #27137 ) ) ;
#13417 = ORIENTED_EDGE ( 'NONE', *, *, #1927, .F. ) ;
#13418 = EDGE_CURVE ( 'NONE', #4932, #8309, #10638, .T. ) ;
#13419 = CARTESIAN_POINT ( 'NONE',  ( 40.58772298843799575, 67.65983010127237662, 12.49999999999999289 ) ) ;
#13420 = FACE_OUTER_BOUND ( 'NONE', #18166, .T. ) ;
#13421 = CARTESIAN_POINT ( 'NONE',  ( -7.730328572437709767, 4.608906612435681005, 1.500000000000001332 ) ) ;
#13422 = ORIENTED_EDGE ( 'NONE', *, *, #19089, .F. ) ;
#13423 = CIRCLE ( 'NONE', #7438, 0.7500000000000006661 ) ;
#13424 = CARTESIAN_POINT ( 'NONE',  ( -40.00000000000002842, 80.00000000000001421, 27.49999999999983658 ) ) ;
#13425 = DIRECTION ( 'NONE',  ( -0.5503133621338232029, -0.8349582046168344540, 0.000000000000000000 ) ) ;
#13426 = CARTESIAN_POINT ( 'NONE',  ( -6.980328572437709767, 4.608906612435681005, -3.621320343559650379 ) ) ;
#13427 = ORIENTED_EDGE ( 'NONE', *, *, #4084, .F. ) ;
#13428 = FACE_OUTER_BOUND ( 'NONE', #1941, .T. ) ;
#13429 = AXIS2_PLACEMENT_3D ( 'NONE', #15293, #3462, #10476 ) ;
#13430 = CARTESIAN_POINT ( 'NONE',  ( -8.430595340551228389, 4.340342926365043930, 13.00000000000000178 ) ) ;
#13431 = ORIENTED_EDGE ( 'NONE', *, *, #868, .F. ) ;
#13432 = DIRECTION ( 'NONE',  ( 0.6707505147970010961, -0.7416830501633147055, 0.000000000000000000 ) ) ;
#13433 = ADVANCED_FACE ( 'NONE', ( #22176, #29667 ), #8305, .T. ) ;
#13434 = ORIENTED_EDGE ( 'NONE', *, *, #189, .T. ) ;
#13435 = CARTESIAN_POINT ( 'NONE',  ( -37.99999999999999289, 70.00000000000000000, -34.49999999999999289 ) ) ;
#13436 = ADVANCED_FACE ( 'NONE', ( #30276 ), #11560, .F. ) ;
#13437 = ORIENTED_EDGE ( 'NONE', *, *, #1025, .F. ) ;
#13438 = CIRCLE ( 'NONE', #7949, 1.447898107987198646 ) ;
#13439 = ADVANCED_FACE ( 'NONE', ( #20600 ), #6427, .F. ) ;
#13440 = VERTEX_POINT ( 'NONE', #15942 ) ;
#13441 = CARTESIAN_POINT ( 'NONE',  ( 9.163215745754998309, -3.196529495465417980, 1.500000000000001332 ) ) ;
#13442 = CARTESIAN_POINT ( 'NONE',  ( 5.549407557472024521, 19.21507098571442285, 20.32243167357988867 ) ) ;
#13443 = VERTEX_POINT ( 'NONE', #20905 ) ;
#13444 = CIRCLE ( 'NONE', #9441, 10.00000000000000000 ) ;
#13445 = CYLINDRICAL_SURFACE ( 'NONE', #23761, 0.7500000000000006661 ) ;
#13446 = CARTESIAN_POINT ( 'NONE',  ( 19.89210292178043460, 2.240810012149824892, 19.66989035740801839 ) ) ;
#13447 = EDGE_LOOP ( 'NONE', ( #23212, #18698 ) ) ;
#13448 = EDGE_CURVE ( 'NONE', #6144, #23060, #10107, .T. ) ;
#13449 = CARTESIAN_POINT ( 'NONE',  ( -12.72536390617885260, -2.839914339433650348, 1.500000000000001332 ) ) ;
#13450 = CARTESIAN_POINT ( 'NONE',  ( -49.99999999999998579, 209.2686044187655909, -75.50000000000002842 ) ) ;
#13451 = DIRECTION ( 'NONE',  ( 0.000000000000000000, 1.000000000000000000, 0.000000000000000000 ) ) ;
#13452 = CARTESIAN_POINT ( 'NONE',  ( 4.972463595808062742, 19.39063357279558275, 18.39992786714538298 ) ) ;
#13453 = ORIENTED_EDGE ( 'NONE', *, *, #30177, .T. ) ;
#13454 = ORIENTED_EDGE ( 'NONE', *, *, #8977, .F. ) ;
#13455 = CYLINDRICAL_SURFACE ( 'NONE', #27770, 20.00000000000000355 ) ;
#13456 = CARTESIAN_POINT ( 'NONE',  ( 10.08077896144684260, -13.75650449134903397, 7.652108011868851811 ) ) ;
#13457 = CARTESIAN_POINT ( 'NONE',  ( 14.96781329949620165, 13.26582956964653448, 18.34726407865098707 ) ) ;
#13458 = CARTESIAN_POINT ( 'NONE',  ( -4.997519263521717825, 19.38405562624022949, 19.33715507985239412 ) ) ;
#13459 = DIRECTION ( 'NONE',  ( 0.000000000000000000, 0.000000000000000000, -1.000000000000000000 ) ) ;
#13460 = DIRECTION ( 'NONE',  ( 1.000000000000000000, 0.000000000000000000, 0.000000000000000000 ) ) ;
#13461 = VECTOR ( 'NONE', #5044, 1000.000000000000000 ) ;
#13462 = DIRECTION ( 'NONE',  ( 1.000000000000000000, 0.000000000000000000, 0.000000000000000000 ) ) ;
#13463 = DIRECTION ( 'NONE',  ( 0.000000000000000000, 0.000000000000000000, -1.000000000000000000 ) ) ;
#13464 = EDGE_CURVE ( 'NONE', #25155, #28714, #16879, .T. ) ;
#13465 = ORIENTED_EDGE ( 'NONE', *, *, #1825, .T. ) ;
#13466 = EDGE_CURVE ( 'NONE', #12285, #8898, #1598, .T. ) ;
#13467 = CIRCLE ( 'NONE', #8504, 9.084132297865673777 ) ;
#13468 = FACE_OUTER_BOUND ( 'NONE', #4369, .T. ) ;
#13469 = CARTESIAN_POINT ( 'NONE',  ( -32.68301789103641397, 8.668739453992939659, 41.18702913609079985 ) ) ;
#13470 = DIRECTION ( 'NONE',  ( 0.000000000000000000, 0.000000000000000000, -1.000000000000000000 ) ) ;
#13471 = ORIENTED_EDGE ( 'NONE', *, *, #4019, .F. ) ;
#13472 = ORIENTED_EDGE ( 'NONE', *, *, #30410, .F. ) ;
#13473 = CARTESIAN_POINT ( 'NONE',  ( -19.69701826448871174, 3.468437286170584777, 6.386539667786103713 ) ) ;
#13474 = DIRECTION ( 'NONE',  ( -1.000000000000000000, 0.000000000000000000, 0.000000000000000000 ) ) ;
#13475 = EDGE_LOOP ( 'NONE', ( #4083, #12445, #13954, #29456 ) ) ;
#13476 = CARTESIAN_POINT ( 'NONE',  ( -0.6570508600772840824, -19.98920419113417069, 6.518927109361846384 ) ) ;
#13477 = DIRECTION ( 'NONE',  ( 1.000000000000000000, 0.000000000000000000, 0.000000000000000000 ) ) ;
#13478 = CARTESIAN_POINT ( 'NONE',  ( 5.130938270761610021, -7.974144905643801629, 21.50000000000000000 ) ) ;
#13479 = DIRECTION ( 'NONE',  ( -0.000000000000000000, -0.000000000000000000, -1.000000000000000000 ) ) ;
#13480 = AXIS2_PLACEMENT_3D ( 'NONE', #21375, #14359, #12 ) ;
#13481 = CARTESIAN_POINT ( 'NONE',  ( -5.694318326875605685, 16.07090250511087248, 18.35718225375110180 ) ) ;
#13482 = CARTESIAN_POINT ( 'NONE',  ( 32.60829997825920401, -13.18983524832148113, 39.84356070656651383 ) ) ;
#13483 = CARTESIAN_POINT ( 'NONE',  ( 1.797484530300063721, -16.98352104300882814, 6.560937769032974209 ) ) ;
#13484 = DIRECTION ( 'NONE',  ( -1.000000000000000000, 0.000000000000000000, 0.000000000000000000 ) ) ;
#13485 = ORIENTED_EDGE ( 'NONE', *, *, #6728, .F. ) ;
#13486 = CARTESIAN_POINT ( 'NONE',  ( 0.000000000000000000, 0.000000000000000000, 1.500000000000001332 ) ) ;
#13487 = FACE_OUTER_BOUND ( 'NONE', #13981, .T. ) ;
#13488 = CARTESIAN_POINT ( 'NONE',  ( -5.292460272911076125, 16.19569186419612805, 7.626437579292365321 ) ) ;
#13489 = CARTESIAN_POINT ( 'NONE',  ( 0.3570196857253507550, 9.540868182094909500, 1.474731560294324284 ) ) ;
#13490 = DIRECTION ( 'NONE',  ( -1.000000000000000000, 0.000000000000000000, 0.000000000000000000 ) ) ;
#13491 = ORIENTED_EDGE ( 'NONE', *, *, #3160, .T. ) ;
#13492 = FACE_BOUND ( 'NONE', #18595, .T. ) ;
#13493 = CARTESIAN_POINT ( 'NONE',  ( 12.56641067637329812, 40.32935944495179115, -1.500000000000000000 ) ) ;
#13494 = CARTESIAN_POINT ( 'NONE',  ( 21.25638073752607227, -35.66179139336605175, 29.47302916183132027 ) ) ;
#13495 = LINE ( 'NONE', #4119, #3186 ) ;
#13496 = EDGE_LOOP ( 'NONE', ( #17952, #3344, #18418, #23114 ) ) ;
#13497 = CIRCLE ( 'NONE', #26437, 20.00000000000000000 ) ;
#13498 = DIRECTION ( 'NONE',  ( 0.000000000000000000, 1.000000000000000000, 1.193512090021232842E-16 ) ) ;
#13499 = EDGE_CURVE ( 'NONE', #18116, #17044, #1563, .T. ) ;
#13500 = DIRECTION ( 'NONE',  ( -0.000000000000000000, -0.000000000000000000, 1.000000000000000000 ) ) ;
#13501 = EDGE_CURVE ( 'NONE', #6837, #11031, #4079, .T. ) ;
#13502 = CARTESIAN_POINT ( 'NONE',  ( -15.00000000000004086, 1.571475800653548713E-14, 92.49999999999998579 ) ) ;
#13503 = EDGE_CURVE ( 'NONE', #26303, #3168, #21251, .T. ) ;
#13504 = ORIENTED_EDGE ( 'NONE', *, *, #30184, .T. ) ;
#13505 = LINE ( 'NONE', #8195, #15828 ) ;
#13506 = CARTESIAN_POINT ( 'NONE',  ( -13.39580148490130540, -35.10399786391197807, 37.49999999996187228 ) ) ;
#13507 = ORIENTED_EDGE ( 'NONE', *, *, #1592, .F. ) ;
#13508 = CARTESIAN_POINT ( 'NONE',  ( 42.49999999999998579, -50.00000000000000000, 52.07879600563550326 ) ) ;
#13509 = CARTESIAN_POINT ( 'NONE',  ( -10.52279982399693559, -17.02885636288122129, 5.652196082364321583 ) ) ;
#13510 = CARTESIAN_POINT ( 'NONE',  ( 4.390207617113956573, -7.856594496258208160, 1.500000000000001332 ) ) ;
#13511 = CARTESIAN_POINT ( 'NONE',  ( 0.8597189258598725292, -17.02598424914432584, 18.34838970509067479 ) ) ;
#13512 = ORIENTED_EDGE ( 'NONE', *, *, #8916, .F. ) ;
#13513 = DIRECTION ( 'NONE',  ( 1.000000000000000000, 0.000000000000000000, 0.000000000000000000 ) ) ;
#13514 = DIRECTION ( 'NONE',  ( 0.000000000000000000, 1.000000000000000000, 0.000000000000000000 ) ) ;
#13515 = AXIS2_PLACEMENT_3D ( 'NONE', #18910, #23559, #26388 ) ;
#13516 = DIRECTION ( 'NONE',  ( -0.000000000000000000, -0.000000000000000000, -1.000000000000000000 ) ) ;
#13517 = CIRCLE ( 'NONE', #8034, 9.482273699623480212 ) ;
#13518 = CARTESIAN_POINT ( 'NONE',  ( -0.6237340761795794331, 8.999114229549594057, -1.500000000000000888 ) ) ;
#13519 =( BOUNDED_CURVE ( )  B_SPLINE_CURVE ( 3, ( #3493, #994, #3178, #12547 ),
 .UNSPECIFIED., .F., .T. ) 
 B_SPLINE_CURVE_WITH_KNOTS ( ( 4, 4 ),
 ( 2.399144907686414196, 2.730840413552699353 ),
 .UNSPECIFIED. ) 
 CURVE ( )  GEOMETRIC_REPRESENTATION_ITEM ( )  RATIONAL_B_SPLINE_CURVE ( ( 1.000000000000000000, 0.9908525036704132205, 0.9908525036704132205, 1.000000000000000000 ) ) 
 REPRESENTATION_ITEM ( '' )  );
#13520 = DIRECTION ( 'NONE',  ( 1.000000000000000000, 0.000000000000000000, 0.000000000000000000 ) ) ;
#13521 = CARTESIAN_POINT ( 'NONE',  ( 4.622016212553096359, -12.19167610014704906, 1.500000000000001332 ) ) ;
#13522 = DIRECTION ( 'NONE',  ( 0.000000000000000000, 1.000000000000000000, 0.000000000000000000 ) ) ;
#13523 = LINE ( 'NONE', #26831, #4432 ) ;
#13524 = LINE ( 'NONE', #29731, #27038 ) ;
#13525 = ORIENTED_EDGE ( 'NONE', *, *, #23837, .F. ) ;
#13526 = ORIENTED_EDGE ( 'NONE', *, *, #266, .F. ) ;
#13527 = DIRECTION ( 'NONE',  ( -0.000000000000000000, -0.000000000000000000, 1.000000000000000000 ) ) ;
#13528 = CARTESIAN_POINT ( 'NONE',  ( 32.74775157612609178, -27.21557300919356948, -19.50000000000000355 ) ) ;
#13529 = DIRECTION ( 'NONE',  ( 0.000000000000000000, -1.132880637372608986E-16, 1.000000000000000000 ) ) ;
#13530 = ORIENTED_EDGE ( 'NONE', *, *, #29982, .F. ) ;
#13531 = SHAPE_REPRESENTATION_RELATIONSHIP ( 'NONE' , 'NONE' ,  #23229, #5063 ) ;
#13532 = DIRECTION ( 'NONE',  ( -0.2817325568414293380, -0.9594929736144974797, 0.000000000000000000 ) ) ;
#13533 = CARTESIAN_POINT ( 'NONE',  ( 9.007774317138297349, -14.44244895400449558, 19.41069149716886955 ) ) ;
#13534 = EDGE_CURVE ( 'NONE', #14664, #18929, #11414, .T. ) ;
#13535 = ORIENTED_EDGE ( 'NONE', *, *, #24634, .T. ) ;
#13536 = VERTEX_POINT ( 'NONE', #893 ) ;
#13537 = CARTESIAN_POINT ( 'NONE',  ( -10.94076559809103699, -16.74260033555410843, 18.47110296274026098 ) ) ;
#13538 = CYLINDRICAL_SURFACE ( 'NONE', #16266, 0.7500000000000015543 ) ;
#13539 = AXIS2_PLACEMENT_3D ( 'NONE', #22956, #22808, #1746 ) ;
#13540 = CARTESIAN_POINT ( 'NONE',  ( -4.175048725057020960, -43.84342162469872051, -16.50000000000000355 ) ) ;
#13541 = CARTESIAN_POINT ( 'NONE',  ( -4.613788807593795838, 42.22795758926503851, 34.60590817694901489 ) ) ;
#13542 = EDGE_LOOP ( 'NONE', ( #18483, #24472, #17639, #19608 ) ) ;
#13543 = LINE ( 'NONE', #28023, #4366 ) ;
#13544 = EDGE_LOOP ( 'NONE', ( #24605, #19190 ) ) ;
#13545 = CARTESIAN_POINT ( 'NONE',  ( -1.073881485057738949, 0.9711784013061123266, 1.500000000000000000 ) ) ;
#13546 = CARTESIAN_POINT ( 'NONE',  ( 9.999999999999959144, 1.510243460696181139E-14, 1.500000000000000000 ) ) ;
#13547 = EDGE_LOOP ( 'NONE', ( #26772, #20754, #15697, #23996, #11997, #28388, #10535, #28999, #11533 ) ) ;
#13548 = DIRECTION ( 'NONE',  ( -0.000000000000000000, -0.000000000000000000, 1.000000000000000000 ) ) ;
#13549 = SURFACE_SIDE_STYLE ('',( #25396 ) ) ;
#13550 = AXIS2_PLACEMENT_3D ( 'NONE', #18224, #16034, #24931 ) ;
#13551 = CARTESIAN_POINT ( 'NONE',  ( 17.29228478519430112, -38.19350839570123668, 29.22794746440463243 ) ) ;
#13552 = FACE_BOUND ( 'NONE', #6560, .T. ) ;
#13553 = CARTESIAN_POINT ( 'NONE',  ( 24.85846090629200233, -6.933313039714898096, 49.19304184080755959 ) ) ;
#13554 = LINE ( 'NONE', #6214, #5568 ) ;
#13555 = CARTESIAN_POINT ( 'NONE',  ( -17.05537006572907899, 0.7816414089123745468, 18.82680253904184298 ) ) ;
#13556 = CARTESIAN_POINT ( 'NONE',  ( 19.62935297797556089, -3.832558109936519575, 24.50000000000000000 ) ) ;
#13557 = ORIENTED_EDGE ( 'NONE', *, *, #2658, .T. ) ;
#13558 = CARTESIAN_POINT ( 'NONE',  ( 10.52132926683979974, -13.44281371605820041, 18.73743063545763121 ) ) ;
#13559 = AXIS2_PLACEMENT_3D ( 'NONE', #28345, #21616, #28798 ) ;
#13560 = CARTESIAN_POINT ( 'NONE',  ( 15.85884089648730289, -35.55173462727349687, 34.80090346875809360 ) ) ;
#13561 = ORIENTED_EDGE ( 'NONE', *, *, #27792, .F. ) ;
#13562 = ORIENTED_EDGE ( 'NONE', *, *, #17818, .F. ) ;
#13563 = EDGE_CURVE ( 'NONE', #26022, #22885, #27846, .T. ) ;
#13564 = DIRECTION ( 'NONE',  ( 1.000000000000000000, 0.000000000000000000, 0.000000000000000000 ) ) ;
#13565 = ORIENTED_EDGE ( 'NONE', *, *, #30149, .T. ) ;
#13566 = CARTESIAN_POINT ( 'NONE',  ( 0.000000000000000000, 12.18947652193948272, -87.50000000000000000 ) ) ;
#13567 = ADVANCED_FACE ( 'NONE', ( #12919 ), #14870, .F. ) ;
#13568 = LINE ( 'NONE', #28050, #4704 ) ;
#13569 = EDGE_CURVE ( 'NONE', #28974, #9226, #23692, .T. ) ;
#13570 = CARTESIAN_POINT ( 'NONE',  ( 24.35970437652574105, 13.37404834226503958, 47.21042702067963859 ) ) ;
#13571 = ORIENTED_EDGE ( 'NONE', *, *, #1417, .T. ) ;
#13572 = EDGE_CURVE ( 'NONE', #30200, #6265, #9912, .T. ) ;
#13573 = AXIS2_PLACEMENT_3D ( 'NONE', #925, #1240, #178 ) ;
#13574 = CYLINDRICAL_SURFACE ( 'NONE', #4770, 2.000000000000001776 ) ;
#13575 = DIRECTION ( 'NONE',  ( -0.000000000000000000, -0.000000000000000000, -1.000000000000000000 ) ) ;
#13576 = ORIENTED_EDGE ( 'NONE', *, *, #19285, .F. ) ;
#13577 = CARTESIAN_POINT ( 'NONE',  ( -13.68208811019134785, -10.53240720452297374, 24.50000000000000000 ) ) ;
#13578 = ORIENTED_EDGE ( 'NONE', *, *, #6155, .T. ) ;
#13579 = EDGE_CURVE ( 'NONE', #26950, #20068, #27252, .T. ) ;
#13580 = DIRECTION ( 'NONE',  ( -0.000000000000000000, -0.000000000000000000, 1.000000000000000000 ) ) ;
#13581 = AXIS2_PLACEMENT_3D ( 'NONE', #14865, #15165, #24380 ) ;
#13582 = VERTEX_POINT ( 'NONE', #27564 ) ;
#13583 = ADVANCED_FACE ( 'NONE', ( #29910 ), #20531, .F. ) ;
#13584 = ORIENTED_EDGE ( 'NONE', *, *, #15067, .T. ) ;
#13585 = EDGE_CURVE ( 'NONE', #6674, #21864, #6031, .T. ) ;
#13586 = CARTESIAN_POINT ( 'NONE',  ( 3.728348255937731448, 16.64288108867316751, 7.603368798681074736 ) ) ;
#13587 = CARTESIAN_POINT ( 'NONE',  ( 32.28307784207223108, 8.475829241206289666, 41.62281023987511475 ) ) ;
#13588 = CARTESIAN_POINT ( 'NONE',  ( -40.05104235265675783, -2.353288714454540020, -6.500000000000000888 ) ) ;
#13589 = VERTEX_POINT ( 'NONE', #3853 ) ;
#13590 = CARTESIAN_POINT ( 'NONE',  ( -35.76481447503397959, 5.202797454133647470, 27.50000000000001066 ) ) ;
#13591 = DIRECTION ( 'NONE',  ( -0.000000000000000000, 0.000000000000000000, 1.000000000000000000 ) ) ;
#13592 = DIRECTION ( 'NONE',  ( 0.000000000000000000, 0.000000000000000000, -1.000000000000000000 ) ) ;
#13593 = ORIENTED_EDGE ( 'NONE', *, *, #4058, .T. ) ;
#13594 = VECTOR ( 'NONE', #24434, 1000.000000000000000 ) ;
#13595 = CARTESIAN_POINT ( 'NONE',  ( 0.000000000000000000, -5.590849009245238754, 1.500000000000000000 ) ) ;
#13596 = CARTESIAN_POINT ( 'NONE',  ( 18.01689225005682005, -8.724154469992754457, 7.272049892295485485 ) ) ;
#13597 = CARTESIAN_POINT ( 'NONE',  ( -15.64089046717303333, 12.49323067438738555, 5.749491821935610147 ) ) ;
#13598 = CARTESIAN_POINT ( 'NONE',  ( 5.231931633751615074, 19.32210152104737233, 20.34789198813115263 ) ) ;
#13599 = ORIENTED_EDGE ( 'NONE', *, *, #24461, .T. ) ;
#13600 = ORIENTED_EDGE ( 'NONE', *, *, #6309, .F. ) ;
#13601 = DIRECTION ( 'NONE',  ( 0.9594929736144992560, 0.2817325568414232317, 0.000000000000000000 ) ) ;
#13602 = ADVANCED_FACE ( 'NONE', ( #29593 ), #22559, .F. ) ;
#13603 = CYLINDRICAL_SURFACE ( 'NONE', #28068, 21.71568325578132530 ) ;
#13604 = EDGE_CURVE ( 'NONE', #1725, #27956, #21862, .T. ) ;
#13605 = CARTESIAN_POINT ( 'NONE',  ( -5.103338407348686268, 19.35644909001343805, 18.90679857307105749 ) ) ;
#13606 = LINE ( 'NONE', #30121, #29709 ) ;
#13607 = CARTESIAN_POINT ( 'NONE',  ( -23.21352257770656990, 10.78826658734919519, 45.15942333309111234 ) ) ;
#13608 = EDGE_CURVE ( 'NONE', #23147, #2256, #27714, .T. ) ;
#13609 = CARTESIAN_POINT ( 'NONE',  ( -26.80246859415415273, 7.028748154183637631, -1.499999999999999556 ) ) ;
#13610 = CARTESIAN_POINT ( 'NONE',  ( -6.414842543015754295, -17.06554576617236307, -1.500000000000000000 ) ) ;
#13611 = B_SPLINE_CURVE_WITH_KNOTS ( 'NONE', 3,
 ( #29947, #27606, #11215, #18855 ),
 .UNSPECIFIED., .F., .F.,
 ( 4, 4 ),
 ( 3.018024802580205417E-07, 0.007932103453629116285 ),
 .UNSPECIFIED. ) ;
#13612 = ORIENTED_EDGE ( 'NONE', *, *, #12471, .T. ) ;
#13613 = EDGE_CURVE ( 'NONE', #29162, #549, #8691, .T. ) ;
#13614 = CARTESIAN_POINT ( 'NONE',  ( 1.342668813586973764, -19.95494644892924185, 6.392525840300336881 ) ) ;
#13615 = CARTESIAN_POINT ( 'NONE',  ( 14.20168120032941594, 14.08243226175162555, 19.08830981656263504 ) ) ;
#13616 = DIRECTION ( 'NONE',  ( 0.000000000000000000, 0.000000000000000000, 1.000000000000000000 ) ) ;
#13617 = ORIENTED_EDGE ( 'NONE', *, *, #5907, .F. ) ;
#13618 = CYLINDRICAL_SURFACE ( 'NONE', #24758, 7.500000000000013323 ) ;
#13619 = AXIS2_PLACEMENT_3D ( 'NONE', #16029, #7556, #25854 ) ;
#13620 = ORIENTED_EDGE ( 'NONE', *, *, #20899, .T. ) ;
#13621 = EDGE_CURVE ( 'NONE', #20574, #26441, #6426, .T. ) ;
#13622 = CARTESIAN_POINT ( 'NONE',  ( -8.197313248159920462, 3.914781618004780306, 21.50000000000000000 ) ) ;
#13623 = AXIS2_PLACEMENT_3D ( 'NONE', #16423, #18616, #27976 ) ;
#13624 = UNCERTAINTY_MEASURE_WITH_UNIT (LENGTH_MEASURE( 1.000000000000000082E-05 ), #14769, 'distance_accuracy_value', 'NONE');
#13625 = CARTESIAN_POINT ( 'NONE',  ( -19.87500762523393050, 2.235808837979145203, 20.32200205377525393 ) ) ;
#13626 = VERTEX_POINT ( 'NONE', #25377 ) ;
#13627 = CARTESIAN_POINT ( 'NONE',  ( -7.827050521741846012, 5.352643706120544742, 21.50000000000000000 ) ) ;
#13628 = CARTESIAN_POINT ( 'NONE',  ( 9.913295469302216389, 49.01253027209195778, -66.29974890224383444 ) ) ;
#13629 = CARTESIAN_POINT ( 'NONE',  ( -24.03057240117691862, 26.57182937991348481, 1.500000000000001332 ) ) ;
#13630 = FACE_OUTER_BOUND ( 'NONE', #7261, .T. ) ;
#13631 = DIRECTION ( 'NONE',  ( -0.000000000000000000, -0.000000000000000000, 1.000000000000000000 ) ) ;
#13632 = CARTESIAN_POINT ( 'NONE',  ( 49.99999999999998579, 90.00000000000001421, 52.49999999999999289 ) ) ;
#13633 = CARTESIAN_POINT ( 'NONE',  ( 1.512395753140456378, -17.00118538373299160, 5.951255046771932733 ) ) ;
#13634 = ORIENTED_EDGE ( 'NONE', *, *, #30575, .T. ) ;
#13635 = EDGE_CURVE ( 'NONE', #1968, #24589, #15858, .T. ) ;
#13636 = EDGE_CURVE ( 'NONE', #18929, #14664, #447, .T. ) ;
#13637 = CARTESIAN_POINT ( 'NONE',  ( -70.00000000000000000, -70.00000000000000000, 12.49999999999999112 ) ) ;
#13638 = FACE_OUTER_BOUND ( 'NONE', #3315, .T. ) ;
#13639 = ORIENTED_EDGE ( 'NONE', *, *, #20251, .T. ) ;
#13640 = DIRECTION ( 'NONE',  ( -0.000000000000000000, -0.000000000000000000, 1.000000000000000000 ) ) ;
#13641 = AXIS2_PLACEMENT_3D ( 'NONE', #13710, #23196, #22594 ) ;
#13642 = CARTESIAN_POINT ( 'NONE',  ( -14.87733195063809255, -8.360270151095061664, 18.56793045041961321 ) ) ;
#13643 = CIRCLE ( 'NONE', #28070, 15.00000000000000000 ) ;
#13644 = DIRECTION ( 'NONE',  ( 0.000000000000000000, 0.000000000000000000, 1.000000000000000000 ) ) ;
#13645 = VERTEX_POINT ( 'NONE', #3547 ) ;
#13646 = FACE_BOUND ( 'NONE', #5407, .T. ) ;
#13647 = DIRECTION ( 'NONE',  ( -1.369518533665900065E-16, 0.000000000000000000, -1.000000000000000000 ) ) ;
#13648 = CARTESIAN_POINT ( 'NONE',  ( 35.05587750292992411, -18.67595856107542218, 34.76255166971075994 ) ) ;
#13649 = CARTESIAN_POINT ( 'NONE',  ( 69.99999999999998579, 50.00000000000000000, 12.49999999999999112 ) ) ;
#13650 = ORIENTED_EDGE ( 'NONE', *, *, #2304, .F. ) ;
#13651 = CARTESIAN_POINT ( 'NONE',  ( -13.22505861668333083, 42.10773672057167261, -19.50000000000000355 ) ) ;
#13652 = CARTESIAN_POINT ( 'NONE',  ( 6.482337650448408262, 6.364020599487814955, 21.50000000000000000 ) ) ;
#13653 = VERTEX_POINT ( 'NONE', #23014 ) ;
#13654 = B_SPLINE_SURFACE_WITH_KNOTS ( 'NONE', 3, 1, ( 
 ( #4299, #25986 ),
 ( #11957, #30498 ),
 ( #23782, #11633 ),
 ( #4614, #30811 ),
 ( #18816, #21125 ),
 ( #26127, #18514 ),
 ( #2263, #30644 ),
 ( #7256, #18659 ),
 ( #9291, #90 ),
 ( #21289, #2114 ),
 ( #28634, #28335 ),
 ( #20836, #9000 ),
 ( #14262, #11784 ),
 ( #28014, #4471 ),
 ( #26286, #14114 ),
 ( #18974, #1819 ),
 ( #23621, #2434 ),
 ( #6646, #7112 ),
 ( #4758, #13978 ),
 ( #9607, #19116 ),
 ( #11342, #16163 ),
 ( #13829, #28164 ),
 ( #23331, #1971 ),
 ( #11493, #21601 ),
 ( #15041, #24405 ),
 ( #239, #12569 ),
 ( #542, #9750 ),
 ( #12722, #17234 ),
 ( #16932, #26920 ),
 ( #24554, #3199 ),
 ( #26759, #5390 ) ),
 .UNSPECIFIED., .F., .F., .F.,
 ( 4, 3, 3, 3, 3, 3, 3, 3, 3, 3, 4 ),
 ( 2, 2 ),
 ( 0.000000000000000000, 0.05425176834609614362, 0.1085332949128348518, 0.1623767749169379715, 0.2157504826133058717, 0.2688657508888169789, 0.3218907763505471364, 0.3749548578363334772, 0.4282048033836237666, 0.4818374082110496448, 0.4999999999131654604 ),
 ( 0.000000000000000000, 1.000000000000000000 ),
 .UNSPECIFIED. ) ;
#13655 = AXIS2_PLACEMENT_3D ( 'NONE', #26110, #4740, #21430 ) ;
#13656 = CARTESIAN_POINT ( 'NONE',  ( -7.734930024145167060, -41.68293636675864633, 34.59191748876874328 ) ) ;
#13657 = ORIENTED_EDGE ( 'NONE', *, *, #4054, .T. ) ;
#13658 = FACE_OUTER_BOUND ( 'NONE', #16957, .T. ) ;
#13659 = CIRCLE ( 'NONE', #19118, 1.447898107987198646 ) ;
#13660 = AXIS2_PLACEMENT_3D ( 'NONE', #22216, #5231, #5688 ) ;
#13661 = CARTESIAN_POINT ( 'NONE',  ( -10.39297074171569690, -17.10854403003571989, 5.661398277488802755 ) ) ;
#13662 = DIRECTION ( 'NONE',  ( -0.000000000000000000, -0.000000000000000000, 1.000000000000000000 ) ) ;
#13663 = FACE_OUTER_BOUND ( 'NONE', #27733, .T. ) ;
#13664 = ORIENTED_EDGE ( 'NONE', *, *, #15307, .T. ) ;
#13665 = CARTESIAN_POINT ( 'NONE',  ( 0.000000000000000000, 0.000000000000000000, 0.000000000000000000 ) ) ;
#13666 = CARTESIAN_POINT ( 'NONE',  ( 16.58213327075030818, 4.067275193340576855, 6.147510495896841398 ) ) ;
#13667 = CARTESIAN_POINT ( 'NONE',  ( -33.42925964089141644, -11.06161099612212695, 39.78814634291941843 ) ) ;
#13668 = B_SPLINE_CURVE_WITH_KNOTS ( 'NONE', 3,
 ( #16694, #9519, #28402, #5144, #19037, #21831, #12332, #24004 ),
 .UNSPECIFIED., .F., .F.,
 ( 4, 2, 2, 4 ),
 ( 0.02518894967656377937, 0.02782118485464665780, 0.02913730244368809702, 0.03045342003272953624 ),
 .UNSPECIFIED. ) ;
#13669 = DIRECTION ( 'NONE',  ( -0.000000000000000000, -0.000000000000000000, -1.000000000000000000 ) ) ;
#13670 = DIRECTION ( 'NONE',  ( -0.000000000000000000, -0.000000000000000000, -1.000000000000000000 ) ) ;
#13671 = CARTESIAN_POINT ( 'NONE',  ( 0.000000000000000000, 0.000000000000000000, 92.49999999999998579 ) ) ;
#13672 = CARTESIAN_POINT ( 'NONE',  ( 3.537840656726939592, 16.69140805415182527, 18.45571264222803975 ) ) ;
#13673 = CARTESIAN_POINT ( 'NONE',  ( 8.999114229549594057, -0.1262659238204522361, -1.500000000000001776 ) ) ;
#13674 = CARTESIAN_POINT ( 'NONE',  ( -18.41515300997269122, -7.848447721146241562, 19.87181966307587544 ) ) ;
#13675 = CARTESIAN_POINT ( 'NONE',  ( 0.3563104543936387314, 9.539178283403856540, -1.477658550686871575 ) ) ;
#13676 = VERTEX_POINT ( 'NONE', #25530 ) ;
#13677 = ORIENTED_EDGE ( 'NONE', *, *, #7277, .F. ) ;
#13678 = CYLINDRICAL_SURFACE ( 'NONE', #502, 4.999999999999997335 ) ;
#13679 = VECTOR ( 'NONE', #23511, 1000.000000000000000 ) ;
#13680 = CARTESIAN_POINT ( 'NONE',  ( 0.000000000000000000, 44.39187623478217404, -19.50000000000000355 ) ) ;
#13681 = DIRECTION ( 'NONE',  ( 0.000000000000000000, 1.000000000000000000, 0.000000000000000000 ) ) ;
#13682 = ORIENTED_EDGE ( 'NONE', *, *, #20978, .T. ) ;
#13683 = DIRECTION ( 'NONE',  ( 0.000000000000000000, 0.000000000000000000, 1.000000000000000000 ) ) ;
#13684 = DIRECTION ( 'NONE',  ( 1.000000000000000000, 0.000000000000000000, 0.000000000000000000 ) ) ;
#13685 = CARTESIAN_POINT ( 'NONE',  ( -24.03057240117690441, -26.57182937991348481, 1.500000000000001332 ) ) ;
#13686 = ORIENTED_EDGE ( 'NONE', *, *, #26117, .T. ) ;
#13687 = CARTESIAN_POINT ( 'NONE',  ( -19.81665592078379490, 2.832673353242748604, 5.701226463332907279 ) ) ;
#13688 = CARTESIAN_POINT ( 'NONE',  ( 15.52089561533224327, 12.61365839305099179, 6.913388067999413522 ) ) ;
#13689 = DIRECTION ( 'NONE',  ( -0.000000000000000000, -0.000000000000000000, 1.000000000000000000 ) ) ;
#13690 = ORIENTED_EDGE ( 'NONE', *, *, #29510, .T. ) ;
#13691 = CARTESIAN_POINT ( 'NONE',  ( -0.1262659238204836554, -8.999114229549588728, -1.500000000000002665 ) ) ;
#13692 = VERTEX_POINT ( 'NONE', #6193 ) ;
#13693 = CARTESIAN_POINT ( 'NONE',  ( -3.683253992019774881, 8.303920738747249786, -1.500000000000000888 ) ) ;
#13694 = PLANE ( 'NONE',  #28266 ) ;
#13695 = ORIENTED_EDGE ( 'NONE', *, *, #14508, .F. ) ;
#13696 = SHAPE_REPRESENTATION ( 'Housing  Cover Cap', ( #7396 ), #10404 ) ;
#13697 = CARTESIAN_POINT ( 'NONE',  ( -7.538175180318458679, -5.069257791428355198, 21.50000000000000000 ) ) ;
#13698 = DIRECTION ( 'NONE',  ( 0.000000000000000000, 1.000000000000000000, 0.000000000000000000 ) ) ;
#13699 = CARTESIAN_POINT ( 'NONE',  ( 8.321693349542481855, -43.14082846441630892, -16.50000000000000355 ) ) ;
#13700 = CYLINDRICAL_SURFACE ( 'NONE', #11310, 1.999999999999998224 ) ;
#13701 = FACE_OUTER_BOUND ( 'NONE', #24973, .T. ) ;
#13702 = DIRECTION ( 'NONE',  ( 0.000000000000000000, 0.000000000000000000, 1.000000000000000000 ) ) ;
#13703 = CARTESIAN_POINT ( 'NONE',  ( -19.88720069594608475, 2.282442057551329562, 20.32367522806703874 ) ) ;
#13704 = CARTESIAN_POINT ( 'NONE',  ( 5.141690706682880752, -7.488956955540417404, 21.50000000000000000 ) ) ;
#13705 = VERTEX_POINT ( 'NONE', #1666 ) ;
#13706 = CARTESIAN_POINT ( 'NONE',  ( -6.385759811051640256, 15.83451745216270901, 6.147510495896842286 ) ) ;
#13707 = CARTESIAN_POINT ( 'NONE',  ( 11.52197458429824550, -37.50933785548061650, 34.80090346875809360 ) ) ;
#13708 = EDGE_LOOP ( 'NONE', ( #21936, #10702, #13057, #18023 ) ) ;
#13709 = EDGE_LOOP ( 'NONE', ( #12414, #16726, #7587, #3055 ) ) ;
#13710 = CARTESIAN_POINT ( 'NONE',  ( 8.999114229549594057, -0.1262659238204522361, 1.500000000000001332 ) ) ;
#13711 = DIRECTION ( 'NONE',  ( 0.000000000000000000, 0.000000000000000000, -1.000000000000000000 ) ) ;
#13712 = ORIENTED_EDGE ( 'NONE', *, *, #10538, .F. ) ;
#13713 = CARTESIAN_POINT ( 'NONE',  ( 10.16054539467770113, 13.96046037420044961, 1.500000000000000000 ) ) ;
#13714 = PLANE ( 'NONE',  #26372 ) ;
#13715 = ORIENTED_EDGE ( 'NONE', *, *, #13621, .F. ) ;
#13716 = FACE_OUTER_BOUND ( 'NONE', #22421, .T. ) ;
#13717 = DIRECTION ( 'NONE',  ( -1.000000000000000000, 0.000000000000000000, 0.000000000000000000 ) ) ;
#13718 = ORIENTED_EDGE ( 'NONE', *, *, #20062, .F. ) ;
#13719 = CARTESIAN_POINT ( 'NONE',  ( 25.47847050916410439, -26.57182937991349903, 24.50000000000000000 ) ) ;
#13720 = ORIENTED_EDGE ( 'NONE', *, *, #2378, .T. ) ;
#13721 = DIRECTION ( 'NONE',  ( -0.000000000000000000, -0.000000000000000000, 1.000000000000000000 ) ) ;
#13722 = ORIENTED_EDGE ( 'NONE', *, *, #29867, .T. ) ;
#13723 = EDGE_LOOP ( 'NONE', ( #24408, #24690 ) ) ;
#13724 = EDGE_CURVE ( 'NONE', #24236, #11596, #21839, .T. ) ;
#13725 = DIRECTION ( 'NONE',  ( -0.000000000000000000, -0.000000000000000000, -1.000000000000000000 ) ) ;
#13726 = DIRECTION ( 'NONE',  ( 1.000000000000000000, 0.000000000000000000, 0.000000000000000000 ) ) ;
#13727 = AXIS2_PLACEMENT_3D ( 'NONE', #13135, #8301, #27332 ) ;
#13728 = CARTESIAN_POINT ( 'NONE',  ( -34.13832859401788511, 12.80067323710188276, 27.50000000000001776 ) ) ;
#13729 = CYLINDRICAL_SURFACE ( 'NONE', #8362, 0.7500000000000004441 ) ;
#13730 = CARTESIAN_POINT ( 'NONE',  ( 19.85280965686022014, 2.565335765644451094, 20.12545155307891065 ) ) ;
#13731 = EDGE_LOOP ( 'NONE', ( #14488, #8183, #11425, #30734 ) ) ;
#13732 = EDGE_CURVE ( 'NONE', #21892, #14781, #25837, .T. ) ;
#13733 = CARTESIAN_POINT ( 'NONE',  ( -16.87560513830565867, 2.281487909151088012, 20.12545155307891065 ) ) ;
#13734 = DIRECTION ( 'NONE',  ( 1.156482317317870344E-15, 1.000000000000000000, 0.000000000000000000 ) ) ;
#13735 = CARTESIAN_POINT ( 'NONE',  ( 37.99999999999999289, 70.00000000000000000, -34.50000000000000000 ) ) ;
#13736 = CARTESIAN_POINT ( 'NONE',  ( 3.077027262763119442, 16.79827892558873614, 19.14333282897057842 ) ) ;
#13737 = ORIENTED_EDGE ( 'NONE', *, *, #17549, .T. ) ;
#13738 = ORIENTED_EDGE ( 'NONE', *, *, #1590, .F. ) ;
#13739 = DIRECTION ( 'NONE',  ( 0.000000000000000000, 0.000000000000000000, -1.000000000000000000 ) ) ;
#13740 = DIRECTION ( 'NONE',  ( -1.000000000000000000, 0.000000000000000000, 0.000000000000000000 ) ) ;
#13741 = CARTESIAN_POINT ( 'NONE',  ( 14.87898868866547097, 13.36471831362575102, 18.34798005863227388 ) ) ;
#13742 = CARTESIAN_POINT ( 'NONE',  ( 39.99999999999998579, 80.00000000000001421, 47.49999999999999289 ) ) ;
#13743 = CARTESIAN_POINT ( 'NONE',  ( -4.163336342344337027E-14, 1.387778780781445676E-14, 37.50000000000000000 ) ) ;
#13744 = ADVANCED_FACE ( 'NONE', ( #15694 ), #13219, .F. ) ;
#13745 = EDGE_CURVE ( 'NONE', #5492, #2392, #25369, .T. ) ;
#13746 = DIRECTION ( 'NONE',  ( 1.000000000000000000, 0.000000000000000000, 0.000000000000000000 ) ) ;
#13747 = VERTEX_POINT ( 'NONE', #30360 ) ;
#13748 = CARTESIAN_POINT ( 'NONE',  ( -19.94516883457951550, 1.701953382846943086, 6.041646659195333058 ) ) ;
#13749 = CYLINDRICAL_SURFACE ( 'NONE', #22184, 7.500000000000000000 ) ;
#13750 = LINE ( 'NONE', #16392, #8495 ) ;
#13751 = ORIENTED_EDGE ( 'NONE', *, *, #29759, .F. ) ;
#13752 = CIRCLE ( 'NONE', #17729, 3.000000000000002665 ) ;
#13753 = DIRECTION ( 'NONE',  ( 1.000000000000000000, 0.000000000000000000, 0.000000000000000000 ) ) ;
#13754 = ORIENTED_EDGE ( 'NONE', *, *, #17730, .T. ) ;
#13755 = DIRECTION ( 'NONE',  ( -0.9898214418809326842, 0.1423148382732851158, -0.000000000000000000 ) ) ;
#13756 = CARTESIAN_POINT ( 'NONE',  ( -23.27838111883973227, 36.10018642694448943, -16.50000600000000262 ) ) ;
#13757 = VERTEX_POINT ( 'NONE', #28484 ) ;
#13758 = CARTESIAN_POINT ( 'NONE',  ( -0.1522245795255685596, -19.99979613760742225, 5.775318986477954830 ) ) ;
#13759 = APPLICATION_CONTEXT ( 'automotive_design' ) ;
#13760 = EDGE_CURVE ( 'NONE', #15501, #26631, #9402, .T. ) ;
#13761 = CARTESIAN_POINT ( 'NONE',  ( 1.977841715212117935, 49.97021211411167485, -40.09845259988525612 ) ) ;
#13762 = ADVANCED_FACE ( 'NONE', ( #16769 ), #13654, .T. ) ;
#13763 = FACE_OUTER_BOUND ( 'NONE', #6112, .T. ) ;
#13764 = DIRECTION ( 'NONE',  ( -0.000000000000000000, -0.000000000000000000, -1.000000000000000000 ) ) ;
#13765 = CARTESIAN_POINT ( 'NONE',  ( 39.99999999999998579, 80.00000000000001421, 52.49999999999999289 ) ) ;
#13766 = AXIS2_PLACEMENT_3D ( 'NONE', #1073, #19947, #29464 ) ;
#13767 = DIRECTION ( 'NONE',  ( -1.000000000000000000, 0.000000000000000000, 0.000000000000000000 ) ) ;
#13768 = CARTESIAN_POINT ( 'NONE',  ( -4.163336342344337027E-14, 1.387778780781445676E-14, 51.25735931288069480 ) ) ;
#13769 = VERTEX_POINT ( 'NONE', #7735 ) ;
#13770 = ADVANCED_FACE ( 'NONE', ( #24093, #2743, #2898 ), #13918, .T. ) ;
#13771 = DIRECTION ( 'NONE',  ( 0.000000000000000000, -1.132880637372608986E-16, 1.000000000000000000 ) ) ;
#13772 = DIRECTION ( 'NONE',  ( 1.000000000000000000, 0.000000000000000000, 0.000000000000000000 ) ) ;
#13773 = EDGE_LOOP ( 'NONE', ( #16021, #20438, #7433, #9855 ) ) ;
#13774 = EDGE_CURVE ( 'NONE', #15313, #23863, #15399, .T. ) ;
#13775 = CARTESIAN_POINT ( 'NONE',  ( 0.000000000000000000, 0.000000000000000000, 1.500000000000001332 ) ) ;
#13776 = CARTESIAN_POINT ( 'NONE',  ( -14.74412167020460274, -8.612351851578502249, 18.92976555901915603 ) ) ;
#13777 = B_SPLINE_CURVE_WITH_KNOTS ( 'NONE', 3,
 ( #5207, #29379, #3324, #20011, #24852, #8019, #3489, #22494, #1140, #10652, #17051 ),
 .UNSPECIFIED., .F., .F.,
 ( 4, 1, 1, 1, 1, 1, 1, 1, 4 ),
 ( 3.141592653589793116, 3.534291735288517255, 3.926990816987241395, 4.319689898685965090, 4.712388980384689674, 5.105088062083414258, 5.497787143782137953, 5.890486225480861648, 6.283185307179586232 ),
 .UNSPECIFIED. ) ;
#13778 = ADVANCED_FACE ( 'NONE', ( #12251 ), #17398, .F. ) ;
#13779 = AXIS2_PLACEMENT_3D ( 'NONE', #11198, #1990, #23494 ) ;
#13780 = FILL_AREA_STYLE_COLOUR ( '', #8803 ) ;
#13781 = VECTOR ( 'NONE', #22029, 1000.000000000000000 ) ;
#13782 = CARTESIAN_POINT ( 'NONE',  ( -26.80246859415415273, 7.028748154183637631, -1.499999999999999556 ) ) ;
#13783 = ORIENTED_EDGE ( 'NONE', *, *, #11336, .T. ) ;
#13784 = DIRECTION ( 'NONE',  ( -1.000000000000000000, 0.000000000000000000, 0.000000000000000000 ) ) ;
#13785 = EDGE_CURVE ( 'NONE', #11965, #353, #14895, .T. ) ;
#13786 = DIRECTION ( 'NONE',  ( 0.9898214418809326842, 0.1423148382732852268, -0.000000000000000000 ) ) ;
#13787 = CARTESIAN_POINT ( 'NONE',  ( 16.30589577393280720, -38.63578930953848101, 34.53468016319318679 ) ) ;
#13788 = CARTESIAN_POINT ( 'NONE',  ( -6.908049759614255159, 18.76916546752687509, 6.919864475265776527 ) ) ;
#13789 = EDGE_LOOP ( 'NONE', ( #7852, #18078, #23903, #14128 ) ) ;
#13790 = CARTESIAN_POINT ( 'NONE',  ( 37.16608720827707657, -51.86186943028246787, 12.49999999999999112 ) ) ;
#13791 = VECTOR ( 'NONE', #13164, 1000.000000000000000 ) ;
#13792 = CARTESIAN_POINT ( 'NONE',  ( 10.11202017158463917, -41.14070756921186955, -1.500000000000000000 ) ) ;
#13793 = DIRECTION ( 'NONE',  ( -0.000000000000000000, -0.000000000000000000, 1.000000000000000000 ) ) ;
#13794 = VERTEX_POINT ( 'NONE', #10377 ) ;
#13795 = AXIS2_PLACEMENT_3D ( 'NONE', #2206, #28418, #19656 ) ;
#13796 = CARTESIAN_POINT ( 'NONE',  ( -25.23756106473024730, -11.43858098102957577, -16.50000000000000000 ) ) ;
#13797 = ORIENTED_EDGE ( 'NONE', *, *, #22726, .F. ) ;
#13798 = CARTESIAN_POINT ( 'NONE',  ( -24.75988009833579540, -7.043597625963918141, 45.01551998635112994 ) ) ;
#13799 = EDGE_CURVE ( 'NONE', #29438, #3254, #4460, .T. ) ;
#13800 = EDGE_CURVE ( 'NONE', #25790, #25448, #19891, .T. ) ;
#13801 = CIRCLE ( 'NONE', #10823, 29.99999999999928946 ) ;
#13802 = CIRCLE ( 'NONE', #22255, 0.7441270634457337607 ) ;
#13803 = CARTESIAN_POINT ( 'NONE',  ( 39.99999999999998579, 80.00000000000001421, 52.49999999999999289 ) ) ;
#13804 = DIRECTION ( 'NONE',  ( -0.000000000000000000, 1.132880637372608986E-16, -1.000000000000000000 ) ) ;
#13805 = ORIENTED_EDGE ( 'NONE', *, *, #23301, .F. ) ;
#13806 = EDGE_CURVE ( 'NONE', #23362, #28205, #19425, .T. ) ;
#13807 = CARTESIAN_POINT ( 'NONE',  ( 11.68275852895869349, 12.45554129448069602, 19.08844262864050023 ) ) ;
#13808 = DIRECTION ( 'NONE',  ( 0.2972711322815266843, -0.9547931052914339078, 0.000000000000000000 ) ) ;
#13809 = LINE ( 'NONE', #30626, #3796 ) ;
#13810 = DIRECTION ( 'NONE',  ( 0.000000000000000000, 0.000000000000000000, -1.000000000000000000 ) ) ;
#13811 = CARTESIAN_POINT ( 'NONE',  ( -47.38851077911648702, 69.82999317555587027, 15.75289764418246286 ) ) ;
#13812 = CIRCLE ( 'NONE', #22282, 0.7500000000000006661 ) ;
#13813 = CARTESIAN_POINT ( 'NONE',  ( -15.27573937290524242, -7.547610621728492397, 18.37259980046034258 ) ) ;
#13814 = CARTESIAN_POINT ( 'NONE',  ( 0.000000000000000000, 0.000000000000000000, 1.500000000000001332 ) ) ;
#13815 = CARTESIAN_POINT ( 'NONE',  ( 4.668110441710642711, -19.44758969394385062, 24.50000000000000000 ) ) ;
#13816 = DIRECTION ( 'NONE',  ( 0.000000000000000000, 0.000000000000000000, -1.000000000000000000 ) ) ;
#13817 = DIRECTION ( 'NONE',  ( 0.000000000000000000, -1.132880637372608986E-16, 1.000000000000000000 ) ) ;
#13818 = CARTESIAN_POINT ( 'NONE',  ( -15.26311659977723956, -7.574663188999289254, 20.32842677360128292 ) ) ;
#13819 = DIRECTION ( 'NONE',  ( 0.000000000000000000, 0.000000000000000000, 1.000000000000000000 ) ) ;
#13820 = AXIS2_PLACEMENT_3D ( 'NONE', #23100, #4692, #30286 ) ;
#13821 = ORIENTED_EDGE ( 'NONE', *, *, #30763, .F. ) ;
#13822 = ORIENTED_EDGE ( 'NONE', *, *, #23824, .F. ) ;
#13823 = AXIS2_PLACEMENT_3D ( 'NONE', #27996, #15833, #30180 ) ;
#13824 = DIRECTION ( 'NONE',  ( -1.000000000000000000, 0.000000000000000000, 0.000000000000000000 ) ) ;
#13825 = CARTESIAN_POINT ( 'NONE',  ( 12.56641067637329812, 40.32935944495179115, -1.500000000000000000 ) ) ;
#13826 = DIRECTION ( 'NONE',  ( -0.000000000000000000, -1.000000000000000000, -0.000000000000000000 ) ) ;
#13827 = VERTEX_POINT ( 'NONE', #14732 ) ;
#13828 = DIRECTION ( 'NONE',  ( 1.000000000000000000, 0.000000000000000000, 0.000000000000000000 ) ) ;
#13829 = CARTESIAN_POINT ( 'NONE',  ( 18.05613910678266976, -8.642405844459423392, 18.63641924841378028 ) ) ;
#13830 = CARTESIAN_POINT ( 'NONE',  ( 4.119120293826441959, 16.53802619141620411, 5.653912893140659257 ) ) ;
#13831 = AXIS2_PLACEMENT_3D ( 'NONE', #8664, #15515, #27218 ) ;
#13832 = ADVANCED_FACE ( 'NONE', ( #21913 ), #8045, .F. ) ;
#13833 = ORIENTED_EDGE ( 'NONE', *, *, #16472, .F. ) ;
#13834 = CARTESIAN_POINT ( 'NONE',  ( -16.81500952837178886, 2.642855143025227616, 6.530762810602277924 ) ) ;
#13835 = AXIS2_PLACEMENT_3D ( 'NONE', #28386, #2636, #23988 ) ;
#13836 = DIRECTION ( 'NONE',  ( -0.000000000000000000, -0.000000000000000000, -1.000000000000000000 ) ) ;
#13837 = EDGE_CURVE ( 'NONE', #3697, #4518, #24639, .T. ) ;
#13838 = VECTOR ( 'NONE', #5255, 1000.000000000000000 ) ;
#13839 = CARTESIAN_POINT ( 'NONE',  ( -14.49834914336386404, -41.18788872621845343, -16.50000000000000355 ) ) ;
#13840 = CARTESIAN_POINT ( 'NONE',  ( 1.874238930957292881, 37.52724763749905179, 37.50000000023297986 ) ) ;
#13841 = ORIENTED_EDGE ( 'NONE', *, *, #29838, .F. ) ;
#13842 = DIRECTION ( 'NONE',  ( 0.000000000000000000, 0.000000000000000000, 1.000000000000000000 ) ) ;
#13843 = DIRECTION ( 'NONE',  ( 1.000000000000000000, 0.000000000000000000, 0.000000000000000000 ) ) ;
#13844 = CARTESIAN_POINT ( 'NONE',  ( -1.073881485057887497, 0.9711784013062738641, -1.500000000000000000 ) ) ;
#13845 = AXIS2_PLACEMENT_3D ( 'NONE', #6358, #30061, #18522 ) ;
#13846 = EDGE_LOOP ( 'NONE', ( #1433, #3605, #6407, #9831 ) ) ;
#13847 = AXIS2_PLACEMENT_3D ( 'NONE', #20690, #20989, #30513 ) ;
#13848 = CARTESIAN_POINT ( 'NONE',  ( -39.87350638641186862, -4.706224724276806270, -11.49999999999999645 ) ) ;
#13849 = DIRECTION ( 'NONE',  ( -0.9096319953545183301, -0.4154150130018863796, 0.000000000000000000 ) ) ;
#13850 = DIRECTION ( 'NONE',  ( -1.000000000000000000, 0.000000000000000000, 0.000000000000000000 ) ) ;
#13851 = DIRECTION ( 'NONE',  ( 1.000000000000000000, 0.000000000000000000, 0.000000000000000000 ) ) ;
#13852 = CARTESIAN_POINT ( 'NONE',  ( 24.44496207165490276, 7.595930209050162141, 49.40206402021032517 ) ) ;
#13853 = DIRECTION ( 'NONE',  ( -0.2972711322815276280, -0.9547931052914334638, 0.000000000000000000 ) ) ;
#13854 = CARTESIAN_POINT ( 'NONE',  ( -19.92072812706008023, 1.967956072006115331, 20.19593175699879595 ) ) ;
#13855 = DIRECTION ( 'NONE',  ( 0.000000000000000000, 0.000000000000000000, 1.000000000000000000 ) ) ;
#13856 = EDGE_LOOP ( 'NONE', ( #22548, #5122, #20528, #7220 ) ) ;
#13857 = AXIS2_PLACEMENT_3D ( 'NONE', #28668, #7148, #6678 ) ;
#13858 = CARTESIAN_POINT ( 'NONE',  ( 11.81973518349029462, -16.15564139912475738, 19.89182036555910571 ) ) ;
#13859 = CARTESIAN_POINT ( 'NONE',  ( 32.31576317091162309, 17.59561277345964214, 34.80090346875808649 ) ) ;
#13860 = AXIS2_PLACEMENT_3D ( 'NONE', #27277, #5910, #20700 ) ;
#13861 = ORIENTED_EDGE ( 'NONE', *, *, #18130, .F. ) ;
#13862 = ORIENTED_EDGE ( 'NONE', *, *, #17730, .F. ) ;
#13863 = CARTESIAN_POINT ( 'NONE',  ( 5.041560023644207966, 19.35451993181657926, 20.32200205377525393 ) ) ;
#13864 = ORIENTED_EDGE ( 'NONE', *, *, #9017, .F. ) ;
#13865 = AXIS2_PLACEMENT_3D ( 'NONE', #27540, #1943, #18335 ) ;
#13866 = DIRECTION ( 'NONE',  ( -0.000000000000000000, -0.000000000000000000, 1.000000000000000000 ) ) ;
#13867 = CARTESIAN_POINT ( 'NONE',  ( 23.07491035053308437, 11.55692089822198376, 49.19304184087432219 ) ) ;
#13868 = ORIENTED_EDGE ( 'NONE', *, *, #26976, .T. ) ;
#13869 = CARTESIAN_POINT ( 'NONE',  ( -15.85201432996395710, 12.19518096057847600, 18.73377938172350810 ) ) ;
#13870 = CARTESIAN_POINT ( 'NONE',  ( 26.73000961532937225, -9.331429872129930914, -1.500000000000000000 ) ) ;
#13871 = ORIENTED_EDGE ( 'NONE', *, *, #24998, .F. ) ;
#13872 = DIRECTION ( 'NONE',  ( 0.000000000000000000, 0.000000000000000000, 1.000000000000000000 ) ) ;
#13873 = ORIENTED_EDGE ( 'NONE', *, *, #27310, .F. ) ;
#13874 = CARTESIAN_POINT ( 'NONE',  ( 32.19782014694308003, -14.25394737442115201, -16.55003854064094426 ) ) ;
#13875 = AXIS2_PLACEMENT_3D ( 'NONE', #29226, #12858, #26897 ) ;
#13876 = VERTEX_POINT ( 'NONE', #17696 ) ;
#13877 = AXIS2_PLACEMENT_3D ( 'NONE', #4328, #1844, #1995 ) ;
#13878 = EDGE_LOOP ( 'NONE', ( #27455, #24200, #26484, #22069 ) ) ;
#13879 = LINE ( 'NONE', #30555, #2126 ) ;
#13880 = CARTESIAN_POINT ( 'NONE',  ( 0.7836604620899298990, -17.02735026737547841, 18.34798005863078885 ) ) ;
#13881 = DIRECTION ( 'NONE',  ( -0.000000000000000000, -0.000000000000000000, 1.000000000000000000 ) ) ;
#13882 = CARTESIAN_POINT ( 'NONE',  ( -34.13832859401785669, -12.80067323710187921, 34.80090346875803675 ) ) ;
#13883 = CARTESIAN_POINT ( 'NONE',  ( 20.55390841643019684, -27.45161667029107022, -16.50001200000000168 ) ) ;
#13884 = FACE_OUTER_BOUND ( 'NONE', #24959, .T. ) ;
#13885 = ORIENTED_EDGE ( 'NONE', *, *, #8275, .F. ) ;
#13886 = CARTESIAN_POINT ( 'NONE',  ( 10.83311381505435023, -16.83321666392360783, 7.595116371587256054 ) ) ;
#13887 = CARTESIAN_POINT ( 'NONE',  ( 15.76815964721467367, -6.465453726329344342, 5.657991946698900598 ) ) ;
#13888 = CARTESIAN_POINT ( 'NONE',  ( -13.43037651602832128, 10.49991632925268625, 5.652605728828375753 ) ) ;
#13889 = CARTESIAN_POINT ( 'NONE',  ( 5.080682615984644990, 19.36225455879193902, 18.37415474056476938 ) ) ;
#13890 = ORIENTED_EDGE ( 'NONE', *, *, #17549, .F. ) ;
#13891 = VERTEX_POINT ( 'NONE', #22836 ) ;
#13892 = PRODUCT_DEFINITION_FORMATION_WITH_SPECIFIED_SOURCE ( 'ANY', '', #7963, .NOT_KNOWN. ) ;
#13893 = DIRECTION ( 'NONE',  ( 0.000000000000000000, 1.000000000000000000, 0.000000000000000000 ) ) ;
#13894 = CARTESIAN_POINT ( 'NONE',  ( -5.557658336892892237, 19.23087281213773281, 18.44501272782439827 ) ) ;
#13895 = CARTESIAN_POINT ( 'NONE',  ( 126.5359999999999872, 7.347880794884121708E-16, -6.000000000000001776 ) ) ;
#13896 = CIRCLE ( 'NONE', #14896, 36.25735931288072322 ) ;
#13897 = AXIS2_PLACEMENT_3D ( 'NONE', #13379, #1519, #1212 ) ;
#13898 = CARTESIAN_POINT ( 'NONE',  ( 24.35970437652574816, -13.37404834226503958, 42.96778633356033339 ) ) ;
#13899 = CYLINDRICAL_SURFACE ( 'NONE', #5940, 20.00000000000000355 ) ;
#13900 = VERTEX_POINT ( 'NONE', #8519 ) ;
#13901 = CARTESIAN_POINT ( 'NONE',  ( 0.8583496426666205048, -19.98194197654538584, 7.528076282304595246 ) ) ;
#13902 = CIRCLE ( 'NONE', #8451, 9.482273699623480212 ) ;
#13903 = CARTESIAN_POINT ( 'NONE',  ( -40.00000000000002842, 80.00000000000001421, 52.50000000000014921 ) ) ;
#13904 = CARTESIAN_POINT ( 'NONE',  ( 19.76423196911361302, 3.064691114365034608, 20.34789198813115263 ) ) ;
#13905 = ORIENTED_EDGE ( 'NONE', *, *, #16398, .F. ) ;
#13906 = CARTESIAN_POINT ( 'NONE',  ( 37.99999999999999289, 80.00000000000001421, 17.91742430504415040 ) ) ;
#13907 = ORIENTED_EDGE ( 'NONE', *, *, #20420, .T. ) ;
#13908 = CARTESIAN_POINT ( 'NONE',  ( 0.000000000000000000, 0.000000000000000000, 0.000000000000000000 ) ) ;
#13909 = EDGE_CURVE ( 'NONE', #22584, #26952, #13338, .T. ) ;
#13910 = CIRCLE ( 'NONE', #16894, 2.898871837527149609 ) ;
#13911 = CARTESIAN_POINT ( 'NONE',  ( -23.07229726322976404, 36.25693017875646262, -16.50000000000000000 ) ) ;
#13912 = ORIENTED_EDGE ( 'NONE', *, *, #23824, .T. ) ;
#13913 = CARTESIAN_POINT ( 'NONE',  ( 35.72891310271008081, 4.992827801344182248, 27.50000000000001066 ) ) ;
#13914 = CARTESIAN_POINT ( 'NONE',  ( -4.776122516674677878E-15, -42.50000000000000000, 1.500000000000001332 ) ) ;
#13915 = CARTESIAN_POINT ( 'NONE',  ( -4.100931858250860707, -19.90478481566557534, 1.500000000000000000 ) ) ;
#13916 = ADVANCED_FACE ( 'NONE', ( #1486 ), #18168, .F. ) ;
#13917 = CARTESIAN_POINT ( 'NONE',  ( 0.000000000000000000, -2.435693370351110282E-15, 21.50000000000000355 ) ) ;
#13918 = CONICAL_SURFACE ( 'NONE', #7943, 37.50000000000001421, 0.7853981633974500554 ) ;
#13919 = LINE ( 'NONE', #24026, #30255 ) ;
#13920 = CARTESIAN_POINT ( 'NONE',  ( -19.84403786039536755, 2.492757843112275662, 5.652196082369963293 ) ) ;
#13921 = EDGE_LOOP ( 'NONE', ( #4225, #5004, #18110, #30116 ) ) ;
#13922 = CARTESIAN_POINT ( 'NONE',  ( 15.38884489568259362, -7.274072546997685684, 6.782064869129509788 ) ) ;
#13923 = COLOUR_RGB ( '',0.7921568627450980005, 0.8196078431372548767, 0.9333333333333333481 ) ;
#13924 = CARTESIAN_POINT ( 'NONE',  ( 25.19442432474404470, 35.44676296256560022, -19.50000000000000355 ) ) ;
#13925 = DIRECTION ( 'NONE',  ( -0.000000000000000000, -0.000000000000000000, -1.000000000000000000 ) ) ;
#13926 = ORIENTED_EDGE ( 'NONE', *, *, #16050, .T. ) ;
#13927 = CARTESIAN_POINT ( 'NONE',  ( -23.21352257770656990, -10.78826658734919519, 49.40206402021038201 ) ) ;
#13928 = CIRCLE ( 'NONE', #15413, 21.71568325578263625 ) ;
#13929 = ADVANCED_FACE ( 'NONE', ( #3815 ), #1018, .F. ) ;
#13930 = CARTESIAN_POINT ( 'NONE',  ( 3.221450758838616757, 1.621276839356792454, -1.500000000000000000 ) ) ;
#13931 = ORIENTED_EDGE ( 'NONE', *, *, #20391, .T. ) ;
#13932 = DIRECTION ( 'NONE',  ( 0.000000000000000000, 0.000000000000000000, 1.000000000000000000 ) ) ;
#13933 = LINE ( 'NONE', #8960, #5178 ) ;
#13934 = EDGE_CURVE ( 'NONE', #11358, #15951, #17741, .T. ) ;
#13935 = CARTESIAN_POINT ( 'NONE',  ( 32.23417439153795527, -24.08006005343069944, 30.66707834874007332 ) ) ;
#13936 = EDGE_CURVE ( 'NONE', #29313, #12760, #29459, .T. ) ;
#13937 = FACE_OUTER_BOUND ( 'NONE', #9255, .T. ) ;
#13938 = VERTEX_POINT ( 'NONE', #30164 ) ;
#13939 = CARTESIAN_POINT ( 'NONE',  ( 23.21352257770656635, -10.78826658734920052, 49.40206402021031806 ) ) ;
#13940 = DIRECTION ( 'NONE',  ( -0.9329908884337534403, -0.3598999890241668664, 0.000000000000000000 ) ) ;
#13941 = CARTESIAN_POINT ( 'NONE',  ( -20.00000000000004263, 1.387778780781445676E-14, 24.50000000000000000 ) ) ;
#13942 = EDGE_CURVE ( 'NONE', #18940, #24218, #26130, .T. ) ;
#13943 = EDGE_LOOP ( 'NONE', ( #3751, #24642, #734, #19336, #16730, #23708 ) ) ;
#13944 = ADVANCED_FACE ( 'NONE', ( #27213 ), #17866, .F. ) ;
#13945 = CARTESIAN_POINT ( 'NONE',  ( -32.93066664481271033, 23.11087910253402455, -3.166603179814979185 ) ) ;
#13946 = ORIENTED_EDGE ( 'NONE', *, *, #15096, .F. ) ;
#13947 = CARTESIAN_POINT ( 'NONE',  ( -30.86161751192252467, -15.46691422980912733, 40.47962024281694937 ) ) ;
#13948 = EDGE_CURVE ( 'NONE', #19294, #1929, #3351, .T. ) ;
#13949 = LINE ( 'NONE', #30782, #26459 ) ;
#13950 = TOROIDAL_SURFACE ( 'NONE', #5476, 53.00000000000000711, 3.000000000000000000 ) ;
#13951 = PLANE ( 'NONE',  #6862 ) ;
#13952 = EDGE_CURVE ( 'NONE', #24522, #16767, #20086, .T. ) ;
#13953 = CARTESIAN_POINT ( 'NONE',  ( 1.316598178790388207, -17.01073877869967532, 20.19593175699879595 ) ) ;
#13954 = ORIENTED_EDGE ( 'NONE', *, *, #23339, .F. ) ;
#13955 = EDGE_CURVE ( 'NONE', #26398, #1188, #6148, .T. ) ;
#13956 = DIRECTION ( 'NONE',  ( -0.000000000000000000, 0.000000000000000000, 1.000000000000000000 ) ) ;
#13957 = CARTESIAN_POINT ( 'NONE',  ( 8.419710366748642372, 7.777014463793876509, 1.500000000000000000 ) ) ;
#13958 = CARTESIAN_POINT ( 'NONE',  ( 15.57266529552201995, -38.96488032230103471, 1.500000000000000000 ) ) ;
#13959 = ORIENTED_EDGE ( 'NONE', *, *, #3618, .T. ) ;
#13960 = CARTESIAN_POINT ( 'NONE',  ( 0.000000000000000000, 0.000000000000000000, 21.50000000000000000 ) ) ;
#13961 = CARTESIAN_POINT ( 'NONE',  ( -15.57728904105048606, -6.860944617588176087, 19.21496526180053621 ) ) ;
#13962 = FACE_OUTER_BOUND ( 'NONE', #29801, .T. ) ;
#13963 = DIRECTION ( 'NONE',  ( 1.000000000000000000, 0.000000000000000000, 0.000000000000000000 ) ) ;
#13964 = CARTESIAN_POINT ( 'NONE',  ( 4.473510263713153634, 42.23049256842776344, 19.94491637797075612 ) ) ;
#13965 = CARTESIAN_POINT ( 'NONE',  ( -24.02386986937633395, 13.21681873352653902, 43.33784216537009826 ) ) ;
#13966 = CARTESIAN_POINT ( 'NONE',  ( -15.57976790534002909, -6.855017190910953850, 19.33715507985239412 ) ) ;
#13967 = CIRCLE ( 'NONE', #28932, 0.7500000000000006661 ) ;
#13968 = CARTESIAN_POINT ( 'NONE',  ( 33.56327786402394509, -10.57885966092500851, 35.56709683732771055 ) ) ;
#13969 = EDGE_LOOP ( 'NONE', ( #10889, #4919 ) ) ;
#13970 = VERTEX_POINT ( 'NONE', #14077 ) ;
#13971 = CARTESIAN_POINT ( 'NONE',  ( 32.98805937973593672, -80.00000000000000000, 13.00000000000000178 ) ) ;
#13972 = CARTESIAN_POINT ( 'NONE',  ( 37.98493438987956949, 11.12428508576150143, -1.500000000000000000 ) ) ;
#13973 = EDGE_CURVE ( 'NONE', #23230, #4543, #1942, .T. ) ;
#13974 = LINE ( 'NONE', #18656, #25844 ) ;
#13975 = EDGE_CURVE ( 'NONE', #21378, #10498, #10126, .T. ) ;
#13976 = VERTEX_POINT ( 'NONE', #9107 ) ;
#13977 = CARTESIAN_POINT ( 'NONE',  ( -50.00000000000000000, -50.00000000000000000, 70.00000000000000000 ) ) ;
#13978 = CARTESIAN_POINT ( 'NONE',  ( 15.43168774359948436, -7.187270164670358064, 18.90679857307105749 ) ) ;
#13979 = EDGE_CURVE ( 'NONE', #2547, #28904, #26571, .T. ) ;
#13980 = CARTESIAN_POINT ( 'NONE',  ( 6.184030279945250008, 19.03884152227148263, 7.080843742048788414 ) ) ;
#13981 = EDGE_LOOP ( 'NONE', ( #22654, #21133, #10088, #16825 ) ) ;
#13982 = CARTESIAN_POINT ( 'NONE',  ( 0.1262659238204208167, 8.999114229549594057, 21.50000000000000000 ) ) ;
#13983 = EDGE_CURVE ( 'NONE', #5019, #7694, #26091, .T. ) ;
#13984 = CARTESIAN_POINT ( 'NONE',  ( 12.13430697852917994, 11.98518526348621371, 7.603368798681074736 ) ) ;
#13985 = CARTESIAN_POINT ( 'NONE',  ( 0.000000000000000000, 0.000000000000000000, 1.500000000000001332 ) ) ;
#13986 = CARTESIAN_POINT ( 'NONE',  ( -24.78335882923826006, 28.14977597724353231, 37.50000000000454037 ) ) ;
#13987 = ORIENTED_EDGE ( 'NONE', *, *, #3106, .F. ) ;
#13988 = FACE_OUTER_BOUND ( 'NONE', #24958, .T. ) ;
#13989 = EDGE_CURVE ( 'NONE', #21542, #11840, #1163, .T. ) ;
#13990 = CARTESIAN_POINT ( 'NONE',  ( -15.04923167492114366, -8.024232118407711667, 5.653604225791662330 ) ) ;
#13991 = AXIS2_PLACEMENT_3D ( 'NONE', #27611, #28204, #6836 ) ;
#13992 = CARTESIAN_POINT ( 'NONE',  ( -15.01515151829604910, 13.21212483861245168, 5.775318986477952166 ) ) ;
#13993 = ORIENTED_EDGE ( 'NONE', *, *, #13204, .F. ) ;
#13994 = CARTESIAN_POINT ( 'NONE',  ( 16.83255095305771931, 2.584307790367077029, 18.54473042795394022 ) ) ;
#13995 = CARTESIAN_POINT ( 'NONE',  ( 7.295277785476350196, -43.36226450306268987, -16.50000000000000000 ) ) ;
#13996 = CARTESIAN_POINT ( 'NONE',  ( 30.33183837007556249, -13.53414739637283226, -16.55003854064094426 ) ) ;
#13997 = CARTESIAN_POINT ( 'NONE',  ( -5.687793815610304726, 6.974883619896852238, 1.500000000000001332 ) ) ;
#13998 = CARTESIAN_POINT ( 'NONE',  ( 39.99999999999998579, 90.00000000000001421, 22.49999999999999289 ) ) ;
#13999 = CYLINDRICAL_SURFACE ( 'NONE', #25944, 0.7499999999999988898 ) ;
#14000 = DIRECTION ( 'NONE',  ( 0.000000000000000000, 1.000000000000000000, 0.000000000000000000 ) ) ;
#14001 = VERTEX_POINT ( 'NONE', #16276 ) ;
#14002 = ADVANCED_FACE ( 'NONE', ( #4574 ), #4423, .F. ) ;
#14003 = EDGE_CURVE ( 'NONE', #12360, #7713, #9560, .T. ) ;
#14004 = CARTESIAN_POINT ( 'NONE',  ( 10.69227409735889722, -13.31703061742498306, 19.36813350477385143 ) ) ;
#14005 = PLANE ( 'NONE',  #5618 ) ;
#14006 = ORIENTED_EDGE ( 'NONE', *, *, #23471, .T. ) ;
#14007 = ORIENTED_EDGE ( 'NONE', *, *, #201, .T. ) ;
#14008 = DIRECTION ( 'NONE',  ( -0.000000000000000000, 1.132880637372608986E-16, -1.000000000000000000 ) ) ;
#14009 = ORIENTED_EDGE ( 'NONE', *, *, #9015, .T. ) ;
#14010 = VECTOR ( 'NONE', #17456, 1000.000000000000114 ) ;
#14011 = DIRECTION ( 'NONE',  ( 1.000000000000000000, 0.000000000000000000, 0.000000000000000000 ) ) ;
#14012 = DIRECTION ( 'NONE',  ( 1.000000000000000000, 0.000000000000000000, 0.000000000000000000 ) ) ;
#14013 = VERTEX_POINT ( 'NONE', #28135 ) ;
#14014 = DIRECTION ( 'NONE',  ( 0.000000000000000000, 0.000000000000000000, 1.000000000000000000 ) ) ;
#14015 = CARTESIAN_POINT ( 'NONE',  ( 0.000000000000000000, 0.000000000000000000, 21.50000000000000000 ) ) ;
#14016 = VERTEX_POINT ( 'NONE', #13790 ) ;
#14017 = ORIENTED_EDGE ( 'NONE', *, *, #22387, .T. ) ;
#14018 = CARTESIAN_POINT ( 'NONE',  ( -31.29501345865439532, 26.27841684421964885, -6.500000000000000888 ) ) ;
#14019 = VECTOR ( 'NONE', #5129, 1000.000000000000000 ) ;
#14020 = ORIENTED_EDGE ( 'NONE', *, *, #27092, .F. ) ;
#14021 = VERTEX_POINT ( 'NONE', #13939 ) ;
#14022 = DIRECTION ( 'NONE',  ( -1.000000000000000000, 0.000000000000000000, 0.000000000000000000 ) ) ;
#14023 = DIRECTION ( 'NONE',  ( 1.000000000000000000, 0.000000000000000000, 0.000000000000000000 ) ) ;
#14024 = AXIS2_PLACEMENT_3D ( 'NONE', #18349, #25822, #28152 ) ;
#14025 = CARTESIAN_POINT ( 'NONE',  ( -14.79998981349582721, -8.507912210612349924, 18.73314399819311404 ) ) ;
#14026 = DIRECTION ( 'NONE',  ( 1.000000000000000000, 0.000000000000000000, 0.000000000000000000 ) ) ;
#14027 = FACE_BOUND ( 'NONE', #13943, .T. ) ;
#14028 = EDGE_LOOP ( 'NONE', ( #4938, #15585, #6303, #22663 ) ) ;
#14029 = LINE ( 'NONE', #14335, #23199 ) ;
#14030 = DIRECTION ( 'NONE',  ( 0.000000000000000000, -0.000000000000000000, 1.000000000000000000 ) ) ;
#14031 = CARTESIAN_POINT ( 'NONE',  ( -13.51981801095249658, 10.39108251695558138, 7.627891251804737927 ) ) ;
#14032 = LINE ( 'NONE', #9664, #26778 ) ;
#14033 = ORIENTED_EDGE ( 'NONE', *, *, #26906, .F. ) ;
#14034 = ORIENTED_EDGE ( 'NONE', *, *, #8218, .T. ) ;
#14035 = EDGE_CURVE ( 'NONE', #18512, #23209, #27839, .T. ) ;
#14036 = DIRECTION ( 'NONE',  ( 1.000000000000000000, 0.000000000000000000, 0.000000000000000000 ) ) ;
#14037 = FACE_OUTER_BOUND ( 'NONE', #5546, .T. ) ;
#14038 = DIRECTION ( 'NONE',  ( 0.06975647374412530244, -0.000000000000000000, 0.9975640502598241977 ) ) ;
#14039 = CARTESIAN_POINT ( 'NONE',  ( -4.163336342344337027E-14, 1.387778780781445676E-14, 67.49999999999997158 ) ) ;
#14040 = DIRECTION ( 'NONE',  ( 0.000000000000000000, 0.000000000000000000, 1.000000000000000000 ) ) ;
#14041 = ORIENTED_EDGE ( 'NONE', *, *, #30549, .F. ) ;
#14042 = CARTESIAN_POINT ( 'NONE',  ( -17.05413688332568967, 0.7966627085705102473, 7.196036389296800451 ) ) ;
#14043 = CARTESIAN_POINT ( 'NONE',  ( 6.187077094091595342, 11.47693674426096599, 1.500000000000001332 ) ) ;
#14044 = DIRECTION ( 'NONE',  ( -0.6707505147970023174, -0.7416830501633134842, 0.000000000000000000 ) ) ;
#14045 = ORIENTED_EDGE ( 'NONE', *, *, #29014, .T. ) ;
#14046 = DIRECTION ( 'NONE',  ( -0.000000000000000000, -0.000000000000000000, 1.000000000000000000 ) ) ;
#14047 = ORIENTED_EDGE ( 'NONE', *, *, #17830, .T. ) ;
#14048 = CARTESIAN_POINT ( 'NONE',  ( 15.98815986143407208, -5.948957736846856470, 5.749491821935610147 ) ) ;
#14049 = DIRECTION ( 'NONE',  ( 1.000000000000000000, 0.000000000000000000, 0.000000000000000000 ) ) ;
#14050 = ORIENTED_EDGE ( 'NONE', *, *, #30356, .T. ) ;
#14051 = CARTESIAN_POINT ( 'NONE',  ( 30.05895891365310391, -21.74113609263913105, 27.50000000000000000 ) ) ;
#14052 = CARTESIAN_POINT ( 'NONE',  ( -40.05104235265675783, 2.353288714454549790, -11.49999999999999645 ) ) ;
#14053 = VECTOR ( 'NONE', #17263, 1000.000000000000000 ) ;
#14054 = CARTESIAN_POINT ( 'NONE',  ( -13.93942108199721730, 16.65122935894503442, 1.500000000000000000 ) ) ;
#14055 = FACE_OUTER_BOUND ( 'NONE', #29757, .T. ) ;
#14056 = CYLINDRICAL_SURFACE ( 'NONE', #884, 10.00000000000000000 ) ;
#14057 = DIRECTION ( 'NONE',  ( 1.000000000000000000, 0.000000000000000000, -0.000000000000000000 ) ) ;
#14058 = CARTESIAN_POINT ( 'NONE',  ( -30.50257113119997499, 15.54031451041691092, 40.76699977199277214 ) ) ;
#14059 = ORIENTED_EDGE ( 'NONE', *, *, #11135, .F. ) ;
#14060 = CARTESIAN_POINT ( 'NONE',  ( 32.74775157611827581, 27.21557300921217859, -19.50000000000000355 ) ) ;
#14061 = CARTESIAN_POINT ( 'NONE',  ( 37.99999999999999289, 80.00000000000001421, 50.49999999999998579 ) ) ;
#14062 = ORIENTED_EDGE ( 'NONE', *, *, #3078, .T. ) ;
#14063 = DIRECTION ( 'NONE',  ( 1.000000000000000000, 0.000000000000000000, 0.000000000000000000 ) ) ;
#14064 = CARTESIAN_POINT ( 'NONE',  ( -14.75084321123810938, -8.599826344683139112, 19.79423548914561692 ) ) ;
#14065 = CARTESIAN_POINT ( 'NONE',  ( -33.53985793123796100, 24.80925987296827984, -16.50000000000000000 ) ) ;
#14066 =( LENGTH_UNIT ( ) NAMED_UNIT ( * ) SI_UNIT ( .MILLI., .METRE. ) );
#14067 = CARTESIAN_POINT ( 'NONE',  ( 10.64374042650142904, 42.96126232887663576, -19.50000000000000355 ) ) ;
#14068 = ORIENTED_EDGE ( 'NONE', *, *, #5034, .F. ) ;
#14069 = CARTESIAN_POINT ( 'NONE',  ( -12.86767874445213877, -1.850092897552710225, 1.500000000000001332 ) ) ;
#14070 = CIRCLE ( 'NONE', #15576, 1.447898107987198646 ) ;
#14071 = CIRCLE ( 'NONE', #28097, 9.482273699623480212 ) ;
#14072 = CARTESIAN_POINT ( 'NONE',  ( -34.07766914599911701, 21.40380666528009002, -1.500000000000000000 ) ) ;
#14073 = CARTESIAN_POINT ( 'NONE',  ( 14.12697113674015448, -34.75723440155685751, 37.49999999999971578 ) ) ;
#14075 = AXIS2_PLACEMENT_3D ( 'NONE', #3341, #24699, #10367 ) ;
#14074 = CARTESIAN_POINT ( 'NONE',  ( -4.622016212553093695, -12.19167610014704906, 24.50000000000000000 ) ) ;
#14076 = ORIENTED_EDGE ( 'NONE', *, *, #3520, .F. ) ;
#14077 = CARTESIAN_POINT ( 'NONE',  ( 20.47140833542507821, -26.57182937991349903, -6.500000000000000888 ) ) ;
#14078 = CARTESIAN_POINT ( 'NONE',  ( 19.64114023396309960, -37.13592150529014191, -1.500000000000000000 ) ) ;
#14079 = LINE ( 'NONE', #11299, #29381 ) ;
#14080 = ORIENTED_EDGE ( 'NONE', *, *, #26331, .T. ) ;
#14081 = ORIENTED_EDGE ( 'NONE', *, *, #11708, .T. ) ;
#14082 = CARTESIAN_POINT ( 'NONE',  ( -32.06725342158289038, -14.54034564589948708, 35.54788606881766810 ) ) ;
#14083 = EDGE_LOOP ( 'NONE', ( #28365, #9570, #5473, #26910 ) ) ;
#14084 = CARTESIAN_POINT ( 'NONE',  ( 0.1277494853664046803, -20.01772078232906438, 18.36582235739946611 ) ) ;
#14085 = CARTESIAN_POINT ( 'NONE',  ( -8.550548368345317840, -14.74545326172987103, 7.652108011868850035 ) ) ;
#14086 = DIRECTION ( 'NONE',  ( -0.000000000000000000, -0.000000000000000000, 1.000000000000000000 ) ) ;
#14087 = CARTESIAN_POINT ( 'NONE',  ( 0.9279538312821433710, -17.02439129904410464, 20.33971507717571114 ) ) ;
#14088 = VERTEX_POINT ( 'NONE', #23437 ) ;
#14089 = CARTESIAN_POINT ( 'NONE',  ( -37.99999999999999289, 90.00000000000001421, -34.49999999999999289 ) ) ;
#14090 = AXIS2_PLACEMENT_3D ( 'NONE', #20166, #26898, #5518 ) ;
#14091 = CARTESIAN_POINT ( 'NONE',  ( 2.703030265324084080, -12.75514121382991384, 1.500000000000001332 ) ) ;
#14092 = CARTESIAN_POINT ( 'NONE',  ( 11.70346162051516359, 12.43461153239107730, 19.69140814234746273 ) ) ;
#14093 = CARTESIAN_POINT ( 'NONE',  ( 27.03074382657074537, 6.449748410230989215, 42.96778633356034760 ) ) ;
#14094 = ORIENTED_EDGE ( 'NONE', *, *, #13936, .T. ) ;
#14095 = AXIS2_PLACEMENT_3D ( 'NONE', #6104, #8753, #27175 ) ;
#14096 = CARTESIAN_POINT ( 'NONE',  ( -15.57738559309032489, -6.860713375568480821, 19.41069149716888020 ) ) ;
#14097 = DIRECTION ( 'NONE',  ( 0.9096319953545183301, 0.4154150130018865461, 0.000000000000000000 ) ) ;
#14098 = CARTESIAN_POINT ( 'NONE',  ( -2.431858781452794549, -8.752572334588112568, -1.500000000000002887 ) ) ;
#14099 = CARTESIAN_POINT ( 'NONE',  ( 4.049916833591939103, 16.55712665779026693, 20.34789198813115263 ) ) ;
#14100 = FACE_OUTER_BOUND ( 'NONE', #24451, .T. ) ;
#14101 = AXIS2_PLACEMENT_3D ( 'NONE', #16128, #23287, #1931 ) ;
#14102 = ADVANCED_FACE ( 'NONE', ( #30318, #8964 ), #18480, .T. ) ;
#14103 = CARTESIAN_POINT ( 'NONE',  ( 5.060094141397912360, 42.14075867279367316, 28.87075318537527835 ) ) ;
#14104 = CARTESIAN_POINT ( 'NONE',  ( 31.31394823341868161, -25.51108937476379879, -1.500000000000000000 ) ) ;
#14105 = ORIENTED_EDGE ( 'NONE', *, *, #26558, .F. ) ;
#14106 = ORIENTED_EDGE ( 'NONE', *, *, #18529, .F. ) ;
#14107 = DIRECTION ( 'NONE',  ( 0.000000000000000000, 0.000000000000000000, -1.000000000000000000 ) ) ;
#14108 = CARTESIAN_POINT ( 'NONE',  ( 0.000000000000000000, 44.39187623478217404, -19.50000000000000355 ) ) ;
#14109 = LINE ( 'NONE', #23617, #18869 ) ;
#14110 = CARTESIAN_POINT ( 'NONE',  ( 1.687027447297431371, 8.840471615930075799, 21.50000000000000000 ) ) ;
#14111 = ORIENTED_EDGE ( 'NONE', *, *, #22309, .T. ) ;
#14112 = CARTESIAN_POINT ( 'NONE',  ( 0.000000000000000000, 0.000000000000000000, 0.000000000000000000 ) ) ;
#14113 = AXIS2_PLACEMENT_3D ( 'NONE', #9439, #9729, #21262 ) ;
#14114 = CARTESIAN_POINT ( 'NONE',  ( 15.38325456941028868, -7.285321374151285667, 19.33715507985239412 ) ) ;
#14115 = EDGE_CURVE ( 'NONE', #21119, #17125, #11455, .T. ) ;
#14116 = CARTESIAN_POINT ( 'NONE',  ( 4.964892671625814380, 16.28226395658652237, 6.310736198168394928 ) ) ;
#14117 = EDGE_CURVE ( 'NONE', #3636, #24493, #19149, .T. ) ;
#14118 = AXIS2_PLACEMENT_3D ( 'NONE', #25598, #18118, #27942 ) ;
#14119 = ORIENTED_EDGE ( 'NONE', *, *, #19172, .T. ) ;
#14120 = AXIS2_PLACEMENT_3D ( 'NONE', #14505, #22134, #9672 ) ;
#14121 = CARTESIAN_POINT ( 'NONE',  ( 11.70346162051517780, 12.43461153239108441, 6.995624166085161910 ) ) ;
#14122 = CARTESIAN_POINT ( 'NONE',  ( -4.622016212553093695, -12.19167610014704906, 1.500000000000001332 ) ) ;
#14123 = CARTESIAN_POINT ( 'NONE',  ( -15.22124877282432465, 34.27704336327021650, 37.50000000002827250 ) ) ;
#14124 = VERTEX_POINT ( 'NONE', #193 ) ;
#14125 = DIRECTION ( 'NONE',  ( -0.000000000000000000, -0.000000000000000000, 1.000000000000000000 ) ) ;
#14126 = DIRECTION ( 'NONE',  ( 0.000000000000000000, 1.000000000000000000, 1.193512090021232842E-16 ) ) ;
#14127 = CARTESIAN_POINT ( 'NONE',  ( -7.028330626922778990, 10.93629592680536788, 24.50000000000000000 ) ) ;
#14128 = ORIENTED_EDGE ( 'NONE', *, *, #3316, .F. ) ;
#14129 = CARTESIAN_POINT ( 'NONE',  ( -18.46504858183722675, -7.730374101464832393, 6.420335371522007506 ) ) ;
#14130 = CARTESIAN_POINT ( 'NONE',  ( 26.80246859415415273, 7.028748154183637631, -6.500000000000000888 ) ) ;
#14131 = ADVANCED_FACE ( 'NONE', ( #10174 ), #26242, .F. ) ;
#14132 = DIRECTION ( 'NONE',  ( 1.000000000000000000, 0.000000000000000000, 0.000000000000000000 ) ) ;
#14133 = EDGE_CURVE ( 'NONE', #18371, #29096, #24139, .T. ) ;
#14134 = CARTESIAN_POINT ( 'NONE',  ( 16.18102710830015667, -40.48237095587791856, -16.50000000000000355 ) ) ;
#14135 = B_SPLINE_SURFACE_WITH_KNOTS ( 'NONE', 3, 1, ( 
 ( #24626, #19794 ),
 ( #8114, #17621 ),
 ( #21667, #7494 ),
 ( #15254, #24786 ),
 ( #5142, #304 ),
 ( #28863, #16992 ),
 ( #24156, #12327 ),
 ( #9987, #25097 ),
 ( #10751, #22903 ),
 ( #1405, #1245 ),
 ( #20564, #20262 ),
 ( #15580, #29787 ),
 ( #8263, #18406 ),
 ( #15902, #8429 ),
 ( #15420, #16045 ),
 ( #12949, #11063 ),
 ( #17939, #27911 ),
 ( #27448, #25415 ),
 ( #1552, #25249 ),
 ( #11210, #6069 ),
 ( #10918, #13257 ),
 ( #20112, #22595 ),
 ( #3740, #1695 ),
 ( #22746, #20421 ),
 ( #29942, #6536 ),
 ( #30237, #24942 ),
 ( #8579, #18085 ),
 ( #27602, #6224 ),
 ( #20707, #15731 ),
 ( #25561, #30086 ),
 ( #22442, #8882 ) ),
 .UNSPECIFIED., .F., .F., .F.,
 ( 4, 3, 3, 3, 3, 3, 3, 3, 3, 3, 4 ),
 ( 2, 2 ),
 ( 0.000000000000000000, 0.05425176834609633791, 0.1085332949128352958, 0.1623767749169382768, 0.2157504826133063158, 0.2688657508888171455, 0.3218907763505476360, 0.3749548578363336993, 0.4282048033836242107, 0.4818374082110501444, 0.4999999999131656825 ),
 ( 0.000000000000000000, 1.000000000000000000 ),
 .UNSPECIFIED. ) ;
#14136 = PLANE ( 'NONE',  #23215 ) ;
#14137 = ADVANCED_FACE ( 'NONE', ( #660 ), #19219, .F. ) ;
#14138 = LINE ( 'NONE', #4324, #29707 ) ;
#14139 = DIRECTION ( 'NONE',  ( 0.000000000000000000, 0.000000000000000000, 1.000000000000000000 ) ) ;
#14140 = AXIS2_PLACEMENT_3D ( 'NONE', #5720, #22251, #724 ) ;
#14141 = DIRECTION ( 'NONE',  ( 1.000000000000000000, 0.000000000000000000, 0.000000000000000000 ) ) ;
#14142 = DIRECTION ( 'NONE',  ( 1.000000000000000000, 0.000000000000000000, 0.000000000000000000 ) ) ;
#14143 = ORIENTED_EDGE ( 'NONE', *, *, #27858, .F. ) ;
#14144 = ADVANCED_FACE ( 'NONE', ( #12687 ), #23144, .T. ) ;
#14145 = CARTESIAN_POINT ( 'NONE',  ( 10.22519205257000507, -13.65449557370668465, 20.25542030744407640 ) ) ;
#14146 = CARTESIAN_POINT ( 'NONE',  ( -4.622016212553093695, -12.19167610014704906, 1.500000000000001332 ) ) ;
#14147 = ORIENTED_EDGE ( 'NONE', *, *, #11034, .T. ) ;
#14148 = ORIENTED_EDGE ( 'NONE', *, *, #9470, .T. ) ;
#14149 = EDGE_CURVE ( 'NONE', #4573, #21077, #244, .T. ) ;
#14150 = CARTESIAN_POINT ( 'NONE',  ( -25.10445388623454477, -25.60065097860747585, -1.500000000000000000 ) ) ;
#14151 = EDGE_CURVE ( 'NONE', #2092, #2473, #13218, .T. ) ;
#14152 = ORIENTED_EDGE ( 'NONE', *, *, #2678, .F. ) ;
#14153 = CARTESIAN_POINT ( 'NONE',  ( -47.00000000000000000, 87.00000000000001421, 22.49999999999999289 ) ) ;
#14154 = FACE_OUTER_BOUND ( 'NONE', #20066, .T. ) ;
#14155 = ORIENTED_EDGE ( 'NONE', *, *, #25631, .T. ) ;
#14156 = CARTESIAN_POINT ( 'NONE',  ( 16.13887868878509479, -5.569097860077073747, 19.89182036555910571 ) ) ;
#14157 = CARTESIAN_POINT ( 'NONE',  ( 19.57650873258266344, 4.179294809495488039, 19.14333282897057842 ) ) ;
#14158 = DIRECTION ( 'NONE',  ( -0.000000000000000000, -0.000000000000000000, 1.000000000000000000 ) ) ;
#14159 = EDGE_LOOP ( 'NONE', ( #14007, #4647, #20299, #23670 ) ) ;
#14160 = CARTESIAN_POINT ( 'NONE',  ( 1.492780340587499928E-15, -12.18947652193948272, -87.50000000000000000 ) ) ;
#14161 = AXIS2_PLACEMENT_3D ( 'NONE', #6538, #20711, #15906 ) ;
#14162 = VERTEX_POINT ( 'NONE', #7216 ) ;
#14163 = EDGE_CURVE ( 'NONE', #26039, #15359, #2695, .T. ) ;
#14164 = ORIENTED_EDGE ( 'NONE', *, *, #30202, .F. ) ;
#14165 = EDGE_CURVE ( 'NONE', #26054, #4436, #6364, .T. ) ;
#14166 = EDGE_CURVE ( 'NONE', #5019, #2261, #18677, .T. ) ;
#14167 = FACE_OUTER_BOUND ( 'NONE', #2157, .T. ) ;
#14168 = CARTESIAN_POINT ( 'NONE',  ( 0.7788148816922458861, -17.02744011591804707, 20.34789198813115263 ) ) ;
#14169 = CARTESIAN_POINT ( 'NONE',  ( 0.3493067888074735117, -20.01473451864462305, 7.652108011868850035 ) ) ;
#14170 = CARTESIAN_POINT ( 'NONE',  ( -14.58213539500865785, 7.758783772730382111, 1.500000000000000000 ) ) ;
#14171 = CARTESIAN_POINT ( 'NONE',  ( -23.09047454507859953, 11.74540567832116267, 49.09408197974163812 ) ) ;
#14172 = DIRECTION ( 'NONE',  ( 1.000000000000000000, 0.000000000000000000, 0.000000000000000000 ) ) ;
#14173 = ORIENTED_EDGE ( 'NONE', *, *, #10266, .F. ) ;
#14174 = CARTESIAN_POINT ( 'NONE',  ( 10.92346103252092604, -16.77505673787611329, 7.632642797338977658 ) ) ;
#14175 = DIRECTION ( 'NONE',  ( 0.000000000000000000, -1.132880637372608986E-16, 1.000000000000000000 ) ) ;
#14176 = CARTESIAN_POINT ( 'NONE',  ( -13.65791587866001855, 10.22062306005669363, 7.559636331181775581 ) ) ;
#14177 = LINE ( 'NONE', #2800, #4851 ) ;
#14178 = ORIENTED_EDGE ( 'NONE', *, *, #11303, .T. ) ;
#14179 = ORIENTED_EDGE ( 'NONE', *, *, #19079, .F. ) ;
#14180 = CIRCLE ( 'NONE', #28649, 0.6002263538043648428 ) ;
#14181 = DIRECTION ( 'NONE',  ( 0.000000000000000000, 0.000000000000000000, -1.000000000000000000 ) ) ;
#14182 = FACE_OUTER_BOUND ( 'NONE', #6989, .T. ) ;
#14183 = CARTESIAN_POINT ( 'NONE',  ( -4.776122516674677878E-15, -42.50000000000000000, 19.72227980406325543 ) ) ;
#14184 = LINE ( 'NONE', #25741, #2900 ) ;
#14185 = CARTESIAN_POINT ( 'NONE',  ( 12.35522425158189108, 11.74279415389956505, 5.652196082368482699 ) ) ;
#14186 = CARTESIAN_POINT ( 'NONE',  ( -2.492600117579355956, -39.42873062461828226, 27.50000000000000355 ) ) ;
#14187 = AXIS2_PLACEMENT_3D ( 'NONE', #21708, #7385, #12207 ) ;
#14188 = CARTESIAN_POINT ( 'NONE',  ( -10.18506332983503704, 29.04537757311073776, 24.50000000000000000 ) ) ;
#14189 = ORIENTED_EDGE ( 'NONE', *, *, #22201, .T. ) ;
#14190 = CARTESIAN_POINT ( 'NONE',  ( -19.95113275051131652, 1.631914050426796159, 6.131018562779544823 ) ) ;
#14191 = CARTESIAN_POINT ( 'NONE',  ( -5.687793815610304726, 6.974883619896852238, 21.50000000000000000 ) ) ;
#14192 = LINE ( 'NONE', #9378, #6980 ) ;
#14193 = ORIENTED_EDGE ( 'NONE', *, *, #2846, .T. ) ;
#14194 = CARTESIAN_POINT ( 'NONE',  ( -12.66227964008306550, -1.387778780781445676E-14, -1.500000000000000000 ) ) ;
#14195 = ORIENTED_EDGE ( 'NONE', *, *, #10591, .T. ) ;
#14196 = ADVANCED_FACE ( 'NONE', ( #28592 ), #24367, .F. ) ;
#14197 = CARTESIAN_POINT ( 'NONE',  ( 18.52707432543149579, -7.580618987226253935, 5.749491821935610147 ) ) ;
#14198 = UNCERTAINTY_MEASURE_WITH_UNIT (LENGTH_MEASURE( 1.000000000000000082E-05 ), #29664, 'distance_accuracy_value', 'NONE');
#14199 = CARTESIAN_POINT ( 'NONE',  ( -2.959227181723746547, 8.499586724479465616, 1.500000000000001332 ) ) ;
#14200 = ORIENTED_EDGE ( 'NONE', *, *, #12681, .F. ) ;
#14201 = CARTESIAN_POINT ( 'NONE',  ( 34.43169391940249113, -11.54542193137334394, 27.50000000000000355 ) ) ;
#14202 = DIRECTION ( 'NONE',  ( -0.000000000000000000, 1.000000000000000000, -0.000000000000000000 ) ) ;
#14203 = CARTESIAN_POINT ( 'NONE',  ( 10.58819075803338450, -13.39403179698972934, 18.84329447212443753 ) ) ;
#14204 = CARTESIAN_POINT ( 'NONE',  ( 4.510281037539698445E-13, -4.926614671774132148E-13, 77.49999999999998579 ) ) ;
#14205 = CARTESIAN_POINT ( 'NONE',  ( -10.62409560796092833, -16.94539057243558489, 5.651480102388687143 ) ) ;
#14206 = CARTESIAN_POINT ( 'NONE',  ( -30.74201181684194850, 15.50830195949553669, 40.56825029441224473 ) ) ;
#14207 = ORIENTED_EDGE ( 'NONE', *, *, #20809, .T. ) ;
#14208 = CARTESIAN_POINT ( 'NONE',  ( -2.081668171172168513E-14, 75.00000000000001421, 37.49999999999999289 ) ) ;
#14209 = CARTESIAN_POINT ( 'NONE',  ( -39.83602371821029919, -11.57901747687044924, -19.50000000000000355 ) ) ;
#14210 = VECTOR ( 'NONE', #1651, 1000.000000000000000 ) ;
#14211 = CARTESIAN_POINT ( 'NONE',  ( 25.47847050916411504, 26.57182937991349903, 26.54355021145563143 ) ) ;
#14212 = ORIENTED_EDGE ( 'NONE', *, *, #25949, .F. ) ;
#14213 = DIRECTION ( 'NONE',  ( 0.000000000000000000, 0.000000000000000000, 1.000000000000000000 ) ) ;
#14214 = CARTESIAN_POINT ( 'NONE',  ( -17.99620775894062419, -8.766556869501986426, 20.33971507717571114 ) ) ;
#14215 = DIRECTION ( 'NONE',  ( -0.000000000000000000, -0.000000000000000000, -1.000000000000000000 ) ) ;
#14216 = CARTESIAN_POINT ( 'NONE',  ( 4.172444469722463189, 16.52351170763985877, 5.651492010659114662 ) ) ;
#14217 = CYLINDRICAL_SURFACE ( 'NONE', #22564, 9.482273699623480212 ) ;
#14218 = VERTEX_POINT ( 'NONE', #12372 ) ;
#14219 = DIRECTION ( 'NONE',  ( 0.000000000000000000, 0.000000000000000000, -1.000000000000000000 ) ) ;
#14220 = AXIS2_PLACEMENT_3D ( 'NONE', #19062, #28282, #16420 ) ;
#14221 = DIRECTION ( 'NONE',  ( -0.000000000000000000, -0.000000000000000000, -1.000000000000000000 ) ) ;
#14222 = CARTESIAN_POINT ( 'NONE',  ( 27.16566537401950043, 25.85840940979817049, 37.50000000000431299 ) ) ;
#14223 = LINE ( 'NONE', #23736, #30507 ) ;
#14224 = ORIENTED_EDGE ( 'NONE', *, *, #3242, .T. ) ;
#14225 = CIRCLE ( 'NONE', #10754, 0.7500000000000002220 ) ;
#14226 = ORIENTED_EDGE ( 'NONE', *, *, #11106, .T. ) ;
#14227 = DIRECTION ( 'NONE',  ( 0.000000000000000000, 0.000000000000000000, 1.000000000000000000 ) ) ;
#14228 = CARTESIAN_POINT ( 'NONE',  ( -43.34097750826428097, -11.89502811014147987, 1.500000000000000444 ) ) ;
#14229 = ORIENTED_EDGE ( 'NONE', *, *, #7075, .F. ) ;
#14230 = ORIENTED_EDGE ( 'NONE', *, *, #4837, .F. ) ;
#14231 = CYLINDRICAL_SURFACE ( 'NONE', #24720, 3.000000000000002665 ) ;
#14232 = VERTEX_POINT ( 'NONE', #17040 ) ;
#14233 = ORIENTED_EDGE ( 'NONE', *, *, #21494, .T. ) ;
#14234 = CARTESIAN_POINT ( 'NONE',  ( 0.3346962451677067962, -17.03061174119336840, 20.25336174263950184 ) ) ;
#14235 = DIRECTION ( 'NONE',  ( 1.000000000000000000, 0.000000000000000000, 0.000000000000000000 ) ) ;
#14236 = CARTESIAN_POINT ( 'NONE',  ( 1.265447379378154436, -19.97763032565216790, 19.79423548914561692 ) ) ;
#14237 = ORIENTED_EDGE ( 'NONE', *, *, #24407, .F. ) ;
#14238 = CARTESIAN_POINT ( 'NONE',  ( 18.57699708025013052, -7.409721753143990952, 5.853797745100183469 ) ) ;
#14239 = AXIS2_PLACEMENT_3D ( 'NONE', #1397, #25408, #29935 ) ;
#14240 = CARTESIAN_POINT ( 'NONE',  ( 0.000000000000000000, 0.000000000000000000, -1.500000000000000000 ) ) ;
#14241 = CARTESIAN_POINT ( 'NONE',  ( 14.30907656312162679, 13.99861481489062598, 19.89182036555910571 ) ) ;
#14242 = VERTEX_POINT ( 'NONE', #26566 ) ;
#14243 = CIRCLE ( 'NONE', #14319, 0.7500000000000024425 ) ;
#14244 = VECTOR ( 'NONE', #29374, 1000.000000000000227 ) ;
#14245 = CARTESIAN_POINT ( 'NONE',  ( 0.000000000000000000, 0.000000000000000000, 85.49999999999998579 ) ) ;
#14246 = CARTESIAN_POINT ( 'NONE',  ( -17.59781475975453446, -9.540531696329381361, 6.560937769032974209 ) ) ;
#14247 = CARTESIAN_POINT ( 'NONE',  ( 12.24063095261064404, 4.490763173670002217, 1.500000000000001332 ) ) ;
#14248 = CARTESIAN_POINT ( 'NONE',  ( -19.90071050938331609, 1.994113959836041783, 7.528076282304594358 ) ) ;
#14249 = CYLINDRICAL_SURFACE ( 'NONE', #10425, 0.7500000000000006661 ) ;
#14250 = CARTESIAN_POINT ( 'NONE',  ( -15.34842816977634428, -7.387654668753816267, 18.44501272782439827 ) ) ;
#14251 = CARTESIAN_POINT ( 'NONE',  ( 37.99999999999999289, 65.00000000000000000, 50.49999999999998579 ) ) ;
#14252 = CIRCLE ( 'NONE', #27705, 0.7500000000000006661 ) ;
#14253 = VERTEX_POINT ( 'NONE', #508 ) ;
#14254 = ORIENTED_EDGE ( 'NONE', *, *, #26518, .T. ) ;
#14255 = CARTESIAN_POINT ( 'NONE',  ( 33.46566279634969021, 23.92259740141769342, -11.49999999999999822 ) ) ;
#14256 = CIRCLE ( 'NONE', #29216, 9.084132297865673777 ) ;
#14257 = CARTESIAN_POINT ( 'NONE',  ( -37.98493438988128901, 11.12428508575241004, -1.500000000000000000 ) ) ;
#14258 = CARTESIAN_POINT ( 'NONE',  ( 32.19782014694308003, -14.25394737442115201, 35.54550565580006349 ) ) ;
#14259 = CARTESIAN_POINT ( 'NONE',  ( 11.83518757993566695, -16.12237520560631765, 18.84486140012300481 ) ) ;
#14260 = ORIENTED_EDGE ( 'NONE', *, *, #4183, .T. ) ;
#14261 = DIRECTION ( 'NONE',  ( 1.000000000000000000, 0.000000000000000000, 0.000000000000000000 ) ) ;
#14262 = CARTESIAN_POINT ( 'NONE',  ( 17.93514094173302453, -8.890850898656898593, 19.56050940960062690 ) ) ;
#14263 = CIRCLE ( 'NONE', #10289, 11.99999999999999645 ) ;
#14264 = CARTESIAN_POINT ( 'NONE',  ( 4.159666964149448809, 16.52698801271858287, 7.652108011868850035 ) ) ;
#14265 = EDGE_CURVE ( 'NONE', #8229, #1903, #14313, .T. ) ;
#14266 = TOROIDAL_SURFACE ( 'NONE', #15268, 53.00000000000000711, 3.000000000000000000 ) ;
#14267 = ORIENTED_EDGE ( 'NONE', *, *, #68, .F. ) ;
#14268 = CARTESIAN_POINT ( 'NONE',  ( 4.917955972067796111, 16.29747060413736648, 18.90679857307105749 ) ) ;
#14269 = LINE ( 'NONE', #9462, #778 ) ;
#14270 = AXIS2_PLACEMENT_3D ( 'NONE', #26270, #4909, #19248 ) ;
#14271 = DIRECTION ( 'NONE',  ( -0.000000000000000000, -0.000000000000000000, 1.000000000000000000 ) ) ;
#14272 = CARTESIAN_POINT ( 'NONE',  ( -26.07963561311912670, 31.61094817644626076, 34.51864978005331608 ) ) ;
#14273 = ORIENTED_EDGE ( 'NONE', *, *, #21531, .T. ) ;
#14274 = CARTESIAN_POINT ( 'NONE',  ( -77.99999999999998579, 42.50000000000000000, 1.500000000000000222 ) ) ;
#14275 = ADVANCED_FACE ( 'NONE', ( #22023 ), #3781, .T. ) ;
#14276 = DIRECTION ( 'NONE',  ( 0.000000000000000000, 0.000000000000000000, 1.000000000000000000 ) ) ;
#14277 = CARTESIAN_POINT ( 'NONE',  ( -31.31394823341925715, -25.51108937476197980, -1.500000000000000000 ) ) ;
#14278 = CIRCLE ( 'NONE', #4315, 0.7500000000000006661 ) ;
#14279 = EDGE_LOOP ( 'NONE', ( #26610, #2704, #9954, #11835 ) ) ;
#14280 = CARTESIAN_POINT ( 'NONE',  ( -15.16517292768934411, -7.781889190071454188, 7.652108011868850035 ) ) ;
#14281 = CARTESIAN_POINT ( 'NONE',  ( -37.16608720827707657, -65.00000000000000000, 97.07879600563551037 ) ) ;
#14282 = CARTESIAN_POINT ( 'NONE',  ( -70.00000000000000000, 65.00000000000000000, 12.49999999999999112 ) ) ;
#14283 = CARTESIAN_POINT ( 'NONE',  ( -0.6606983433884106027, -20.00701505202155417, 6.755862304746362845 ) ) ;
#14284 = CIRCLE ( 'NONE', #3845, 1.000000000000004441 ) ;
#14285 = DIRECTION ( 'NONE',  ( -0.000000000000000000, -0.000000000000000000, -1.000000000000000000 ) ) ;
#14287 = ADVANCED_FACE ( 'NONE', ( #17984 ), #12989, .F. ) ;
#14286 = AXIS2_PLACEMENT_3D ( 'NONE', #15280, #22457, #1106 ) ;
#14288 = FACE_OUTER_BOUND ( 'NONE', #22664, .T. ) ;
#14289 = CARTESIAN_POINT ( 'NONE',  ( -16.97424920726489006, 1.578583718960127280, 20.34789198813115263 ) ) ;
#14290 = CARTESIAN_POINT ( 'NONE',  ( -8.413215745754975217, 3.196529495465474380, -1.500000000000001332 ) ) ;
#14291 = ORIENTED_EDGE ( 'NONE', *, *, #28016, .F. ) ;
#14292 = CARTESIAN_POINT ( 'NONE',  ( 10.64246886845954521, -13.35396698543973137, 19.69140814234746273 ) ) ;
#14293 = CARTESIAN_POINT ( 'NONE',  ( 5.687793815610356241, -6.974883619896809606, -1.500000000000002665 ) ) ;
#14294 = ORIENTED_EDGE ( 'NONE', *, *, #25998, .T. ) ;
#14295 = ORIENTED_EDGE ( 'NONE', *, *, #9142, .F. ) ;
#14296 = AXIS2_PLACEMENT_3D ( 'NONE', #24228, #24077, #11943 ) ;
#14297 = CARTESIAN_POINT ( 'NONE',  ( -12.99194183819582449, 48.28319231324876171, -47.48680334385887392 ) ) ;
#14298 = FACE_OUTER_BOUND ( 'NONE', #12450, .T. ) ;
#14299 = AXIS2_PLACEMENT_3D ( 'NONE', #29962, #13591, #25587 ) ;
#14300 = VERTEX_POINT ( 'NONE', #20315 ) ;
#14301 = AXIS2_PLACEMENT_3D ( 'NONE', #26868, #12519, #10160 ) ;
#14302 = CARTESIAN_POINT ( 'NONE',  ( 15.31432103507273546, 12.89133701742166949, 20.12545155307891065 ) ) ;
#14303 = B_SPLINE_CURVE_WITH_KNOTS ( 'NONE', 3,
 ( #1102, #17634, #22454, #6081, #11076, #13116, #27307, #10934, #6238, #17953, #10613, #27462, #22609, #29337, #15744, #25265 ),
 .UNSPECIFIED., .F., .F.,
 ( 4, 2, 2, 2, 2, 2, 2, 4 ),
 ( 0.5000000000000000000, 0.6250000000000017764, 0.6875000000000025535, 0.7187500000000028866, 0.7500000000000033307, 0.8125000000000022204, 0.8750000000000013323, 1.000000000000000000 ),
 .UNSPECIFIED. ) ;
#14304 = EDGE_CURVE ( 'NONE', #30200, #19542, #17062, .T. ) ;
#14305 = CARTESIAN_POINT ( 'NONE',  ( -8.550548368345317840, -14.74545326172986925, 7.652108011868850035 ) ) ;
#14306 = CLOSED_SHELL ( 'NONE', ( #29193, #17137, #27110, #243, #19734, #30793, #9364, #5395, #17637, #1972, #26348, #12438, #30139, #12965, #14882, #5187, #22745, #12262, #12502, #6505, #4406, #2152, #19642, #5005, #23295, #2729, #3276, #2883, #15212, #10359, #234, #11525, #18307, #1947, #2992, #13433, #24889, #9216, #6518, #16154, #24603, #11464, #5556, #9003, #18699, #21420, #10930, #11340, #6329, #30509, #483, #27349, #14358, #18172, #12281, #7436, #19497, #14671, #26745, #20791, #6897, #27, #26522, #8793, #17134, #28823, #552, #15371, #1215, #16656, #21406, #29620, #422, #4431, #26951, #18004, #11678, #11829, #3300, #8629, #20234, #19507, #15297, #7000, #17964, #11542, #4247, #26765, #12615, #15514, #5181, #17749, #2563, #11895, #2138, #21394, #22314, #19704, #10134 ) ) ;
#14307 = ORIENTED_EDGE ( 'NONE', *, *, #7718, .F. ) ;
#14308 = EDGE_CURVE ( 'NONE', #466, #3526, #7624, .T. ) ;
#14309 = CARTESIAN_POINT ( 'NONE',  ( 18.56338958360293390, -7.490577753534553018, 18.50655187082627862 ) ) ;
#14310 = CARTESIAN_POINT ( 'NONE',  ( 16.58472157312808193, 4.055073576757204812, 18.82680253904184298 ) ) ;
#14311 = AXIS2_PLACEMENT_3D ( 'NONE', #7656, #5152, #14973 ) ;
#14312 = DIRECTION ( 'NONE',  ( 1.000000000000000000, 0.000000000000000000, 0.000000000000000000 ) ) ;
#14313 = CIRCLE ( 'NONE', #6286, 0.7500000000000006661 ) ;
#14314 = ORIENTED_EDGE ( 'NONE', *, *, #29046, .T. ) ;
#14315 = CIRCLE ( 'NONE', #13847, 0.7499999999999997780 ) ;
#14316 = CARTESIAN_POINT ( 'NONE',  ( 15.38611090871061293, -7.279566334535328309, 19.21496526180054332 ) ) ;
#14317 = ORIENTED_EDGE ( 'NONE', *, *, #4787, .F. ) ;
#14318 = EDGE_CURVE ( 'NONE', #11562, #34, #11511, .T. ) ;
#14319 = AXIS2_PLACEMENT_3D ( 'NONE', #19697, #5826, #24854 ) ;
#14320 = VERTEX_POINT ( 'NONE', #6266 ) ;
#14321 = EDGE_CURVE ( 'NONE', #17470, #9984, #22636, .T. ) ;
#14322 = VECTOR ( 'NONE', #16225, 1000.000000000000000 ) ;
#14323 = ADVANCED_FACE ( 'NONE', ( #22798 ), #18131, .F. ) ;
#14324 = DIRECTION ( 'NONE',  ( -0.2972711322815276280, -0.9547931052914334638, 0.000000000000000000 ) ) ;
#14325 = CARTESIAN_POINT ( 'NONE',  ( 0.01899995639454398616, -8.236198097127184425, -3.734486434573641933 ) ) ;
#14326 = AXIS2_PLACEMENT_3D ( 'NONE', #25926, #20485, #3965 ) ;
#14327 = EDGE_CURVE ( 'NONE', #14013, #11387, #12330, .T. ) ;
#14328 = AXIS2_PLACEMENT_3D ( 'NONE', #5413, #9774, #19291 ) ;
#14329 = CARTESIAN_POINT ( 'NONE',  ( 1.365674945463512424, -19.97097327164667391, 6.672349528511551497 ) ) ;
#14330 = ADVANCED_FACE ( 'NONE', ( #13468 ), #27182, .F. ) ;
#14331 = CARTESIAN_POINT ( 'NONE',  ( -14.70620249426369242, -8.682611668020191686, 19.21769074125272425 ) ) ;
#14332 = CARTESIAN_POINT ( 'NONE',  ( -24.35970437652574105, 13.37404834226503247, 47.21042702067971675 ) ) ;
#14333 = CARTESIAN_POINT ( 'NONE',  ( 4.770489558936219510E-15, -42.50000000000000000, -1.500000000000000000 ) ) ;
#14334 = EDGE_LOOP ( 'NONE', ( #10822, #10049, #14233, #24335 ) ) ;
#14335 = CARTESIAN_POINT ( 'NONE',  ( 39.52380524533145945, -7.028748154382054913, -1.499999999999999556 ) ) ;
#14336 = CARTESIAN_POINT ( 'NONE',  ( 23.21352257770656635, -10.78826658734920052, 45.15942333309103418 ) ) ;
#14337 = VECTOR ( 'NONE', #13191, 1000.000000000000114 ) ;
#14338 = CARTESIAN_POINT ( 'NONE',  ( -15.69442553397265883, 12.42550873695621938, 7.500147780736496017 ) ) ;
#14339 = CYLINDRICAL_SURFACE ( 'NONE', #4339, 2.000000000000005329 ) ;
#14340 = ORIENTED_EDGE ( 'NONE', *, *, #16209, .T. ) ;
#14341 = VERTEX_POINT ( 'NONE', #10333 ) ;
#14342 = VECTOR ( 'NONE', #9086, 1000.000000000000000 ) ;
#14343 = FACE_OUTER_BOUND ( 'NONE', #29454, .T. ) ;
#14344 = CARTESIAN_POINT ( 'NONE',  ( 24.49591551883469265, -22.99161772365830814, -16.50001200000000523 ) ) ;
#14345 = DIRECTION ( 'NONE',  ( 1.000000000000000000, 0.000000000000000000, -0.000000000000000000 ) ) ;
#14346 = FACE_OUTER_BOUND ( 'NONE', #9070, .T. ) ;
#14347 = CARTESIAN_POINT ( 'NONE',  ( 0.000000000000000000, 0.000000000000000000, -11.49999999999999645 ) ) ;
#14348 = CARTESIAN_POINT ( 'NONE',  ( -19.70185583149091002, -33.06308933231057523, 27.50000000000000355 ) ) ;
#14349 = EDGE_CURVE ( 'NONE', #254, #19220, #6738, .T. ) ;
#14350 = CARTESIAN_POINT ( 'NONE',  ( 2.168404344971008868E-16, 30.50000000000000000, 1.500000000000001332 ) ) ;
#14351 =( GEOMETRIC_REPRESENTATION_CONTEXT ( 3 ) GLOBAL_UNCERTAINTY_ASSIGNED_CONTEXT ( ( #17008 ) ) GLOBAL_UNIT_ASSIGNED_CONTEXT ( ( #9640, #2297, #4337 ) ) REPRESENTATION_CONTEXT ( 'NONE', 'WORKASPACE' ) );
#14352 = VERTEX_POINT ( 'NONE', #10642 ) ;
#14353 = EDGE_CURVE ( 'NONE', #24910, #5531, #17827, .T. ) ;
#14354 = AXIS2_PLACEMENT_3D ( 'NONE', #7275, #257, #28957 ) ;
#14355 = CARTESIAN_POINT ( 'NONE',  ( -5.095241848980792021, -39.11820605553161556, 34.50000000000000000 ) ) ;
#14356 = VECTOR ( 'NONE', #16980, 1000.000000000000000 ) ;
#14357 = CARTESIAN_POINT ( 'NONE',  ( -17.81964242321468461, -9.081580984160163794, 20.22386025856690139 ) ) ;
#14358 = ADVANCED_FACE ( 'NONE', ( #6257 ), #22629, .F. ) ;
#14359 = DIRECTION ( 'NONE',  ( 0.000000000000000000, 0.000000000000000000, 1.000000000000000000 ) ) ;
#14360 = VERTEX_POINT ( 'NONE', #20456 ) ;
#14361 = CARTESIAN_POINT ( 'NONE',  ( 15.45595318746689095, 12.72131790141721375, 6.111214848085761986 ) ) ;
#14362 = ADVANCED_FACE ( 'NONE', ( #25290 ), #10789, .F. ) ;
#14363 = VERTEX_POINT ( 'NONE', #18580 ) ;
#14364 = CARTESIAN_POINT ( 'NONE',  ( 49.99999999999998579, -50.00000000000000000, 12.49999999999999112 ) ) ;
#14365 = EDGE_CURVE ( 'NONE', #8763, #1352, #30119, .T. ) ;
#14366 = AXIS2_PLACEMENT_3D ( 'NONE', #7809, #24337, #12503 ) ;
#14367 = CARTESIAN_POINT ( 'NONE',  ( -4.183878327245746931, 43.84516588455117869, -16.50000000000000000 ) ) ;
#14368 = ORIENTED_EDGE ( 'NONE', *, *, #11276, .F. ) ;
#14369 = CARTESIAN_POINT ( 'NONE',  ( 23.90632052215872605, 29.53616140628007614, 27.50000000000000355 ) ) ;
#14370 = EDGE_CURVE ( 'NONE', #4649, #25953, #25085, .T. ) ;
#14371 = CARTESIAN_POINT ( 'NONE',  ( -24.44496207165490276, -7.595930209050158588, 49.40206402021039622 ) ) ;
#14372 = CARTESIAN_POINT ( 'NONE',  ( 10.52561254568492011, -13.43997246243151267, 19.96568007040468729 ) ) ;
#14373 = DIRECTION ( 'NONE',  ( 0.000000000000000000, 1.000000000000000000, 0.000000000000000000 ) ) ;
#14374 = CARTESIAN_POINT ( 'NONE',  ( -29.15452456067357545, -29.11038375075818152, -6.500000000000000888 ) ) ;
#14375 = CARTESIAN_POINT ( 'NONE',  ( 22.58267429318974706, -26.57182937991349903, 1.500000000000000000 ) ) ;
#14376 = PRODUCT_DEFINITION_FORMATION_WITH_SPECIFIED_SOURCE ( 'ANY', '', #23856, .NOT_KNOWN. ) ;
#14377 = EDGE_LOOP ( 'NONE', ( #29140, #27427, #4969, #172 ) ) ;
#14378 = FACE_OUTER_BOUND ( 'NONE', #22105, .T. ) ;
#14379 = AXIS2_PLACEMENT_3D ( 'NONE', #14245, #7561, #14719 ) ;
#14380 = AXIS2_PLACEMENT_3D ( 'NONE', #13365, #15206, #8681 ) ;
#14381 = CARTESIAN_POINT ( 'NONE',  ( 31.18700685317022803, -26.11823559933272421, -1.500000000000000000 ) ) ;
#14382 = DIRECTION ( 'NONE',  ( -0.000000000000000000, -0.000000000000000000, -1.000000000000000000 ) ) ;
#14383 = EDGE_LOOP ( 'NONE', ( #10919, #30106 ) ) ;
#14384 = DIRECTION ( 'NONE',  ( -1.000000000000000000, 0.000000000000000000, 0.000000000000000000 ) ) ;
#14385 = DIRECTION ( 'NONE',  ( 0.000000000000000000, -1.132880637372608986E-16, 1.000000000000000000 ) ) ;
#14386 = CARTESIAN_POINT ( 'NONE',  ( 0.000000000000000000, -2.435693370351110282E-15, 21.50000000000000355 ) ) ;
#14387 = EDGE_CURVE ( 'NONE', #15666, #4693, #23202, .T. ) ;
#14388 = DIRECTION ( 'NONE',  ( 1.000000000000000000, 0.000000000000000000, 0.000000000000000000 ) ) ;
#14389 = EDGE_CURVE ( 'NONE', #10056, #165, #22938, .T. ) ;
#14390 = CARTESIAN_POINT ( 'NONE',  ( -5.738360882150000286, -7.548823014270624299, 13.00000000000000178 ) ) ;
#14391 = AXIS2_PLACEMENT_3D ( 'NONE', #13215, #18047, #27562 ) ;
#14392 = ORIENTED_EDGE ( 'NONE', *, *, #3093, .F. ) ;
#14393 = CARTESIAN_POINT ( 'NONE',  ( 37.16608720827707657, -65.00000000000000000, 97.07879600563551037 ) ) ;
#14394 = CARTESIAN_POINT ( 'NONE',  ( 38.97083381611543729, -2.113745753963891083, 35.07647338176046503 ) ) ;
#14395 = LINE ( 'NONE', #28439, #2125 ) ;
#14396 = EDGE_LOOP ( 'NONE', ( #7217, #16049, #15687, #21885 ) ) ;
#14397 =( GEOMETRIC_REPRESENTATION_CONTEXT ( 3 ) GLOBAL_UNCERTAINTY_ASSIGNED_CONTEXT ( ( #4848 ) ) GLOBAL_UNIT_ASSIGNED_CONTEXT ( ( #21403, #7212, #23900 ) ) REPRESENTATION_CONTEXT ( 'NONE', 'WORKASPACE' ) );
#14398 = DIRECTION ( 'NONE',  ( 1.000000000000000000, 0.000000000000000000, 0.000000000000000000 ) ) ;
#14399 = VERTEX_POINT ( 'NONE', #1729 ) ;
#14400 = B_SPLINE_CURVE_WITH_KNOTS ( 'NONE', 3,
 ( #8091, #17595, #27113, #15228, #24757, #8704 ),
 .UNSPECIFIED., .F., .F.,
 ( 4, 2, 4 ),
 ( 1.408367944307646891, 1.570796326794821507, 1.733224709277370712 ),
 .UNSPECIFIED. ) ;
#14401 = CYLINDRICAL_SURFACE ( 'NONE', #1249, 7.500000000000000000 ) ;
#14402 = DIRECTION ( 'NONE',  ( 1.000000000000000000, 0.000000000000000000, 0.000000000000000000 ) ) ;
#14403 = ORIENTED_EDGE ( 'NONE', *, *, #27123, .T. ) ;
#14404 = ORIENTED_EDGE ( 'NONE', *, *, #45, .F. ) ;
#14405 = CARTESIAN_POINT ( 'NONE',  ( -29.81956388892670518, -15.48018185647901213, 37.15911814917528488 ) ) ;
#14406 = ORIENTED_EDGE ( 'NONE', *, *, #19646, .T. ) ;
#14407 = PRODUCT_DEFINITION_SHAPE ( 'NONE', 'NONE',  #24773 ) ;
#14408 =( REPRESENTATION_RELATIONSHIP ('NONE','NONE', #19885, #10497 ) REPRESENTATION_RELATIONSHIP_WITH_TRANSFORMATION ( #25748 )SHAPE_REPRESENTATION_RELATIONSHIP( ) );
#14409 = AXIS2_PLACEMENT_3D ( 'NONE', #1509, #17715, #8536 ) ;
#14410 = ORIENTED_EDGE ( 'NONE', *, *, #27534, .T. ) ;
#14411 = ORIENTED_EDGE ( 'NONE', *, *, #6087, .F. ) ;
#14412 = CARTESIAN_POINT ( 'NONE',  ( 0.2396382576306451684, -20.01636569787184783, 18.35377592296120497 ) ) ;
#14413 = CARTESIAN_POINT ( 'NONE',  ( 0.000000000000000000, 39.50000000000000000, 27.50000000000000355 ) ) ;
#14414 = DIRECTION ( 'NONE',  ( 1.000000000000000000, 0.000000000000000000, 0.000000000000000000 ) ) ;
#14415 = AXIS2_PLACEMENT_3D ( 'NONE', #29403, #20179, #6000 ) ;
#14416 = CARTESIAN_POINT ( 'NONE',  ( 1.000541756189970544, -17.02230863066393241, 20.32367522806703874 ) ) ;
#14417 = EDGE_LOOP ( 'NONE', ( #29938, #2004, #1709, #30335 ) ) ;
#14418 = DIRECTION ( 'NONE',  ( 0.000000000000000000, 1.000000000000000000, 0.000000000000000000 ) ) ;
#14419 = PLANE ( 'NONE',  #26316 ) ;
#14420 = CARTESIAN_POINT ( 'NONE',  ( 14.40720023010962336, 13.89764844773314678, 20.06253562465620632 ) ) ;
#14421 = CARTESIAN_POINT ( 'NONE',  ( 30.53339558441486190, 7.800891647352844238, 39.24389099736750808 ) ) ;
#14422 = EDGE_LOOP ( 'NONE', ( #14530, #2056, #27008, #25339 ) ) ;
#14423 = AXIS2_PLACEMENT_3D ( 'NONE', #18454, #9383, #28410 ) ;
#14424 = CARTESIAN_POINT ( 'NONE',  ( -2.094186647214681063, 9.248129367672087042, 21.50000000000000000 ) ) ;
#14425 = CARTESIAN_POINT ( 'NONE',  ( -14.70315170625143075, -8.688231105434647716, 6.672349528511551497 ) ) ;
#14426 = CARTESIAN_POINT ( 'NONE',  ( -6.493275194760118829, 15.79517802630852152, 6.447548852708279377 ) ) ;
#14427 = CARTESIAN_POINT ( 'NONE',  ( -19.86062922652984142, 2.360743482685565997, 5.652912763329822177 ) ) ;
#14428 = CARTESIAN_POINT ( 'NONE',  ( 4.770489558936219510E-15, -42.50000000000000000, -1.500000000000000000 ) ) ;
#14429 = CARTESIAN_POINT ( 'NONE',  ( 37.99999999999999289, 90.00000000000001421, -34.50000000000000000 ) ) ;
#14430 = DIRECTION ( 'NONE',  ( -0.000000000000000000, -0.000000000000000000, 1.000000000000000000 ) ) ;
#14431 = ORIENTED_EDGE ( 'NONE', *, *, #28215, .F. ) ;
#14432 = EDGE_LOOP ( 'NONE', ( #28614, #30639 ) ) ;
#14433 = CARTESIAN_POINT ( 'NONE',  ( 25.64627119138473432, 23.40052582045089480, -16.50000000000000000 ) ) ;
#14434 = EDGE_CURVE ( 'NONE', #12485, #23974, #1591, .T. ) ;
#14435 = CARTESIAN_POINT ( 'NONE',  ( -15.35487586320816078, 12.84287697592353084, 7.652108011868850035 ) ) ;
#14436 = DIRECTION ( 'NONE',  ( -1.000000000000000000, 0.000000000000000000, 0.000000000000000000 ) ) ;
#14437 = ORIENTED_EDGE ( 'NONE', *, *, #5745, .F. ) ;
#14438 = ITEM_DEFINED_TRANSFORMATION ( 'NONE', 'NONE', #22350,  #7396 ) ;
#14439 = CIRCLE ( 'NONE', #7973, 11.46182693247429718 ) ;
#14440 = DIRECTION ( 'NONE',  ( 0.4154150130018859910, 0.9096319953545186632, 0.000000000000000000 ) ) ;
#14441 = CARTESIAN_POINT ( 'NONE',  ( 5.627515464934154110, 19.21053377385552707, 7.595116371587256054 ) ) ;
#14442 = ORIENTED_EDGE ( 'NONE', *, *, #20194, .T. ) ;
#14443 = CARTESIAN_POINT ( 'NONE',  ( 6.275630943545793983, 19.00876817605120195, 19.33715507985239412 ) ) ;
#14444 = DIRECTION ( 'NONE',  ( 0.000000000000000000, 0.000000000000000000, -1.000000000000000000 ) ) ;
#14445 = VECTOR ( 'NONE', #13213, 1000.000000000000000 ) ;
#14446 = DIRECTION ( 'NONE',  ( -0.9096319953545185522, 0.4154150130018859355, 0.000000000000000000 ) ) ;
#14447 = CARTESIAN_POINT ( 'NONE',  ( -34.55463468735881349, 14.62320705866887494, 37.50000000001273293 ) ) ;
#14448 = VERTEX_POINT ( 'NONE', #8470 ) ;
#14449 = CARTESIAN_POINT ( 'NONE',  ( -4.776122516674677878E-15, -42.50000000000000000, 1.500000000000000000 ) ) ;
#14450 = CARTESIAN_POINT ( 'NONE',  ( 33.41082347385297169, 9.568393510027430438, 36.00351576910800588 ) ) ;
#14451 = CARTESIAN_POINT ( 'NONE',  ( 12.04446003218043515, 42.09125592553625239, -16.50000000000000000 ) ) ;
#14452 = VERTEX_POINT ( 'NONE', #28086 ) ;
#14453 = CARTESIAN_POINT ( 'NONE',  ( 14.36006998371584054, 17.26937953831785677, 1.500000000000000000 ) ) ;
#14454 = DIRECTION ( 'NONE',  ( 0.000000000000000000, 0.000000000000000000, -1.000000000000000000 ) ) ;
#14455 = LINE ( 'NONE', #21621, #22751 ) ;
#14456 = CARTESIAN_POINT ( 'NONE',  ( 0.7836603915001320031, -17.02734626464551226, 5.652196082367002994 ) ) ;
#14457 = CARTESIAN_POINT ( 'NONE',  ( 0.000000000000000000, 0.000000000000000000, 1.500000000000000000 ) ) ;
#14458 = CARTESIAN_POINT ( 'NONE',  ( -37.99999999999999289, 90.00000000000001421, -81.50000000000000000 ) ) ;
#14459 = CARTESIAN_POINT ( 'NONE',  ( 36.97777267373784582, -13.52151540233721505, 9.972772046649604150 ) ) ;
#14460 = PLANE ( 'NONE',  #7400 ) ;
#14461 = ORIENTED_EDGE ( 'NONE', *, *, #18735, .T. ) ;
#14462 = DIRECTION ( 'NONE',  ( -0.000000000000000000, -0.000000000000000000, 1.000000000000000000 ) ) ;
#14463 = DIRECTION ( 'NONE',  ( -1.000000000000000000, 0.000000000000000000, 0.000000000000000000 ) ) ;
#14464 = ORIENTED_EDGE ( 'NONE', *, *, #18423, .F. ) ;
#14465 = VERTEX_POINT ( 'NONE', #17974 ) ;
#14466 = CARTESIAN_POINT ( 'NONE',  ( 5.169584817211992700, 19.32078214751397738, 20.34789198813115618 ) ) ;
#14467 = DIRECTION ( 'NONE',  ( 0.000000000000000000, 1.000000000000000000, 1.193512090021232842E-16 ) ) ;
#14468 =( NAMED_UNIT ( * ) SI_UNIT ( $, .STERADIAN. ) SOLID_ANGLE_UNIT ( ) );
#14469 = ORIENTED_EDGE ( 'NONE', *, *, #22137, .F. ) ;
#14470 = DIRECTION ( 'NONE',  ( 0.5406408174555974444, 0.8412535328311813165, 0.000000000000000000 ) ) ;
#14471 = ADVANCED_FACE ( 'NONE', ( #6102 ), #25130, .F. ) ;
#14472 = ORIENTED_EDGE ( 'NONE', *, *, #29614, .F. ) ;
#14473 = CARTESIAN_POINT ( 'NONE',  ( 18.63200854944940232, -7.318485330915432741, 18.64703902303423178 ) ) ;
#14474 = CARTESIAN_POINT ( 'NONE',  ( 16.71770988170261063, 3.349230485916621980, 18.35718225375110180 ) ) ;
#14475 = AXIS2_PLACEMENT_3D ( 'NONE', #5437, #8086, #21953 ) ;
#14476 = DIRECTION ( 'NONE',  ( -1.000000000000000000, 0.000000000000000000, 0.000000000000000000 ) ) ;
#14477 = VERTEX_POINT ( 'NONE', #27794 ) ;
#14478 = CARTESIAN_POINT ( 'NONE',  ( 28.34828976096172681, 29.18752572968383419, 1.500000000000000000 ) ) ;
#14479 = ORIENTED_EDGE ( 'NONE', *, *, #26181, .T. ) ;
#14480 = ORIENTED_EDGE ( 'NONE', *, *, #29747, .F. ) ;
#14481 = CARTESIAN_POINT ( 'NONE',  ( 31.29501345865701012, -26.27841684422097401, -6.499999999999999112 ) ) ;
#14482 = DIRECTION ( 'NONE',  ( 0.000000000000000000, 0.000000000000000000, -1.000000000000000000 ) ) ;
#14483 = DIRECTION ( 'NONE',  ( -0.9898214418809326842, -0.1423148382732852824, 0.000000000000000000 ) ) ;
#14484 = DIRECTION ( 'NONE',  ( -0.000000000000000000, -0.000000000000000000, -1.000000000000000000 ) ) ;
#14485 = CARTESIAN_POINT ( 'NONE',  ( -23.12946144662537051, 11.96621729904739517, 48.95860290871405596 ) ) ;
#14486 = CARTESIAN_POINT ( 'NONE',  ( -6.980328572437709767, 4.608906612435681005, 21.50000000000000000 ) ) ;
#14487 = ADVANCED_FACE ( 'NONE', ( #4073 ), #13603, .T. ) ;
#14488 = ORIENTED_EDGE ( 'NONE', *, *, #19693, .F. ) ;
#14489 = EDGE_CURVE ( 'NONE', #4417, #26711, #6864, .T. ) ;
#14490 = AXIS2_PLACEMENT_3D ( 'NONE', #26728, #27042, #13005 ) ;
#14491 = CARTESIAN_POINT ( 'NONE',  ( -19.71314312682348913, 3.479754436677866547, 19.11611934778430921 ) ) ;
#14492 = CARTESIAN_POINT ( 'NONE',  ( 18.32239734440382151, -8.062462575157594458, 5.653912893140659257 ) ) ;
#14493 = VECTOR ( 'NONE', #22857, 1000.000000000000000 ) ;
#14494 = CYLINDRICAL_SURFACE ( 'NONE', #14822, 0.7500000000000002220 ) ;
#14495 = DIRECTION ( 'NONE',  ( 0.000000000000000000, 0.000000000000000000, -1.000000000000000000 ) ) ;
#14496 = EDGE_CURVE ( 'NONE', #1222, #27986, #21506, .T. ) ;
#14497 = ORIENTED_EDGE ( 'NONE', *, *, #19128, .F. ) ;
#14498 =( BOUNDED_CURVE ( )  B_SPLINE_CURVE ( 3, ( #8477, #975, #22336, #17506 ),
 .UNSPECIFIED., .F., .T. ) 
 B_SPLINE_CURVE_WITH_KNOTS ( ( 4, 4 ),
 ( 3.141592653589793116, 6.283185307179586232 ),
 .UNSPECIFIED. ) 
 CURVE ( )  GEOMETRIC_REPRESENTATION_ITEM ( )  RATIONAL_B_SPLINE_CURVE ( ( 1.000000000000000000, 0.3333333333333333703, 0.3333333333333333703, 1.000000000000000000 ) ) 
 REPRESENTATION_ITEM ( '' )  );
#14499 = ORIENTED_EDGE ( 'NONE', *, *, #5602, .F. ) ;
#14500 = CARTESIAN_POINT ( 'NONE',  ( 39.87350638640861433, 4.706224724276823146, -11.49999999999999645 ) ) ;
#14501 = CARTESIAN_POINT ( 'NONE',  ( -37.16608720827707657, -51.86186943028246787, 97.07879600563551037 ) ) ;
#14502 = EDGE_CURVE ( 'NONE', #5698, #14945, #23687, .T. ) ;
#14503 = CARTESIAN_POINT ( 'NONE',  ( -40.05104235265675783, -2.353288714459718989, -11.49999999999999645 ) ) ;
#14504 = CARTESIAN_POINT ( 'NONE',  ( -5.475907499891252250, 16.13963752243574490, 18.34969686940295830 ) ) ;
#14505 = CARTESIAN_POINT ( 'NONE',  ( -2.959227181723746547, 8.499586724479465616, -1.500000000000000888 ) ) ;
#14506 = CARTESIAN_POINT ( 'NONE',  ( -31.59044894475038134, -19.10522403758187338, 27.50000000000000355 ) ) ;
#14507 = CARTESIAN_POINT ( 'NONE',  ( -5.001173922442003317, 19.36461358832317359, 6.518927109361842831 ) ) ;
#14508 = EDGE_CURVE ( 'NONE', #5466, #27986, #12166, .T. ) ;
#14509 = VERTEX_POINT ( 'NONE', #23540 ) ;
#14510 = CARTESIAN_POINT ( 'NONE',  ( -13.83774706505031560, -36.52929077895569066, 34.49999999999999289 ) ) ;
#14511 = ADVANCED_FACE ( 'NONE', ( #30569, #2333 ), #4527, .F. ) ;
#14512 = CARTESIAN_POINT ( 'NONE',  ( -17.98703099176682230, -8.745510052321845862, 20.34789198813115618 ) ) ;
#14513 = FACE_OUTER_BOUND ( 'NONE', #28409, .T. ) ;
#14514 = ORIENTED_EDGE ( 'NONE', *, *, #15087, .F. ) ;
#14515 = ADVANCED_FACE ( 'NONE', ( #14037 ), #7337, .F. ) ;
#14516 = CARTESIAN_POINT ( 'NONE',  ( 12.94832566568966037, 11.05145698499350004, 6.211014596808754007 ) ) ;
#14517 = ORIENTED_EDGE ( 'NONE', *, *, #9737, .F. ) ;
#14518 = FACE_OUTER_BOUND ( 'NONE', #23127, .T. ) ;
#14519 = UNCERTAINTY_MEASURE_WITH_UNIT (LENGTH_MEASURE( 1.000000000000000082E-05 ), #14066, 'distance_accuracy_value', 'NONE');
#14520 = CARTESIAN_POINT ( 'NONE',  ( -33.03787114093149313, 23.27353420009350415, -4.833239141675061745 ) ) ;
#14521 = DIRECTION ( 'NONE',  ( 0.9329908884337542174, -0.3598999890241650901, 0.000000000000000000 ) ) ;
#14522 = EDGE_LOOP ( 'NONE', ( #16996, #9191, #6467, #21058 ) ) ;
#14523 = CARTESIAN_POINT ( 'NONE',  ( 49.67347041229598403, 69.99755012469657345, 55.05519839654500203 ) ) ;
#14524 = CARTESIAN_POINT ( 'NONE',  ( -5.130938270761550513, 7.974144905643841597, 1.500000000000001332 ) ) ;
#14525 = DIRECTION ( 'NONE',  ( -0.06975647374412530244, 0.000000000000000000, 0.9975640502598241977 ) ) ;
#14526 = CARTESIAN_POINT ( 'NONE',  ( -18.40581374043506457, -7.824871006739531509, 6.144783687052511212 ) ) ;
#14527 = CARTESIAN_POINT ( 'NONE',  ( -10.73477556097085461, -16.87541441043898516, 5.676722608126685721 ) ) ;
#14528 = CARTESIAN_POINT ( 'NONE',  ( 33.42925964089141644, -11.06161099612213228, 39.78814634291933316 ) ) ;
#14529 = EDGE_CURVE ( 'NONE', #23663, #17274, #29070, .T. ) ;
#14530 = ORIENTED_EDGE ( 'NONE', *, *, #23339, .T. ) ;
#14531 = ADVANCED_FACE ( 'NONE', ( #14182 ), #4989, .F. ) ;
#14532 = CARTESIAN_POINT ( 'NONE',  ( 0.000000000000000000, 0.000000000000000000, -1.500000000000000000 ) ) ;
#14533 = EDGE_CURVE ( 'NONE', #17860, #17738, #3678, .T. ) ;
#14534 = CARTESIAN_POINT ( 'NONE',  ( -31.18700685316100163, -26.11823559932341610, -1.500000000000000000 ) ) ;
#14535 = DIRECTION ( 'NONE',  ( 0.000000000000000000, 0.000000000000000000, -1.000000000000000000 ) ) ;
#14536 = EDGE_CURVE ( 'NONE', #28753, #16453, #2009, .T. ) ;
#14537 = VERTEX_POINT ( 'NONE', #18884 ) ;
#14538 = DIRECTION ( 'NONE',  ( 0.000000000000000000, 0.000000000000000000, -1.000000000000000000 ) ) ;
#14539 = CARTESIAN_POINT ( 'NONE',  ( -17.67332396526446914, -9.400239829055450969, 19.89182036555910571 ) ) ;
#14540 = DIRECTION ( 'NONE',  ( -0.000000000000000000, -0.000000000000000000, 1.000000000000000000 ) ) ;
#14541 = ADVANCED_FACE ( 'NONE', ( #21047 ), #25896, .F. ) ;
#14542 = FILL_AREA_STYLE_COLOUR ( '', #3321 ) ;
#14543 = AXIS2_PLACEMENT_3D ( 'NONE', #21680, #21999, #12504 ) ;
#14544 = CARTESIAN_POINT ( 'NONE',  ( -10.11202017158466759, 41.14070756921185534, -1.500000000000000000 ) ) ;
#14545 = VERTEX_POINT ( 'NONE', #30858 ) ;
#14546 = EDGE_CURVE ( 'NONE', #3669, #21410, #4679, .T. ) ;
#14547 = DIRECTION ( 'NONE',  ( 0.000000000000000000, 0.000000000000000000, 1.000000000000000000 ) ) ;
#14548 = CARTESIAN_POINT ( 'NONE',  ( 36.66051849534079565, 8.298796628992828772, 37.50000000001189449 ) ) ;
#14549 = EDGE_CURVE ( 'NONE', #7038, #23836, #13175, .T. ) ;
#14550 = DIRECTION ( 'NONE',  ( 0.000000000000000000, 1.132880637372608986E-16, -1.000000000000000000 ) ) ;
#14551 = ORIENTED_EDGE ( 'NONE', *, *, #24795, .T. ) ;
#14552 = DIRECTION ( 'NONE',  ( 0.000000000000000000, 0.000000000000000000, 1.000000000000000000 ) ) ;
#14553 = ORIENTED_EDGE ( 'NONE', *, *, #5364, .F. ) ;
#14554 = LINE ( 'NONE', #24050, #27669 ) ;
#14555 = FACE_OUTER_BOUND ( 'NONE', #9498, .T. ) ;
#14556 = ORIENTED_EDGE ( 'NONE', *, *, #3915, .F. ) ;
#14557 = ORIENTED_EDGE ( 'NONE', *, *, #14318, .T. ) ;
#14558 = DIRECTION ( 'NONE',  ( 0.000000000000000000, 0.000000000000000000, 1.000000000000000000 ) ) ;
#14559 = ORIENTED_EDGE ( 'NONE', *, *, #23783, .T. ) ;
#14560 = ORIENTED_EDGE ( 'NONE', *, *, #9154, .T. ) ;
#14561 = VERTEX_POINT ( 'NONE', #2804 ) ;
#14562 = CARTESIAN_POINT ( 'NONE',  ( 0.01267125088587655463, -20.01782649599895336, 20.29090034784956131 ) ) ;
#14563 = ADVANCED_FACE ( 'NONE', ( #22285 ), #17690, .F. ) ;
#14564 = CARTESIAN_POINT ( 'NONE',  ( 4.510281037539698445E-13, -4.926614671774132148E-13, 65.49999999999998579 ) ) ;
#14565 = CARTESIAN_POINT ( 'NONE',  ( -9.785592877189483119, -17.46290528139147469, 7.196036389296800451 ) ) ;
#14566 = EDGE_CURVE ( 'NONE', #540, #26699, #22441, .T. ) ;
#14567 = CARTESIAN_POINT ( 'NONE',  ( 4.989870534563210391, 16.27408959345712347, 19.08155846658118904 ) ) ;
#14568 = EDGE_LOOP ( 'NONE', ( #10997, #2389, #20224 ) ) ;
#14569 = DIRECTION ( 'NONE',  ( -1.000000000000000000, 0.000000000000000000, 0.000000000000000000 ) ) ;
#14570 = DIRECTION ( 'NONE',  ( -1.000000000000000000, 0.000000000000000000, 0.000000000000000000 ) ) ;
#14571 = CARTESIAN_POINT ( 'NONE',  ( 0.8583496426666220591, -19.98194197654537874, 20.22386025856689429 ) ) ;
#14572 = FACE_OUTER_BOUND ( 'NONE', #18465, .T. ) ;
#14573 = ORIENTED_EDGE ( 'NONE', *, *, #4389, .F. ) ;
#14574 = CARTESIAN_POINT ( 'NONE',  ( 25.10445388623454477, 25.60065097860747585, -1.500000000000000000 ) ) ;
#14575 = CARTESIAN_POINT ( 'NONE',  ( -14.77047757180930176, -8.563270617688839792, 6.131018562779544823 ) ) ;
#14576 = APPLICATION_CONTEXT ( 'automotive_design' ) ;
#14577 = DIRECTION ( 'NONE',  ( 0.6548607339452855447, 0.7557495743542579358, 0.000000000000000000 ) ) ;
#14578 = CIRCLE ( 'NONE', #4663, 0.7499999999999997780 ) ;
#14579 = AXIS2_PLACEMENT_3D ( 'NONE', #17801, #27315, #30104 ) ;
#14580 = FACE_OUTER_BOUND ( 'NONE', #10173, .T. ) ;
#14581 = CARTESIAN_POINT ( 'NONE',  ( 0.8038475772933620922, 5.196152422706624030, 9.000000000000001776 ) ) ;
#14582 = CARTESIAN_POINT ( 'NONE',  ( -15.25992540518562279, -7.581593484474005606, 18.36582235739946611 ) ) ;
#14583 = DIRECTION ( 'NONE',  ( 0.000000000000000000, 0.000000000000000000, -1.000000000000000000 ) ) ;
#14584 = EDGE_LOOP ( 'NONE', ( #7225, #26900, #2267, #689, #5584 ) ) ;
#14585 = ORIENTED_EDGE ( 'NONE', *, *, #12994, .T. ) ;
#14586 = SURFACE_SIDE_STYLE ('',( #12242 ) ) ;
#14587 = CARTESIAN_POINT ( 'NONE',  ( -5.723804255145591213, 19.16384832744316213, 18.37250658438899009 ) ) ;
#14588 = CARTESIAN_POINT ( 'NONE',  ( -13.09005700315871579, 10.89973235955167929, 7.557577766377196582 ) ) ;
#14589 = CARTESIAN_POINT ( 'NONE',  ( -24.03057240117690441, -26.57182937991348481, 26.54355021145562787 ) ) ;
#14590 = ORIENTED_EDGE ( 'NONE', *, *, #4057, .F. ) ;
#14591 = CARTESIAN_POINT ( 'NONE',  ( 16.01701959592644897, -5.879758784403577465, 20.24143955528809258 ) ) ;
#14592 = DIRECTION ( 'NONE',  ( 0.000000000000000000, 0.000000000000000000, -1.000000000000000000 ) ) ;
#14593 = ORIENTED_EDGE ( 'NONE', *, *, #17979, .F. ) ;
#14594 = CARTESIAN_POINT ( 'NONE',  ( 4.744089322959553101, 16.35312844164164048, 20.05479082170252525 ) ) ;
#14595 = CARTESIAN_POINT ( 'NONE',  ( 14.74830145734718734, 13.53506178006322713, 7.627891251804737927 ) ) ;
#14596 = CARTESIAN_POINT ( 'NONE',  ( 8.884323311075775109, 1.438332125858202692, -3.621320343559650379 ) ) ;
#14597 = CARTESIAN_POINT ( 'NONE',  ( -18.39976944410068072, 37.47990255558614336, 29.29674481779093043 ) ) ;
#14598 = ORIENTED_EDGE ( 'NONE', *, *, #21059, .F. ) ;
#14599 = FACE_OUTER_BOUND ( 'NONE', #21521, .T. ) ;
#14600 = VECTOR ( 'NONE', #10657, 1000.000000000000000 ) ;
#14601 = EDGE_CURVE ( 'NONE', #14763, #7727, #14804, .T. ) ;
#14602 = AXIS2_PLACEMENT_3D ( 'NONE', #22974, #13022, #1313 ) ;
#14603 = CARTESIAN_POINT ( 'NONE',  ( 33.03707461445869598, 8.975870916883787132, 36.52286458921579992 ) ) ;
#14604 = LINE ( 'NONE', #5404, #23774 ) ;
#14605 = ORIENTED_EDGE ( 'NONE', *, *, #7875, .F. ) ;
#14606 = FACE_OUTER_BOUND ( 'NONE', #11083, .T. ) ;
#14607 = DIRECTION ( 'NONE',  ( 1.000000000000000000, 0.000000000000000000, 0.000000000000000000 ) ) ;
#14609 = CARTESIAN_POINT ( 'NONE',  ( 14.88222593340885958, 13.36111339922579155, 7.652108011868850035 ) ) ;
#14608 = VECTOR ( 'NONE', #23585, 1000.000000000000114 ) ;
#14610 = DIRECTION ( 'NONE',  ( -1.000000000000000000, 0.000000000000000000, 0.000000000000000000 ) ) ;
#14611 = CARTESIAN_POINT ( 'NONE',  ( -77.99999999999998579, -42.49999999999998579, 27.50000000000000711 ) ) ;
#14612 = CARTESIAN_POINT ( 'NONE',  ( 4.510281037539698445E-13, -4.926614671774132148E-13, 82.49999999999998579 ) ) ;
#14613 = CARTESIAN_POINT ( 'NONE',  ( -1.897971151300065476E-14, 75.00000000000001421, 22.49999999999999289 ) ) ;
#14614 = FACE_BOUND ( 'NONE', #24850, .T. ) ;
#14615 = ORIENTED_EDGE ( 'NONE', *, *, #265, .T. ) ;
#14616 = CARTESIAN_POINT ( 'NONE',  ( -4.163336342344337027E-14, 1.387778780781445676E-14, 24.50000000000000000 ) ) ;
#14617 = AXIS2_PLACEMENT_3D ( 'NONE', #3331, #24689, #10195 ) ;
#14618 = FACE_OUTER_BOUND ( 'NONE', #26828, .T. ) ;
#14619 = VERTEX_POINT ( 'NONE', #24783 ) ;
#14620 = EDGE_LOOP ( 'NONE', ( #22438, #20944, #28134, #4208 ) ) ;
#14621 = VECTOR ( 'NONE', #7493, 1000.000000000000000 ) ;
#14622 = CARTESIAN_POINT ( 'NONE',  ( -19.64177907938615064, 36.71644397333972876, 24.50000000000000000 ) ) ;
#14623 = CARTESIAN_POINT ( 'NONE',  ( -11.28151912705817672, 48.71169459815545366, -64.89780961319154073 ) ) ;
#14624 = AXIS2_PLACEMENT_3D ( 'NONE', #15773, #17658, #24667 ) ;
#14625 = SHAPE_REPRESENTATION_RELATIONSHIP ( 'NONE' , 'NONE' ,  #16871, #8388 ) ;
#14626 = ORIENTED_EDGE ( 'NONE', *, *, #28513, .T. ) ;
#14627 = DIRECTION ( 'NONE',  ( 0.000000000000000000, -1.132880637372608986E-16, 1.000000000000000000 ) ) ;
#14628 = CARTESIAN_POINT ( 'NONE',  ( -28.34828976096172681, -29.18752572968383419, 1.500000000000000000 ) ) ;
#14629 = VERTEX_POINT ( 'NONE', #29003 ) ;
#14630 = DIRECTION ( 'NONE',  ( 0.9594929736144951482, -0.2817325568414371095, 0.000000000000000000 ) ) ;
#14631 = CARTESIAN_POINT ( 'NONE',  ( 16.66634534075877028, 3.639270104310703857, 18.44527579819791185 ) ) ;
#14632 = DIRECTION ( 'NONE',  ( 0.000000000000000000, -1.132880637372608986E-16, 1.000000000000000000 ) ) ;
#14633 = ORIENTED_EDGE ( 'NONE', *, *, #4748, .T. ) ;
#14634 = CARTESIAN_POINT ( 'NONE',  ( 23.11524226670866611, -11.10088790631999345, 45.11515778357083661 ) ) ;
#14635 = VERTEX_POINT ( 'NONE', #14652 ) ;
#14636 = VECTOR ( 'NONE', #17267, 1000.000000000000000 ) ;
#14637 = AXIS2_PLACEMENT_3D ( 'NONE', #20723, #15751, #25271 ) ;
#14638 = CARTESIAN_POINT ( 'NONE',  ( 32.19782014694308003, -14.25394737442115201, 39.78814634291934738 ) ) ;
#14639 = CARTESIAN_POINT ( 'NONE',  ( -6.495433978329089086, 18.93455902173412397, 18.50655187082627862 ) ) ;
#14640 = CARTESIAN_POINT ( 'NONE',  ( -17.81964242321468816, -9.081580984160151360, 7.528076282304601463 ) ) ;
#14641 = CARTESIAN_POINT ( 'NONE',  ( -8.353478261420260509, -14.86569112999328368, 18.37415474056476938 ) ) ;
#14642 = FACE_OUTER_BOUND ( 'NONE', #12695, .T. ) ;
#14643 = CARTESIAN_POINT ( 'NONE',  ( 4.510281037539698445E-13, -4.926614671774132148E-13, 82.49999999999998579 ) ) ;
#14644 = DIRECTION ( 'NONE',  ( -1.000000000000000000, 0.000000000000000000, 0.000000000000000000 ) ) ;
#14645 = ORIENTED_EDGE ( 'NONE', *, *, #25056, .F. ) ;
#14646 = CARTESIAN_POINT ( 'NONE',  ( 9.195964344571802229, -14.32884674914071965, 6.018569869498933578 ) ) ;
#14647 = CARTESIAN_POINT ( 'NONE',  ( -32.53212664356424710, 23.45839305882638470, 8.000000000000005329 ) ) ;
#14648 = CARTESIAN_POINT ( 'NONE',  ( 2.352830851074111163, 9.185733585337919394, 1.500000000000001332 ) ) ;
#14649 = VERTEX_POINT ( 'NONE', #14962 ) ;
#14650 = ORIENTED_EDGE ( 'NONE', *, *, #1608, .T. ) ;
#14651 = DIRECTION ( 'NONE',  ( -0.8910248307962438385, 0.4539545692076743522, 0.000000000000000000 ) ) ;
#14652 = CARTESIAN_POINT ( 'NONE',  ( 37.99999999999999289, 90.00000000000001421, -81.50000000000001421 ) ) ;
#14653 = FACE_OUTER_BOUND ( 'NONE', #25572, .T. ) ;
#14654 = PLANE ( 'NONE',  #17611 ) ;
#14655 = AXIS2_PLACEMENT_3D ( 'NONE', #17623, #19798, #14966 ) ;
#14656 = CARTESIAN_POINT ( 'NONE',  ( 2.810445847081854964, 9.056208293496318618, 13.00000000000000178 ) ) ;
#14657 = EDGE_LOOP ( 'NONE', ( #10970, #5288 ) ) ;
#14658 = ORIENTED_EDGE ( 'NONE', *, *, #14166, .T. ) ;
#14659 = CARTESIAN_POINT ( 'NONE',  ( -29.01070392382221286, -23.40766234503086807, 34.49999999999998579 ) ) ;
#14660 = DIRECTION ( 'NONE',  ( 1.000000000000000000, 0.000000000000000000, 0.000000000000000000 ) ) ;
#14661 = EDGE_CURVE ( 'NONE', #20812, #28337, #12638, .T. ) ;
#14662 = EDGE_LOOP ( 'NONE', ( #1492, #30095, #23743 ) ) ;
#14663 = CARTESIAN_POINT ( 'NONE',  ( 15.53792925084563059, 12.62098510012954478, 6.864725433338323413 ) ) ;
#14664 = VERTEX_POINT ( 'NONE', #29478 ) ;
#14665 = PRODUCT_DEFINITION ( 'UNKNOWN', '', #935, #18249 ) ;
#14666 = DIRECTION ( 'NONE',  ( -1.000000000000000000, 0.000000000000000000, 0.000000000000000000 ) ) ;
#14667 = CARTESIAN_POINT ( 'NONE',  ( 16.74328841314636662, 3.194145055459935545, 20.34789198813115263 ) ) ;
#14668 = DIRECTION ( 'NONE',  ( 1.000000000000000000, 0.000000000000000000, 0.000000000000000000 ) ) ;
#14669 = VERTEX_POINT ( 'NONE', #3424 ) ;
#14670 = CARTESIAN_POINT ( 'NONE',  ( 49.48768812108095005, 69.99365322046264737, 55.67629387500135607 ) ) ;
#14671 = ADVANCED_FACE ( 'NONE', ( #1085 ), #10599, .T. ) ;
#14672 = CARTESIAN_POINT ( 'NONE',  ( 33.56327786402390245, 10.34181101807379655, -16.55003854064094426 ) ) ;
#14673 = CARTESIAN_POINT ( 'NONE',  ( -18.37726663805288041, -7.892083924814681239, 7.267242832833947119 ) ) ;
#14674 = AXIS2_PLACEMENT_3D ( 'NONE', #3200, #9913, #24406 ) ;
#14675 = CARTESIAN_POINT ( 'NONE',  ( 10.74273727477993567, -16.89139546617318999, 20.25336174263950184 ) ) ;
#14676 = LINE ( 'NONE', #15138, #15860 ) ;
#14677 = ORIENTED_EDGE ( 'NONE', *, *, #13983, .T. ) ;
#14678 = LINE ( 'NONE', #5326, #24254 ) ;
#14679 = EDGE_CURVE ( 'NONE', #681, #8511, #929, .T. ) ;
#14680 = CARTESIAN_POINT ( 'NONE',  ( 2.687479362164894248, -44.39187623478217404, -19.50000000000000355 ) ) ;
#14681 = DIRECTION ( 'NONE',  ( 0.000000000000000000, 0.000000000000000000, -1.000000000000000000 ) ) ;
#14682 = ORIENTED_EDGE ( 'NONE', *, *, #29747, .T. ) ;
#14683 = EDGE_CURVE ( 'NONE', #9984, #19691, #22091, .T. ) ;
#14684 = CARTESIAN_POINT ( 'NONE',  ( -15.06839649859470853, -7.981447355247936137, 20.32367522806703874 ) ) ;
#14685 = CARTESIAN_POINT ( 'NONE',  ( 15.43499236066653779, -3.229500095980124996, 24.50000000000000000 ) ) ;
#14686 = CARTESIAN_POINT ( 'NONE',  ( -14.81308450742032434, 13.43805957489523095, 19.96302680909624527 ) ) ;
#14687 = CARTESIAN_POINT ( 'NONE',  ( 4.533306948338779563, 16.41820958405255837, 5.774779864094946369 ) ) ;
#14688 = CARTESIAN_POINT ( 'NONE',  ( 2.687479362164894248, -44.39187623478217404, -19.50000000000000355 ) ) ;
#14689 = DIRECTION ( 'NONE',  ( 1.000000000000000000, 0.000000000000000000, 0.000000000000000000 ) ) ;
#14690 = CARTESIAN_POINT ( 'NONE',  ( 38.70786393739909670, 5.827369745586353567, 35.04830057171592728 ) ) ;
#14691 = CARTESIAN_POINT ( 'NONE',  ( 19.69983030747900443, 3.454193845114027273, 7.626218077512941562 ) ) ;
#14692 = EDGE_LOOP ( 'NONE', ( #11058, #629, #20195, #11934 ) ) ;
#14693 = CARTESIAN_POINT ( 'NONE',  ( -37.16608720827707657, -36.86186943028246787, 12.49999999999999112 ) ) ;
#14694 = ORIENTED_EDGE ( 'NONE', *, *, #8648, .F. ) ;
#14695 = DIRECTION ( 'NONE',  ( 1.000000000000000000, 0.000000000000000000, 0.000000000000000000 ) ) ;
#14696 = CARTESIAN_POINT ( 'NONE',  ( 4.668110441710642711, -19.44758969394385062, 24.50000000000000000 ) ) ;
#14697 = ORIENTED_EDGE ( 'NONE', *, *, #26732, .F. ) ;
#14698 = AXIS2_PLACEMENT_3D ( 'NONE', #12176, #26206, #24330 ) ;
#14699 = EDGE_CURVE ( 'NONE', #23537, #20897, #7657, .T. ) ;
#14700 = ORIENTED_EDGE ( 'NONE', *, *, #21059, .T. ) ;
#14701 = EDGE_CURVE ( 'NONE', #15766, #6758, #8668, .T. ) ;
#14702 = LINE ( 'NONE', #2859, #319 ) ;
#14703 = ORIENTED_EDGE ( 'NONE', *, *, #25213, .F. ) ;
#14704 = VERTEX_POINT ( 'NONE', #10445 ) ;
#14705 = CARTESIAN_POINT ( 'NONE',  ( -0.5567245496722531550, -20.01015347392404209, 18.90679857307105749 ) ) ;
#14706 = LINE ( 'NONE', #29218, #19267 ) ;
#14707 = EDGE_CURVE ( 'NONE', #27782, #18935, #19521, .T. ) ;
#14708 = CYLINDRICAL_SURFACE ( 'NONE', #7013, 20.00000000000000000 ) ;
#14709 = CARTESIAN_POINT ( 'NONE',  ( 40.05520465696179855, -7.028746455191999587, -16.50000000000000000 ) ) ;
#14710 = CARTESIAN_POINT ( 'NONE',  ( -21.90865045291187485, 23.69204963285887899, -16.50001200000000523 ) ) ;
#14711 = VERTEX_POINT ( 'NONE', #1694 ) ;
#14712 = EDGE_CURVE ( 'NONE', #30406, #20533, #6165, .T. ) ;
#14713 = CARTESIAN_POINT ( 'NONE',  ( -50.00000000000000000, -50.00000000000000000, 62.49999999999999289 ) ) ;
#14714 = CARTESIAN_POINT ( 'NONE',  ( 4.186421491866439304, -43.85598367614507964, -16.50000000000000000 ) ) ;
#14715 = CARTESIAN_POINT ( 'NONE',  ( 11.69519594420020248, 12.44297266173654748, 19.03762469184452755 ) ) ;
#14716 = CARTESIAN_POINT ( 'NONE',  ( 6.587096388939653657, -18.88412458026098406, 24.50000000000000000 ) ) ;
#14717 = EDGE_CURVE ( 'NONE', #5725, #28626, #2169, .T. ) ;
#14718 = VERTEX_POINT ( 'NONE', #20261 ) ;
#14719 = DIRECTION ( 'NONE',  ( 1.000000000000000000, 0.000000000000000000, 0.000000000000000000 ) ) ;
#14720 = CARTESIAN_POINT ( 'NONE',  ( -17.77309463542032830, -9.210542792609436091, 5.872146474157316831 ) ) ;
#14721 = CARTESIAN_POINT ( 'NONE',  ( -6.922783288613180375, 18.78247243576999992, 6.447548852708279377 ) ) ;
#14722 = ADVANCED_FACE ( 'NONE', ( #13420 ), #15900, .F. ) ;
#14723 = CARTESIAN_POINT ( 'NONE',  ( 38.00000000000000711, 90.00000000000001421, -87.50000000000000000 ) ) ;
#14724 = CARTESIAN_POINT ( 'NONE',  ( -23.26375789455195786, 12.37328455203049771, 44.40817556379787590 ) ) ;
#14725 = VECTOR ( 'NONE', #3587, 1000.000000000000000 ) ;
#14726 = ORIENTED_EDGE ( 'NONE', *, *, #9932, .T. ) ;
#14727 = ORIENTED_EDGE ( 'NONE', *, *, #23113, .F. ) ;
#14728 = CARTESIAN_POINT ( 'NONE',  ( -5.849168665050582305, 19.12602664087013693, 18.34726407865098707 ) ) ;
#14729 = CARTESIAN_POINT ( 'NONE',  ( 35.00000000000000000, 70.00000000000000000, -22.50000000000003908 ) ) ;
#14730 = LINE ( 'NONE', #12247, #20605 ) ;
#14731 = VERTEX_POINT ( 'NONE', #20706 ) ;
#14732 = CARTESIAN_POINT ( 'NONE',  ( 19.91398265452213678, -1.852915226174634444, 24.50000000000000000 ) ) ;
#14733 = CIRCLE ( 'NONE', #22194, 0.7441270634457163302 ) ;
#14734 = CARTESIAN_POINT ( 'NONE',  ( -50.00000000000000000, 90.00000000000001421, 12.49999999999999112 ) ) ;
#14735 = EDGE_CURVE ( 'NONE', #18935, #15666, #4184, .T. ) ;
#14736 = ORIENTED_EDGE ( 'NONE', *, *, #3490, .F. ) ;
#14737 = EDGE_CURVE ( 'NONE', #20938, #4388, #5153, .T. ) ;
#14738 = DIRECTION ( 'NONE',  ( 1.000000000000000000, 0.000000000000000000, 0.000000000000000000 ) ) ;
#14739 = CARTESIAN_POINT ( 'NONE',  ( -8.097046320276927389, -15.01856385377392478, 18.45571264222804686 ) ) ;
#14740 = EDGE_CURVE ( 'NONE', #16110, #14537, #28558, .T. ) ;
#14741 = CARTESIAN_POINT ( 'NONE',  ( -37.58583663907551653, -0.5225704585679834535, 37.50000000000396483 ) ) ;
#14742 = ORIENTED_EDGE ( 'NONE', *, *, #6192, .F. ) ;
#14743 = CARTESIAN_POINT ( 'NONE',  ( -70.00000000000000000, -70.00000000000000000, 12.49999999999999112 ) ) ;
#14744 = CIRCLE ( 'NONE', #288, 0.6002263538043648428 ) ;
#14745 = CARTESIAN_POINT ( 'NONE',  ( 33.55239377822428537, 10.10392708029668363, 35.71678343307738146 ) ) ;
#14746 = FACE_BOUND ( 'NONE', #10568, .T. ) ;
#14747 = EDGE_LOOP ( 'NONE', ( #9845, #14020, #13557, #16355 ) ) ;
#14748 = CARTESIAN_POINT ( 'NONE',  ( -10.51513057463694523, -17.01270198993485394, 20.34789198813115263 ) ) ;
#14749 = DIRECTION ( 'NONE',  ( -0.000000000000000000, -0.000000000000000000, -1.000000000000000000 ) ) ;
#14750 = FACE_BOUND ( 'NONE', #12180, .T. ) ;
#14751 = B_SPLINE_CURVE_WITH_KNOTS ( 'NONE', 3,
 ( #9390, #12039, #21534, #18747, #169 ),
 .UNSPECIFIED., .F., .F.,
 ( 4, 1, 4 ),
 ( 0.8465381644365373992, 0.8518173996194324804, 0.8570966348023274506 ),
 .UNSPECIFIED. ) ;
#14752 = DIRECTION ( 'NONE',  ( -1.000000000000000000, -0.000000000000000000, -0.000000000000000000 ) ) ;
#14753 = AXIS2_PLACEMENT_3D ( 'NONE', #7445, #16949, #17256 ) ;
#14754 = CARTESIAN_POINT ( 'NONE',  ( -77.99999999999998579, 42.50000000000000000, 27.50000000000000711 ) ) ;
#14755 = CARTESIAN_POINT ( 'NONE',  ( -10.51100353655187369, -17.01524272303503693, 18.34798005863227388 ) ) ;
#14756 = CARTESIAN_POINT ( 'NONE',  ( 37.41913830146530273, -11.98133940937022146, 15.32185239508652863 ) ) ;
#14757 =( GEOMETRIC_REPRESENTATION_CONTEXT ( 3 ) GLOBAL_UNCERTAINTY_ASSIGNED_CONTEXT ( ( #14198 ) ) GLOBAL_UNIT_ASSIGNED_CONTEXT ( ( #29664, #27485, #22631 ) ) REPRESENTATION_CONTEXT ( 'NONE', 'WORKASPACE' ) );
#14758 = CYLINDRICAL_SURFACE ( 'NONE', #14869, 0.7441270634457163302 ) ;
#14759 = VERTEX_POINT ( 'NONE', #15419 ) ;
#14760 = CARTESIAN_POINT ( 'NONE',  ( -5.796781398520591821, 16.03935303270742807, 7.652108011868850035 ) ) ;
#14761 = CARTESIAN_POINT ( 'NONE',  ( 4.695984468547711899, 19.44110619659980088, 7.454606537396347932 ) ) ;
#14762 = ORIENTED_EDGE ( 'NONE', *, *, #21005, .T. ) ;
#14763 = VERTEX_POINT ( 'NONE', #30085 ) ;
#14764 = AXIS2_PLACEMENT_3D ( 'NONE', #26472, #29120, #7757 ) ;
#14765 = CARTESIAN_POINT ( 'NONE',  ( -8.832778568892177162, 41.43887595177744032, 20.59886053955145613 ) ) ;
#14766 = EDGE_CURVE ( 'NONE', #1105, #22982, #18405, .T. ) ;
#14767 = CARTESIAN_POINT ( 'NONE',  ( -38.00000000000000000, 80.00000000000000000, -7.533656238527846826E-15 ) ) ;
#14768 = AXIS2_PLACEMENT_3D ( 'NONE', #17420, #29894, #24897 ) ;
#14769 =( LENGTH_UNIT ( ) NAMED_UNIT ( * ) SI_UNIT ( .MILLI., .METRE. ) );
#14770 = EDGE_LOOP ( 'NONE', ( #49, #18684, #25405, #1687 ) ) ;
#14771 = EDGE_CURVE ( 'NONE', #25239, #15430, #6534, .T. ) ;
#14772 = AXIS2_PLACEMENT_3D ( 'NONE', #26552, #2375, #21397 ) ;
#14773 = CARTESIAN_POINT ( 'NONE',  ( 12.97958999564962035, 11.01328844340110713, 19.00652017443069752 ) ) ;
#14774 = CARTESIAN_POINT ( 'NONE',  ( -10.80882669148404673, -16.84912922860908679, 5.701226463332907279 ) ) ;
#14775 = EDGE_LOOP ( 'NONE', ( #15277, #6924, #20671, #13369 ) ) ;
#14776 = CARTESIAN_POINT ( 'NONE',  ( 18.52707432543149579, -7.580618987226257488, 18.44527579819791185 ) ) ;
#14777 = B_SPLINE_CURVE_WITH_KNOTS ( 'NONE', 3,
 ( #26428, #5057, #16745, #7233, #5211, #26108, #28611 ),
 .UNSPECIFIED., .F., .F.,
 ( 4, 3, 4 ),
 ( 0.000000000000000000, 0.005031266826504186655, 0.01006253384358471795 ),
 .UNSPECIFIED. ) ;
#14778 = CARTESIAN_POINT ( 'NONE',  ( 16.70510464924393901, 3.421819763545495441, 18.37415474056476938 ) ) ;
#14779 = AXIS2_PLACEMENT_3D ( 'NONE', #18499, #11475, #28000 ) ;
#14780 = PLANE ( 'NONE',  #6997 ) ;
#14781 = VERTEX_POINT ( 'NONE', #15730 ) ;
#14782 = CARTESIAN_POINT ( 'NONE',  ( 23.11727550875142612, -11.99039815441031465, 44.71664046407185822 ) ) ;
#14783 = ORIENTED_EDGE ( 'NONE', *, *, #4804, .F. ) ;
#14784 = AXIS2_PLACEMENT_3D ( 'NONE', #18296, #7042, #11890 ) ;
#14785 = ORIENTED_EDGE ( 'NONE', *, *, #11460, .F. ) ;
#14786 = CIRCLE ( 'NONE', #10817, 0.7499999999999997780 ) ;
#14787 = CIRCLE ( 'NONE', #18786, 17.00000000000000000 ) ;
#14788 = DIRECTION ( 'NONE',  ( 1.000000000000000000, 0.000000000000000000, 0.000000000000000000 ) ) ;
#14789 = CARTESIAN_POINT ( 'NONE',  ( -6.855891330591547650, 18.80700764124136626, 18.92976555901915603 ) ) ;
#14790 = CARTESIAN_POINT ( 'NONE',  ( -12.71124774491287646, 11.32026698792773978, 19.45164628100866722 ) ) ;
#14791 = CARTESIAN_POINT ( 'NONE',  ( -9.692246323650998363, -17.51472466453637367, 19.03762469184452755 ) ) ;
#14792 = CARTESIAN_POINT ( 'NONE',  ( -3.914781618004754105, -8.197313248159934673, 21.50000000000000000 ) ) ;
#14793 = CARTESIAN_POINT ( 'NONE',  ( 22.58267429318971864, 26.57182937991349903, 1.500000000000000000 ) ) ;
#14794 = FACE_OUTER_BOUND ( 'NONE', #3770, .T. ) ;
#14795 = EDGE_LOOP ( 'NONE', ( #16165, #13133, #2463, #30250 ) ) ;
#14796 = CARTESIAN_POINT ( 'NONE',  ( 9.496768069075223195, -14.14083042221133724, 5.749228751562096562 ) ) ;
#14797 = VECTOR ( 'NONE', #640, 1000.000000000000000 ) ;
#14798 = CARTESIAN_POINT ( 'NONE',  ( -50.00000000000000000, -50.00000000000000000, 52.07879600563550326 ) ) ;
#14799 = AXIS2_PLACEMENT_3D ( 'NONE', #7204, #28575, #7370 ) ;
#14800 = FACE_BOUND ( 'NONE', #19955, .T. ) ;
#14801 = EDGE_LOOP ( 'NONE', ( #28343, #21446, #18407, #16189, #30212, #2566, #12645, #16294, #11437 ) ) ;
#14802 = ORIENTED_EDGE ( 'NONE', *, *, #13503, .T. ) ;
#14803 = DIRECTION ( 'NONE',  ( -0.000000000000000000, -0.000000000000000000, -1.000000000000000000 ) ) ;
#14804 = LINE ( 'NONE', #21828, #18126 ) ;
#14805 = B_SPLINE_CURVE_WITH_KNOTS ( 'NONE', 3,
 ( #1307, #29865, #4712, #13927 ),
 .UNSPECIFIED., .F., .F.,
 ( 4, 4 ),
 ( 2.143643656977390230E-07, 0.003421830178490235883 ),
 .UNSPECIFIED. ) ;
#14806 = CARTESIAN_POINT ( 'NONE',  ( 37.99999999999933920, 0.000000000000000000, 85.49999999999998579 ) ) ;
#14807 = CARTESIAN_POINT ( 'NONE',  ( -15.42380629409197645, -7.219239307320219901, 7.453286057244485008 ) ) ;
#14808 = CIRCLE ( 'NONE', #25769, 27.70876437800068359 ) ;
#14809 = ADVANCED_FACE ( 'NONE', ( #6385 ), #25248, .F. ) ;
#14810 = DIRECTION ( 'NONE',  ( 1.000000000000000000, 0.000000000000000000, 0.000000000000000000 ) ) ;
#14811 = VECTOR ( 'NONE', #23177, 1000.000000000000000 ) ;
#14812 = CARTESIAN_POINT ( 'NONE',  ( 5.889883548616666964, 19.11329876149442697, 7.454139397117727661 ) ) ;
#14813 = ORIENTED_EDGE ( 'NONE', *, *, #4473, .F. ) ;
#14814 = CARTESIAN_POINT ( 'NONE',  ( -8.999114229549592281, 0.1262659238205133538, -1.500000000000001776 ) ) ;
#14815 = CARTESIAN_POINT ( 'NONE',  ( 9.824744466605370263, -8.513189541288715745, 1.500000000000001332 ) ) ;
#14816 = CARTESIAN_POINT ( 'NONE',  ( 57.49999999999998579, -50.00000000000000000, -87.50000000000000000 ) ) ;
#14817 = ORIENTED_EDGE ( 'NONE', *, *, #12250, .F. ) ;
#14818 = CARTESIAN_POINT ( 'NONE',  ( 9.185733585337914064, -2.352830851074140472, 1.500000000000001332 ) ) ;
#14819 = EDGE_LOOP ( 'NONE', ( #15727, #23341, #9340, #25609 ) ) ;
#14820 = AXIS2_PLACEMENT_3D ( 'NONE', #30650, #19273, #18824 ) ;
#14821 = CARTESIAN_POINT ( 'NONE',  ( 16.16412758434837471, -5.502972621964714151, 6.233981582756856987 ) ) ;
#14822 = AXIS2_PLACEMENT_3D ( 'NONE', #23994, #28855, #18878 ) ;
#14823 = DIRECTION ( 'NONE',  ( 0.000000000000000000, 0.000000000000000000, 1.000000000000000000 ) ) ;
#14824 = CARTESIAN_POINT ( 'NONE',  ( -28.20443790117967708, -1.387778780781445676E-14, -1.500000000000000000 ) ) ;
#14825 = VECTOR ( 'NONE', #27552, 1000.000000000000000 ) ;
#14826 = VERTEX_POINT ( 'NONE', #1851 ) ;
#14827 = DIRECTION ( 'NONE',  ( 1.000000000000000000, 0.000000000000000000, 0.000000000000000000 ) ) ;
#14828 = DIRECTION ( 'NONE',  ( 0.000000000000000000, 0.000000000000000000, -1.000000000000000000 ) ) ;
#14829 = DIRECTION ( 'NONE',  ( 1.000000000000000000, 0.000000000000000000, 0.000000000000000000 ) ) ;
#14830 = CARTESIAN_POINT ( 'NONE',  ( 19.13430944348616691, 33.52606101487586443, 34.49999999999999289 ) ) ;
#14831 = CIRCLE ( 'NONE', #24813, 5.000000000000004441 ) ;
#14832 = CARTESIAN_POINT ( 'NONE',  ( 0.000000000000000000, 0.000000000000000000, 21.50000000000000000 ) ) ;
#14833 = CARTESIAN_POINT ( 'NONE',  ( 9.007065134480612301, -14.44288896217592111, 19.45164628100866722 ) ) ;
#14834 = LINE ( 'NONE', #24500, #19323 ) ;
#14835 = EDGE_LOOP ( 'NONE', ( #8952, #3237 ) ) ;
#14836 = DIRECTION ( 'NONE',  ( 0.000000000000000000, 1.000000000000000000, 0.000000000000000000 ) ) ;
#14837 = LINE ( 'NONE', #24349, #18252 ) ;
#14838 = CARTESIAN_POINT ( 'NONE',  ( -35.76344986165608475, 22.29344514668535027, -19.50000000000000355 ) ) ;
#14839 = CARTESIAN_POINT ( 'NONE',  ( -0.6237340761795794331, 8.999114229549594057, 21.50000000000000000 ) ) ;
#14840 = CARTESIAN_POINT ( 'NONE',  ( 31.80202249548025861, -24.60530730987961689, 8.135760915160240359 ) ) ;
#14841 = TOROIDAL_SURFACE ( 'NONE', #6871, 6.600000000000001421, 0.5999999999999999778 ) ;
#14842 = CARTESIAN_POINT ( 'NONE',  ( -1.000000000000008438, 13.00000000000001421, 43.10779406592839536 ) ) ;
#14843 = CARTESIAN_POINT ( 'NONE',  ( -15.17592917621934845, 13.02713289664471397, 18.37250658438899009 ) ) ;
#14844 = CARTESIAN_POINT ( 'NONE',  ( -4.937793815610304726, 6.974883619896852238, -3.621320343559650379 ) ) ;
#14845 = AXIS2_PLACEMENT_3D ( 'NONE', #4775, #12435, #21463 ) ;
#14846 = CARTESIAN_POINT ( 'NONE',  ( 19.64114023396890829, 37.13592150528549496, -1.500000000000000000 ) ) ;
#14847 = VECTOR ( 'NONE', #6216, 1000.000000000000000 ) ;
#14848 = FACE_OUTER_BOUND ( 'NONE', #29670, .T. ) ;
#14849 = CARTESIAN_POINT ( 'NONE',  ( 14.39597666885513050, 39.52646374787653372, 29.10435809556016551 ) ) ;
#14850 = EDGE_CURVE ( 'NONE', #11240, #9760, #22581, .T. ) ;
#14851 = CARTESIAN_POINT ( 'NONE',  ( 19.65528207207770350, 3.699272045506078577, 5.779535427900762024 ) ) ;
#14852 = EDGE_LOOP ( 'NONE', ( #16816, #2645 ) ) ;
#14853 = DIRECTION ( 'NONE',  ( -1.000000000000000000, -0.000000000000000000, -0.000000000000000000 ) ) ;
#14855 = ORIENTED_EDGE ( 'NONE', *, *, #6296, .F. ) ;
#14854 = VECTOR ( 'NONE', #15162, 1000.000000000000000 ) ;
#14856 = DIRECTION ( 'NONE',  ( -0.000000000000000000, -0.000000000000000000, -1.000000000000000000 ) ) ;
#14857 = ORIENTED_EDGE ( 'NONE', *, *, #17035, .T. ) ;
#14858 = ORIENTED_EDGE ( 'NONE', *, *, #18875, .F. ) ;
#14859 = FACE_OUTER_BOUND ( 'NONE', #25975, .T. ) ;
#14860 = VERTEX_POINT ( 'NONE', #8720 ) ;
#14861 = ORIENTED_EDGE ( 'NONE', *, *, #30346, .F. ) ;
#14862 = ORIENTED_EDGE ( 'NONE', *, *, #19457, .T. ) ;
#14863 = CARTESIAN_POINT ( 'NONE',  ( -32.50000000000000000, 0.000000000000000000, -52.50000000000000000 ) ) ;
#14864 = CARTESIAN_POINT ( 'NONE',  ( 0.000000000000000000, 65.00000000000000000, 50.49999999999998579 ) ) ;
#14865 = CARTESIAN_POINT ( 'NONE',  ( 0.000000000000000000, -2.435693370351110282E-15, 21.50000000000000355 ) ) ;
#14866 = AXIS2_PLACEMENT_3D ( 'NONE', #19404, #28463, #2243 ) ;
#14867 = DIRECTION ( 'NONE',  ( -0.000000000000000000, -1.000000000000000000, -0.000000000000000000 ) ) ;
#14868 = DIRECTION ( 'NONE',  ( -1.000000000000000000, 0.000000000000000000, 0.000000000000000000 ) ) ;
#14869 = AXIS2_PLACEMENT_3D ( 'NONE', #21782, #717, #26313 ) ;
#14870 = TOROIDAL_SURFACE ( 'NONE', #1446, 6.600000000000001421, 0.5999999999999999778 ) ;
#14871 = EDGE_LOOP ( 'NONE', ( #12462, #17301, #15721, #13600 ) ) ;
#14872 = CARTESIAN_POINT ( 'NONE',  ( 24.35970437652574105, 13.37404834226503958, 42.96778633356035471 ) ) ;
#14873 = CYLINDRICAL_SURFACE ( 'NONE', #30033, 9.482273699623480212 ) ;
#14874 = CARTESIAN_POINT ( 'NONE',  ( 0.9949940796826640677, -19.99317329078836991, 5.872146474157316831 ) ) ;
#14875 = CARTESIAN_POINT ( 'NONE',  ( 17.22181377297005866, 14.41708049311048789, 1.500000000000000000 ) ) ;
#14876 = ORIENTED_EDGE ( 'NONE', *, *, #14117, .T. ) ;
#14877 = VECTOR ( 'NONE', #17724, 1000.000000000000000 ) ;
#14878 = FACE_OUTER_BOUND ( 'NONE', #7559, .T. ) ;
#14879 = DIRECTION ( 'NONE',  ( 1.000000000000000000, 0.000000000000000000, 0.000000000000000000 ) ) ;
#14880 = CARTESIAN_POINT ( 'NONE',  ( -6.934698339095104025, 18.77804097180239395, 6.782048567692550378 ) ) ;
#14881 = CARTESIAN_POINT ( 'NONE',  ( 10.64246886845954698, -13.35396698543974203, 6.995624166085161910 ) ) ;
#14882 = ADVANCED_FACE ( 'NONE', ( #1244 ), #6068, .F. ) ;
#14883 = ADVANCED_FACE ( 'NONE', ( #13256 ), #1404, .F. ) ;
#14884 = DIRECTION ( 'NONE',  ( 0.000000000000000000, 0.000000000000000000, 1.000000000000000000 ) ) ;
#14885 = LINE ( 'NONE', #22373, #16574 ) ;
#14886 = ORIENTED_EDGE ( 'NONE', *, *, #11905, .F. ) ;
#14887 = EDGE_LOOP ( 'NONE', ( #9878, #26987, #18795, #4009, #2780, #18507, #21138, #1861, #16577, #1118 ) ) ;
#14888 = CARTESIAN_POINT ( 'NONE',  ( -70.00000000000000000, 50.00000000000000000, 59.49999999999999289 ) ) ;
#14889 = CARTESIAN_POINT ( 'NONE',  ( -40.00000000000002842, 80.00000000000001421, 57.50000000000015632 ) ) ;
#14890 = CARTESIAN_POINT ( 'NONE',  ( 33.56327786402390245, 10.34181101807379299, 39.87954049117193023 ) ) ;
#14891 = EDGE_CURVE ( 'NONE', #315, #14448, #21329, .T. ) ;
#14892 = CARTESIAN_POINT ( 'NONE',  ( -50.00000000000000000, 50.00000000000000000, 62.49999999999999289 ) ) ;
#14893 = ORIENTED_EDGE ( 'NONE', *, *, #5099, .F. ) ;
#14894 = SHAPE_DEFINITION_REPRESENTATION ( #30827, #28257 ) ;
#14895 = LINE ( 'NONE', #3048, #5955 ) ;
#14896 = AXIS2_PLACEMENT_3D ( 'NONE', #9281, #30348, #4602 ) ;
#14897 = FACE_OUTER_BOUND ( 'NONE', #12294, .T. ) ;
#14898 = EDGE_CURVE ( 'NONE', #4424, #25108, #16190, .T. ) ;
#14899 = ORIENTED_EDGE ( 'NONE', *, *, #26128, .T. ) ;
#14900 = LINE ( 'NONE', #7894, #16770 ) ;
#14901 = CARTESIAN_POINT ( 'NONE',  ( 0.000000000000000000, 0.000000000000000000, 1.500000000000001332 ) ) ;
#14902 = VECTOR ( 'NONE', #22446, 1000.000000000000000 ) ;
#14903 = EDGE_CURVE ( 'NONE', #10854, #22904, #13141, .T. ) ;
#14904 = FACE_OUTER_BOUND ( 'NONE', #1454, .T. ) ;
#14905 = CARTESIAN_POINT ( 'NONE',  ( -25.40309444575802900, -32.28060097791307470, 34.51338776223392557 ) ) ;
#14906 = EDGE_LOOP ( 'NONE', ( #7828, #17695, #19335, #15929 ) ) ;
#14907 = LINE ( 'NONE', #13041, #14337 ) ;
#14908 = EDGE_CURVE ( 'NONE', #10764, #28271, #9084, .T. ) ;
#14909 = CARTESIAN_POINT ( 'NONE',  ( 6.899999999999999467, -10.39230484541329247, 0.000000000000000000 ) ) ;
#14910 = AXIS2_PLACEMENT_3D ( 'NONE', #1707, #21026, #18700 ) ;
#14911 = CYLINDRICAL_SURFACE ( 'NONE', #9338, 0.7500000000000006661 ) ;
#14912 = CARTESIAN_POINT ( 'NONE',  ( -19.84344116185556217, 2.497567387674351824, 20.34789198813115263 ) ) ;
#14913 = ORIENTED_EDGE ( 'NONE', *, *, #28215, .T. ) ;
#14914 = DIRECTION ( 'NONE',  ( 0.000000000000000000, 0.000000000000000000, -1.000000000000000000 ) ) ;
#14915 = CARTESIAN_POINT ( 'NONE',  ( -14.44122519041009234, -13.83658248990211348, 1.500000000000001332 ) ) ;
#14916 = PRODUCT ( 'Front & Rear Ported Pressure', 'Front & Rear Ported Pressure', '', ( #26918 ) ) ;
#14917 = LINE ( 'NONE', #17567, #9789 ) ;
#14918 = DIRECTION ( 'NONE',  ( -0.000000000000000000, -0.000000000000000000, 1.000000000000000000 ) ) ;
#14919 = DIRECTION ( 'NONE',  ( -0.000000000000000000, 0.000000000000000000, 1.000000000000000000 ) ) ;
#14920 = LINE ( 'NONE', #19293, #6900 ) ;
#14921 = ORIENTED_EDGE ( 'NONE', *, *, #22526, .F. ) ;
#14922 = EDGE_CURVE ( 'NONE', #52, #6549, #16500, .T. ) ;
#14923 = EDGE_CURVE ( 'NONE', #19418, #24377, #18745, .T. ) ;
#14924 = FACE_OUTER_BOUND ( 'NONE', #13475, .T. ) ;
#14925 = VECTOR ( 'NONE', #21879, 1000.000000000000000 ) ;
#14926 = CARTESIAN_POINT ( 'NONE',  ( -5.524309650260710747, 7.706848733601013635, 13.00000000000000178 ) ) ;
#14927 = ORIENTED_EDGE ( 'NONE', *, *, #9078, .F. ) ;
#14928 = ORIENTED_EDGE ( 'NONE', *, *, #28663, .F. ) ;
#14929 = CARTESIAN_POINT ( 'NONE',  ( -31.56327786402390245, 10.34181101807378944, -16.55003854064094426 ) ) ;
#14930 = CARTESIAN_POINT ( 'NONE',  ( -14.51554025688286309, 47.84704637152103857, -58.90721167866684738 ) ) ;
#14931 = EDGE_CURVE ( 'NONE', #27751, #1760, #271, .T. ) ;
#14932 = ORIENTED_EDGE ( 'NONE', *, *, #5573, .F. ) ;
#14933 = VECTOR ( 'NONE', #13527, 1000.000000000000000 ) ;
#14934 = CARTESIAN_POINT ( 'NONE',  ( 12.94832566568965504, 11.05145698499349649, 18.90679857307105749 ) ) ;
#14935 = CARTESIAN_POINT ( 'NONE',  ( -9.351023488831160080, -14.22394595406099782, 6.310736198168394928 ) ) ;
#14936 = EDGE_CURVE ( 'NONE', #13113, #10117, #4156, .T. ) ;
#14937 = ORIENTED_EDGE ( 'NONE', *, *, #13909, .F. ) ;
#14938 = DIRECTION ( 'NONE',  ( -0.000000000000000000, -0.000000000000000000, 1.000000000000000000 ) ) ;
#14939 = CARTESIAN_POINT ( 'NONE',  ( 16.71904594334103322, 3.341332093703275330, 20.33971507717571114 ) ) ;
#14940 = CARTESIAN_POINT ( 'NONE',  ( 0.000000000000000000, 90.00000000000001421, 0.000000000000000000 ) ) ;
#14941 = ORIENTED_EDGE ( 'NONE', *, *, #19646, .F. ) ;
#14942 = CARTESIAN_POINT ( 'NONE',  ( 23.44182307864140569, -12.68276878097691807, 44.10491087720090064 ) ) ;
#14943 = CIRCLE ( 'NONE', #20429, 1.447898107987198646 ) ;
#14944 = CARTESIAN_POINT ( 'NONE',  ( 33.89076711745516235, -13.33308044341245768, 27.49999999999999645 ) ) ;
#14945 = VERTEX_POINT ( 'NONE', #14150 ) ;
#14946 = EDGE_CURVE ( 'NONE', #16514, #7638, #179, .T. ) ;
#14947 = CARTESIAN_POINT ( 'NONE',  ( 33.36352722101803892, 22.16012013285964599, 30.86670504923349512 ) ) ;
#14948 = CARTESIAN_POINT ( 'NONE',  ( -6.145639756558241018, 15.91995507688107026, 20.13759033520874908 ) ) ;
#14949 = CARTESIAN_POINT ( 'NONE',  ( -14.88094288956370370, 13.38957456607570506, 20.05479082170252525 ) ) ;
#14950 = EDGE_CURVE ( 'NONE', #26251, #25239, #28824, .T. ) ;
#14951 = CARTESIAN_POINT ( 'NONE',  ( -23.17581250239728519, 34.50630206824671831, 1.499999999999999778 ) ) ;
#14952 = CARTESIAN_POINT ( 'NONE',  ( -31.99717184760054423, -24.33433105396149543, 30.64030087745031850 ) ) ;
#14953 = CARTESIAN_POINT ( 'NONE',  ( -4.776122516674677878E-15, -42.50000000000000000, 27.50000000000000355 ) ) ;
#14954 = DIRECTION ( 'NONE',  ( 0.1423148382732746797, -0.9898214418809342385, 0.000000000000000000 ) ) ;
#14955 = ORIENTED_EDGE ( 'NONE', *, *, #15129, .T. ) ;
#14956 = CARTESIAN_POINT ( 'NONE',  ( 9.801156115998400864, -13.94312737849039685, 5.653912893140659257 ) ) ;
#14957 = CARTESIAN_POINT ( 'NONE',  ( 29.54399056023980918, -22.57198099544491754, 34.49999999999999289 ) ) ;
#14958 = CARTESIAN_POINT ( 'NONE',  ( 19.85594780280178639, 2.397944088302079724, 6.033082186765058808 ) ) ;
#14959 = EDGE_LOOP ( 'NONE', ( #20320, #10606 ) ) ;
#14960 = EDGE_LOOP ( 'NONE', ( #11462, #7152, #17294, #22608 ) ) ;
#14961 = CARTESIAN_POINT ( 'NONE',  ( 17.92197892105641799, -8.877232523309841028, 19.08232364404838677 ) ) ;
#14962 = CARTESIAN_POINT ( 'NONE',  ( 22.58267429318971864, 26.57182937991349903, -1.500000000000001332 ) ) ;
#14963 = CARTESIAN_POINT ( 'NONE',  ( 18.71865409427299909, -7.043577866502360507, 19.21940439362676400 ) ) ;
#14964 = CARTESIAN_POINT ( 'NONE',  ( 11.67912593705722735, 12.45929511321702776, 6.917457548096559883 ) ) ;
#14965 = AXIS2_PLACEMENT_3D ( 'NONE', #3906, #23372, #6542 ) ;
#14966 = DIRECTION ( 'NONE',  ( 0.000000000000000000, 0.000000000000000000, 1.000000000000000000 ) ) ;
#14967 = CARTESIAN_POINT ( 'NONE',  ( 5.545588074468602358, 19.21617731956022368, 5.676722608126683944 ) ) ;
#14968 = ORIENTED_EDGE ( 'NONE', *, *, #16829, .F. ) ;
#14969 = CARTESIAN_POINT ( 'NONE',  ( -9.978083804712666094, -17.33339668284229873, 18.54958172136247896 ) ) ;
#14970 = CARTESIAN_POINT ( 'NONE',  ( 22.58267429318971864, 26.57182937991349903, 1.500000000000000000 ) ) ;
#14971 = CARTESIAN_POINT ( 'NONE',  ( 16.80805182381675422, 2.764250834391624334, 5.749228751562096562 ) ) ;
#14972 = VERTEX_POINT ( 'NONE', #22410 ) ;
#14973 = DIRECTION ( 'NONE',  ( 1.000000000000000000, 0.000000000000000000, -0.000000000000000000 ) ) ;
#14974 = EDGE_LOOP ( 'NONE', ( #18058, #30595, #15255, #3949 ) ) ;
#14975 = CARTESIAN_POINT ( 'NONE',  ( 16.18635831298873740, -5.444400941729625742, 6.892848776733236704 ) ) ;
#14976 = CARTESIAN_POINT ( 'NONE',  ( 30.50257113119998564, -15.54031451041691447, 36.52435908487338168 ) ) ;
#14977 = CARTESIAN_POINT ( 'NONE',  ( 0.1262659238204208167, 8.999114229549594057, -3.621320343559650379 ) ) ;
#14978 = ORIENTED_EDGE ( 'NONE', *, *, #3881, .T. ) ;
#14979 = DIRECTION ( 'NONE',  ( -1.000000000000000000, 0.000000000000000000, 0.000000000000000000 ) ) ;
#14980 = AXIS2_PLACEMENT_3D ( 'NONE', #30142, #25000, #13155 ) ;
#14981 = CARTESIAN_POINT ( 'NONE',  ( -50.00000000000000000, -50.00000000000000000, -87.50000000000000000 ) ) ;
#14982 = CARTESIAN_POINT ( 'NONE',  ( 37.16608720827707657, 36.86186943028246787, 97.07879600563551037 ) ) ;
#14983 = CARTESIAN_POINT ( 'NONE',  ( 0.000000000000000000, 39.50000000000000000, 34.49999999999999289 ) ) ;
#14984 = CIRCLE ( 'NONE', #23953, 3.559164065751841743 ) ;
#14985 = EDGE_CURVE ( 'NONE', #10252, #10893, #12453, .T. ) ;
#14986 = CARTESIAN_POINT ( 'NONE',  ( -15.85884089648730999, 35.55173462727350397, 34.80090346875804386 ) ) ;
#14987 = CARTESIAN_POINT ( 'NONE',  ( 10.44014025173321514, -17.07989312292649586, 19.96783386855779341 ) ) ;
#14988 = CARTESIAN_POINT ( 'NONE',  ( 10.36341371996391736, -17.10561997787537081, 19.85261563089511938 ) ) ;
#14989 = ORIENTED_EDGE ( 'NONE', *, *, #19853, .T. ) ;
#14990 = CARTESIAN_POINT ( 'NONE',  ( -27.03074382657074182, -6.449748410230987439, 47.21042702067970964 ) ) ;
#14991 = CARTESIAN_POINT ( 'NONE',  ( -15.56646378676712672, 12.58598989586694827, 20.29915277494337644 ) ) ;
#14992 = DIRECTION ( 'NONE',  ( -0.4154150130018972598, -0.9096319953545133341, 0.000000000000000000 ) ) ;
#14993 = ORIENTED_EDGE ( 'NONE', *, *, #17202, .F. ) ;
#14994 = CARTESIAN_POINT ( 'NONE',  ( 28.22630106158077723, -29.32773264757057419, 11.45922263815823960 ) ) ;
#14995 = LINE ( 'NONE', #24827, #8761 ) ;
#14996 = CARTESIAN_POINT ( 'NONE',  ( 0.000000000000000000, 0.000000000000000000, 21.50000000000000000 ) ) ;
#14997 = LINE ( 'NONE', #17820, #15259 ) ;
#14998 = CARTESIAN_POINT ( 'NONE',  ( -32.74775157610760346, -27.21557300919352329, -19.50000000000000355 ) ) ;
#14999 = CARTESIAN_POINT ( 'NONE',  ( -21.71568325578193637, 0.000000000000000000, 1.500000000000000000 ) ) ;
#15000 = CARTESIAN_POINT ( 'NONE',  ( 16.87360174012151504, 2.245128340637304376, 6.973843882838226094 ) ) ;
#15001 = CARTESIAN_POINT ( 'NONE',  ( -4.163336342344337027E-14, -1.387778780781445676E-14, 1.500000000000000000 ) ) ;
#15002 = ORIENTED_EDGE ( 'NONE', *, *, #24020, .T. ) ;
#15003 = AXIS2_PLACEMENT_3D ( 'NONE', #20322, #3483, #27812 ) ;
#15004 = DIRECTION ( 'NONE',  ( -0.000000000000000000, 1.669238443041286689E-16, 1.000000000000000000 ) ) ;
#15005 = CARTESIAN_POINT ( 'NONE',  ( -32.51029891075602052, -26.37762732681785494, -16.50000000000000000 ) ) ;
#15006 = CARTESIAN_POINT ( 'NONE',  ( 0.000000000000000000, 10.00000000000000888, 157.4999999999999716 ) ) ;
#15007 = ORIENTED_EDGE ( 'NONE', *, *, #10197, .T. ) ;
#15008 = EDGE_LOOP ( 'NONE', ( #14260, #7991, #27535, #16714 ) ) ;
#15009 = CARTESIAN_POINT ( 'NONE',  ( -9.635826629942096488, -17.52571954072710980, 6.523620417364432100 ) ) ;
#15010 = ORIENTED_EDGE ( 'NONE', *, *, #22919, .F. ) ;
#15011 = ORIENTED_EDGE ( 'NONE', *, *, #3856, .F. ) ;
#15012 = DIRECTION ( 'NONE',  ( 0.6707505147970023174, -0.7416830501633134842, 0.000000000000000000 ) ) ;
#15013 = DIRECTION ( 'NONE',  ( 1.982541115402065110E-16, 0.000000000000000000, -1.000000000000000000 ) ) ;
#15014 = CIRCLE ( 'NONE', #2057, 1.000000000000004441 ) ;
#15015 = DIRECTION ( 'NONE',  ( 1.000000000000000000, 0.000000000000000000, 0.000000000000000000 ) ) ;
#15016 = CARTESIAN_POINT ( 'NONE',  ( -8.499586724479453181, -2.959227181723774525, -1.500000000000002220 ) ) ;
#15017 = LINE ( 'NONE', #12701, #3309 ) ;
#15018 = EDGE_LOOP ( 'NONE', ( #13639, #20510 ) ) ;
#15019 = CARTESIAN_POINT ( 'NONE',  ( -11.33743862782229250, -16.47619710613050614, 6.386539667786095720 ) ) ;
#15020 = CARTESIAN_POINT ( 'NONE',  ( -3.221450758838616757, -1.621276839356792454, -1.500000000000000000 ) ) ;
#15021 = FILL_AREA_STYLE ('',( #17377 ) ) ;
#15022 = FACE_BOUND ( 'NONE', #20293, .T. ) ;
#15023 = ORIENTED_EDGE ( 'NONE', *, *, #24989, .T. ) ;
#15024 = AXIS2_PLACEMENT_3D ( 'NONE', #19510, #17484, #14668 ) ;
#15025 = CARTESIAN_POINT ( 'NONE',  ( -9.389232999038368277, -14.19758896559616623, 19.22654678686458141 ) ) ;
#15026 = CARTESIAN_POINT ( 'NONE',  ( -17.62838677698389134, -9.483948870226234007, 6.995624166085161910 ) ) ;
#15027 = CARTESIAN_POINT ( 'NONE',  ( -6.307863225249116468, 15.86248630188382869, 6.041646659195333058 ) ) ;
#15028 = CARTESIAN_POINT ( 'NONE',  ( 10.14446381905445271, -13.71082019663805163, 5.704143890883081269 ) ) ;
#15029 = CARTESIAN_POINT ( 'NONE',  ( 4.336808689942017736E-16, 42.50000000000000000, -1.500000000000000000 ) ) ;
#15030 = CARTESIAN_POINT ( 'NONE',  ( -19.84404562991029763, 2.492760124447683800, 18.34798005863226678 ) ) ;
#15031 = ORIENTED_EDGE ( 'NONE', *, *, #24313, .F. ) ;
#15032 = VERTEX_POINT ( 'NONE', #10412 ) ;
#15033 = CARTESIAN_POINT ( 'NONE',  ( 69.99999999999998579, -50.00000000000000000, -92.50000000000000000 ) ) ;
#15034 = CARTESIAN_POINT ( 'NONE',  ( -5.001173922442007758, 19.36461358832318425, 19.21471108562413832 ) ) ;
#15035 = CARTESIAN_POINT ( 'NONE',  ( 1.577737821089430392, -37.47138393967439640, 37.49999999998041744 ) ) ;
#15037 = VECTOR ( 'NONE', #18760, 1000.000000000000000 ) ;
#15036 = CARTESIAN_POINT ( 'NONE',  ( -7.341751895053199917, 5.349779314757666882, -1.500000000000001110 ) ) ;
#15038 = ORIENTED_EDGE ( 'NONE', *, *, #9638, .T. ) ;
#15039 = PRODUCT_CONTEXT ( 'NONE', #29700, 'mechanical' ) ;
#15040 = B_SPLINE_CURVE_WITH_KNOTS ( 'NONE', 3,
 ( #8538, #15683, #21976, #7787, #13207, #18193, #3842, #6026, #11019, #605, #22696, #19486, #1348, #6332, #15847, #28998, #7635, #16001, #25825, #16608 ),
 .UNSPECIFIED., .F., .F.,
 ( 4, 2, 2, 2, 2, 2, 2, 2, 2, 4 ),
 ( 0.000000000000000000, 0.06249999999999993755, 0.1249999999999998751, 0.1874999999999998057, 0.2187499999999996669, 0.2499999999999994726, 0.3124999999999996114, 0.3749999999999996114, 0.4374999999999996669, 0.4999999999999997224 ),
 .UNSPECIFIED. ) ;
#15041 = CARTESIAN_POINT ( 'NONE',  ( 18.17321615974886129, -8.393345561651576858, 18.44501272782439827 ) ) ;
#15042 = CARTESIAN_POINT ( 'NONE',  ( 25.47847050916411504, 26.57182937991349903, 24.50000000000000000 ) ) ;
#15043 = ORIENTED_EDGE ( 'NONE', *, *, #6512, .T. ) ;
#15044 = CARTESIAN_POINT ( 'NONE',  ( 5.372849316406060005, 19.28330981562107027, 18.34969686940295830 ) ) ;
#15045 = CARTESIAN_POINT ( 'NONE',  ( -19.50000000000000711, 1.046363422724301872E-14, 51.25735931288069480 ) ) ;
#15046 = DIRECTION ( 'NONE',  ( -0.6707505147970024284, -0.7416830501633134842, 0.000000000000000000 ) ) ;
#15047 = CARTESIAN_POINT ( 'NONE',  ( -38.24313799765437949, -8.361081211805744928, 35.00208094606055909 ) ) ;
#15048 = ORIENTED_EDGE ( 'NONE', *, *, #7357, .F. ) ;
#15049 = CARTESIAN_POINT ( 'NONE',  ( 11.61739189738757183, -16.28020533589259955, 7.454606537396342603 ) ) ;
#15050 = CARTESIAN_POINT ( 'NONE',  ( 0.000000000000000000, 0.000000000000000000, 1.500000000000001332 ) ) ;
#15051 = CARTESIAN_POINT ( 'NONE',  ( 3.668292057956000551, -8.743977807160085547, 21.50000000000000000 ) ) ;
#15052 = CARTESIAN_POINT ( 'NONE',  ( -19.72672318758257148, 3.296256974645891180, 19.96302680909625238 ) ) ;
#15053 = VERTEX_POINT ( 'NONE', #571 ) ;
#15054 = CYLINDRICAL_SURFACE ( 'NONE', #20274, 14.52510309069108807 ) ;
#15055 = AXIS2_PLACEMENT_3D ( 'NONE', #27528, #6302, #18018 ) ;
#15056 = CARTESIAN_POINT ( 'NONE',  ( 16.19468640091380962, -5.422205736210276683, 6.783738457429056901 ) ) ;
#15057 = ADVANCED_FACE ( 'NONE', ( #7926 ), #8076, .F. ) ;
#15058 = VECTOR ( 'NONE', #30837, 1000.000000000000000 ) ;
#15059 = CARTESIAN_POINT ( 'NONE',  ( -49.73013633871049421, 69.99829191145150276, 20.16832805650060934 ) ) ;
#15060 = CARTESIAN_POINT ( 'NONE',  ( -28.34828976096172681, 29.18752572968383419, -1.500000000000000000 ) ) ;
#15061 = FACE_OUTER_BOUND ( 'NONE', #9710, .T. ) ;
#15062 = CARTESIAN_POINT ( 'NONE',  ( 37.49382109471516600, -11.70052473558270556, 15.17456354887356795 ) ) ;
#15063 = CARTESIAN_POINT ( 'NONE',  ( -77.99999999999998579, 42.50000000000000711, 32.33822642395377045 ) ) ;
#15064 = ORIENTED_EDGE ( 'NONE', *, *, #24863, .T. ) ;
#15065 = CARTESIAN_POINT ( 'NONE',  ( 11.64054540341803978, 16.26338533980433709, 1.500000000000001332 ) ) ;
#15066 = CARTESIAN_POINT ( 'NONE',  ( 5.035381156335487773, 19.35612728853643105, 5.679672709359370408 ) ) ;
#15067 = EDGE_CURVE ( 'NONE', #9122, #8016, #12150, .T. ) ;
#15068 = VERTEX_POINT ( 'NONE', #24585 ) ;
#15069 = ORIENTED_EDGE ( 'NONE', *, *, #24566, .T. ) ;
#15070 = EDGE_CURVE ( 'NONE', #20436, #19427, #17126, .T. ) ;
#15071 = CARTESIAN_POINT ( 'NONE',  ( -2.703030265324078307, -12.75514121382991384, 1.500000000000001332 ) ) ;
#15072 = DIRECTION ( 'NONE',  ( 1.000000000000000000, 0.000000000000000000, 0.000000000000000000 ) ) ;
#15073 = EDGE_LOOP ( 'NONE', ( #2663, #9832, #25732, #1522, #1271 ) ) ;
#15074 = CARTESIAN_POINT ( 'NONE',  ( -26.83887921667331966, -26.32914559372739660, 27.50000000000000000 ) ) ;
#15075 = CARTESIAN_POINT ( 'NONE',  ( 15.36220013476732404, 12.83425670785759110, 18.63641924841378028 ) ) ;
#15076 = ORIENTED_EDGE ( 'NONE', *, *, #26840, .T. ) ;
#15077 = VECTOR ( 'NONE', #5376, 1000.000000000000000 ) ;
#15078 = CARTESIAN_POINT ( 'NONE',  ( 57.49999999999998579, 50.00000000000000000, 12.49999999999999112 ) ) ;
#15079 = DIRECTION ( 'NONE',  ( -0.000000000000000000, 1.132880637372608986E-16, -1.000000000000000000 ) ) ;
#15080 = CARTESIAN_POINT ( 'NONE',  ( 40.57596378766727696, -1.195117231327979868, -16.50000000000000000 ) ) ;
#15081 = ORIENTED_EDGE ( 'NONE', *, *, #24216, .T. ) ;
#15082 = FACE_OUTER_BOUND ( 'NONE', #14906, .T. ) ;
#15083 = EDGE_CURVE ( 'NONE', #9540, #30466, #12750, .T. ) ;
#15084 = ADVANCED_FACE ( 'NONE', ( #15214 ), #19754, .F. ) ;
#15085 = EDGE_CURVE ( 'NONE', #22374, #346, #7605, .T. ) ;
#15086 = CARTESIAN_POINT ( 'NONE',  ( -16.89625272878630469, 2.150609578401780020, 18.47056384035244037 ) ) ;
#15087 = EDGE_CURVE ( 'NONE', #24759, #9785, #22833, .T. ) ;
#15088 = ORIENTED_EDGE ( 'NONE', *, *, #17241, .F. ) ;
#15089 = FACE_OUTER_BOUND ( 'NONE', #13190, .T. ) ;
#15090 = EDGE_CURVE ( 'NONE', #3354, #7456, #12916, .T. ) ;
#15091 = CARTESIAN_POINT ( 'NONE',  ( 31.92585768990164397, -26.59981599195955226, -13.16665969525543289 ) ) ;
#15092 = B_SPLINE_SURFACE_WITH_KNOTS ( 'NONE', 3, 1, ( 
 ( #7468, #4965 ),
 ( #26643, #26172 ),
 ( #28980, #14474 ),
 ( #7615, #14778 ),
 ( #23976, #24296 ),
 ( #11832, #14631 ),
 ( #12464, #2623 ),
 ( #21951, #10102 ),
 ( #5119, #19311 ),
 ( #12143, #6996 ),
 ( #30847, #14310 ),
 ( #26025, #16508 ),
 ( #24130, #21644 ),
 ( #14157, #126 ),
 ( #4654, #279 ),
 ( #2782, #23661 ),
 ( #9798, #21332 ),
 ( #9492, #19008 ),
 ( #12296, #28523 ),
 ( #7154, #16665 ),
 ( #4798, #23826 ),
 ( #2475, #12610 ),
 ( #13227, #3713 ),
 ( #22260, #7936 ),
 ( #27258, #22714 ),
 ( #17591, #22566 ),
 ( #8231, #900 ),
 ( #3396, #1368 ),
 ( #6041, #14939 ),
 ( #24596, #3235 ),
 ( #22419, #19613 ) ),
 .UNSPECIFIED., .F., .F., .F.,
 ( 4, 3, 3, 3, 3, 3, 3, 3, 3, 3, 4 ),
 ( 2, 2 ),
 ( 0.4999999998345686647, 0.5360336730431939367, 0.5907651151589012883, 0.6456034593241830599, 0.6998270958050434309, 0.7529536536315937223, 0.8052385063053260073, 0.8575343587103997356, 0.9106564858195042023, 0.9648414833209685293, 1.000000006602610236 ),
 ( 0.000000000000000000, 1.000000000000000000 ),
 .UNSPECIFIED. ) ;
#15093 = CARTESIAN_POINT ( 'NONE',  ( 16.58777033243661592, 4.040313317649105507, 7.196036389296800451 ) ) ;
#15094 = DIRECTION ( 'NONE',  ( 1.000000000000000000, 0.000000000000000000, 0.000000000000000000 ) ) ;
#15095 = CARTESIAN_POINT ( 'NONE',  ( -50.00000000000000000, 70.00000000000000000, -92.50000000000000000 ) ) ;
#15096 = EDGE_CURVE ( 'NONE', #26161, #7440, #16958, .T. ) ;
#15097 = CARTESIAN_POINT ( 'NONE',  ( -38.99591598333270781, -2.632255423871425304, 32.22937204864898320 ) ) ;
#15098 = VECTOR ( 'NONE', #26361, 1000.000000000000000 ) ;
#15099 = DIRECTION ( 'NONE',  ( -0.000000000000000000, -0.000000000000000000, -1.000000000000000000 ) ) ;
#15100 = LINE ( 'NONE', #5287, #14356 ) ;
#15101 = VERTEX_POINT ( 'NONE', #26476 ) ;
#15102 = ADVANCED_FACE ( 'NONE', ( #24123 ), #12287, .F. ) ;
#15103 = CIRCLE ( 'NONE', #12137, 20.00000000000000000 ) ;
#15104 = CARTESIAN_POINT ( 'NONE',  ( 11.05488513857797450, -16.68841100269527544, 5.653912893140659257 ) ) ;
#15105 = DIRECTION ( 'NONE',  ( 0.000000000000000000, 0.000000000000000000, 1.000000000000000000 ) ) ;
#15106 = DIRECTION ( 'NONE',  ( 1.000000000000000000, 0.000000000000000000, 0.000000000000000000 ) ) ;
#15107 = VERTEX_POINT ( 'NONE', #29126 ) ;
#15108 = VERTEX_POINT ( 'NONE', #19454 ) ;
#15109 = CARTESIAN_POINT ( 'NONE',  ( 33.01877980957529957, 12.12572312222181026, 35.60092001944724416 ) ) ;
#15110 = DIRECTION ( 'NONE',  ( 0.000000000000000000, -1.132880637372608986E-16, 1.000000000000000000 ) ) ;
#15111 = CARTESIAN_POINT ( 'NONE',  ( 22.95669091611932089, -27.54300778121948312, 1.500000000000000000 ) ) ;
#15112 = VERTEX_POINT ( 'NONE', #28971 ) ;
#15113 = FACE_OUTER_BOUND ( 'NONE', #11636, .T. ) ;
#15114 = LINE ( 'NONE', #3264, #2208 ) ;
#15115 = CARTESIAN_POINT ( 'NONE',  ( -31.76816150326424548, -26.51947378151102086, -11.49999299637583228 ) ) ;
#15116 = EDGE_CURVE ( 'NONE', #20109, #18178, #13659, .T. ) ;
#15117 = ORIENTED_EDGE ( 'NONE', *, *, #5666, .T. ) ;
#15118 = AXIS2_PLACEMENT_3D ( 'NONE', #9121, #4281, #20405 ) ;
#15119 = LINE ( 'NONE', #15909, #9256 ) ;
#15120 = DIRECTION ( 'NONE',  ( -0.6707505147970024284, 0.7416830501633134842, 0.000000000000000000 ) ) ;
#15121 = CARTESIAN_POINT ( 'NONE',  ( 16.87408724266514426, 2.240810012149825781, 6.974106381145714018 ) ) ;
#15122 = ORIENTED_EDGE ( 'NONE', *, *, #6690, .T. ) ;
#15123 = CARTESIAN_POINT ( 'NONE',  ( 15.57266529552203416, 38.96488032230103471, 1.500000000000000000 ) ) ;
#15124 = VECTOR ( 'NONE', #7457, 1000.000000000000114 ) ;
#15125 = EDGE_CURVE ( 'NONE', #20277, #29673, #1207, .T. ) ;
#15126 = ORIENTED_EDGE ( 'NONE', *, *, #26946, .F. ) ;
#15127 = CARTESIAN_POINT ( 'NONE',  ( 27.75715622479469147, -6.315477654728063328E-15, 24.50000000000000000 ) ) ;
#15128 = AXIS2_PLACEMENT_3D ( 'NONE', #24788, #6226, #1554 ) ;
#15129 = EDGE_CURVE ( 'NONE', #1903, #12174, #29737, .T. ) ;
#15130 = CARTESIAN_POINT ( 'NONE',  ( 31.22647667302026520, -15.32805873036034860, 35.97188228574909630 ) ) ;
#15131 = ORIENTED_EDGE ( 'NONE', *, *, #25619, .F. ) ;
#15132 = FACE_OUTER_BOUND ( 'NONE', #20615, .T. ) ;
#15133 = CARTESIAN_POINT ( 'NONE',  ( -37.16608720827707657, 36.86186943028246787, 97.07879600563551037 ) ) ;
#15134 = ORIENTED_EDGE ( 'NONE', *, *, #15690, .T. ) ;
#15135 = CARTESIAN_POINT ( 'NONE',  ( 20.76278282699725608, 32.33563723208181528, 34.49999999999999289 ) ) ;
#15136 = CARTESIAN_POINT ( 'NONE',  ( -57.50000000000001421, 50.00000000000000000, 97.07879600563551037 ) ) ;
#15137 = DIRECTION ( 'NONE',  ( 0.000000000000000000, -1.000000000000000000, 0.000000000000000000 ) ) ;
#15138 = CARTESIAN_POINT ( 'NONE',  ( -5.069257791428325888, 7.538175180318473778, 13.22130136205108819 ) ) ;
#15139 = ORIENTED_EDGE ( 'NONE', *, *, #28881, .F. ) ;
#15140 = CARTESIAN_POINT ( 'NONE',  ( -4.163336342344337027E-14, 1.387778780781445676E-14, 77.49999999999998579 ) ) ;
#15141 = CARTESIAN_POINT ( 'NONE',  ( -15.90168156411150058, 12.15925017959999899, 18.82680253904184298 ) ) ;
#15142 = CARTESIAN_POINT ( 'NONE',  ( 24.03448224033878944, -8.660042335149841009, 49.47829057475696857 ) ) ;
#15143 = ORIENTED_EDGE ( 'NONE', *, *, #1592, .T. ) ;
#15144 = CIRCLE ( 'NONE', #11177, 22.49999999999996447 ) ;
#15145 = CARTESIAN_POINT ( 'NONE',  ( 32.98805937973595093, -22.67054169308931222, 8.000000000000003553 ) ) ;
#15146 = CYLINDRICAL_SURFACE ( 'NONE', #13727, 9.482273699623480212 ) ;
#15147 = CARTESIAN_POINT ( 'NONE',  ( -14.94050307174418712, 13.29624634855318988, 18.54479204710283824 ) ) ;
#15148 = CARTESIAN_POINT ( 'NONE',  ( -37.98493438988125348, -11.12428508575252728, -1.500000000000000000 ) ) ;
#15149 = CARTESIAN_POINT ( 'NONE',  ( -0.1262659238204836554, -8.999114229549588728, 21.50000000000000000 ) ) ;
#15150 = CARTESIAN_POINT ( 'NONE',  ( 19.27189572260205708, 36.95578567799407921, 29.34714106128156885 ) ) ;
#15151 = ADVANCED_FACE ( 'NONE', ( #3700 ), #6188, .T. ) ;
#15152 = ORIENTED_EDGE ( 'NONE', *, *, #19528, .F. ) ;
#15153 = ADVANCED_FACE ( 'NONE', ( #20216 ), #15541, .T. ) ;
#15154 = CARTESIAN_POINT ( 'NONE',  ( -14.36006998371493637, -17.26937953831884442, 1.500000000000000000 ) ) ;
#15155 = ORIENTED_EDGE ( 'NONE', *, *, #10180, .T. ) ;
#15156 = DIRECTION ( 'NONE',  ( -0.8412535328311884220, -0.5406408174555862312, 0.000000000000000000 ) ) ;
#15157 = PLANE ( 'NONE',  #3517 ) ;
#15158 = ORIENTED_EDGE ( 'NONE', *, *, #20072, .T. ) ;
#15159 = EDGE_LOOP ( 'NONE', ( #14517, #28826, #15875, #14855, #2741, #14598 ) ) ;
#15160 = DIRECTION ( 'NONE',  ( -1.000000000000000000, 0.000000000000000000, 0.000000000000000000 ) ) ;
#15161 = ORIENTED_EDGE ( 'NONE', *, *, #17564, .T. ) ;
#15162 = DIRECTION ( 'NONE',  ( -0.000000000000000000, -0.000000000000000000, 1.000000000000000000 ) ) ;
#15163 = CIRCLE ( 'NONE', #25649, 20.00000000000000000 ) ;
#15164 = CARTESIAN_POINT ( 'NONE',  ( -5.971396161871752817, 19.08775596758251680, 20.34789198813115263 ) ) ;
#15165 = DIRECTION ( 'NONE',  ( 0.000000000000000000, 0.000000000000000000, 1.000000000000000000 ) ) ;
#15166 = CYLINDRICAL_SURFACE ( 'NONE', #827, 11.99999999999998224 ) ;
#15167 = LINE ( 'NONE', #19552, #21288 ) ;
#15168 = LINE ( 'NONE', #5828, #19346 ) ;
#15169 = DIRECTION ( 'NONE',  ( 1.000000000000000000, 0.000000000000000000, 0.000000000000000000 ) ) ;
#15170 = SURFACE_STYLE_FILL_AREA ( #15021 ) ;
#15171 = DIRECTION ( 'NONE',  ( -0.000000000000000000, 0.000000000000000000, 1.000000000000000000 ) ) ;
#15172 = VERTEX_POINT ( 'NONE', #27709 ) ;
#15173 = CARTESIAN_POINT ( 'NONE',  ( -11.37242378808260845, -16.47377160145866171, 19.45164628100866722 ) ) ;
#15174 = FACE_OUTER_BOUND ( 'NONE', #18882, .T. ) ;
#15175 = CARTESIAN_POINT ( 'NONE',  ( -5.296822449995555182, 16.19439135686734588, 5.676815824193228721 ) ) ;
#15176 = CARTESIAN_POINT ( 'NONE',  ( 11.63559590357233198, -16.28893981701509119, 7.441806358946449151 ) ) ;
#15177 = DIRECTION ( 'NONE',  ( 0.000000000000000000, 0.000000000000000000, 1.000000000000000000 ) ) ;
#15178 = CARTESIAN_POINT ( 'NONE',  ( 33.56327786402390245, -10.34181101807379477, 35.63689980405263924 ) ) ;
#15179 = ORIENTED_EDGE ( 'NONE', *, *, #24286, .F. ) ;
#15180 = VERTEX_POINT ( 'NONE', #11026 ) ;
#15181 = CARTESIAN_POINT ( 'NONE',  ( -32.19782014694307293, 14.25394737442115733, 35.54550565580015586 ) ) ;
#15182 = CARTESIAN_POINT ( 'NONE',  ( -2.687479362164884034, -44.39187623478217404, -19.50000000000000355 ) ) ;
#15183 = CARTESIAN_POINT ( 'NONE',  ( -5.127072262013855131, -42.13114360820154047, 28.87158698979397897 ) ) ;
#15184 = CARTESIAN_POINT ( 'NONE',  ( 25.23756106473024730, -11.43858098102957399, -16.50000000000000000 ) ) ;
#15185 = ORIENTED_EDGE ( 'NONE', *, *, #6336, .F. ) ;
#15186 = ITEM_DEFINED_TRANSFORMATION ( 'NONE', 'NONE', #10895,  #7396 ) ;
#15187 = CARTESIAN_POINT ( 'NONE',  ( 3.540451764263689682, 16.69076635161362887, 7.545655578832110244 ) ) ;
#15188 = CARTESIAN_POINT ( 'NONE',  ( -7.663215745754974328, 3.196529495465474380, -1.500000000000001332 ) ) ;
#15189 = ORIENTED_EDGE ( 'NONE', *, *, #24608, .T. ) ;
#15190 = PLANE ( 'NONE',  #29732 ) ;
#15191 = CARTESIAN_POINT ( 'NONE',  ( 0.3570196857253563061, -6.047589086025013216, 7.525268439705684820 ) ) ;
#15192 = CARTESIAN_POINT ( 'NONE',  ( -38.38780269126310429, -7.528505152340548179, 32.04353250950420318 ) ) ;
#15193 = ORIENTED_EDGE ( 'NONE', *, *, #20200, .F. ) ;
#15194 = DIRECTION ( 'NONE',  ( 1.000000000000000000, 0.000000000000000000, 0.000000000000000000 ) ) ;
#15195 = LINE ( 'NONE', #24721, #27791 ) ;
#15196 = CARTESIAN_POINT ( 'NONE',  ( -28.20443790117967708, -1.387778780781445676E-14, 1.500000000000000000 ) ) ;
#15197 = ORIENTED_EDGE ( 'NONE', *, *, #28127, .F. ) ;
#15198 = CARTESIAN_POINT ( 'NONE',  ( 9.749114229549594057, -0.1262659238204522361, 21.50000000000000000 ) ) ;
#15199 = AXIS2_PLACEMENT_3D ( 'NONE', #7652, #767, #26674 ) ;
#15200 = CARTESIAN_POINT ( 'NONE',  ( 12.99618331672382610, 10.99290767930309443, 19.08155846658118904 ) ) ;
#15201 = CARTESIAN_POINT ( 'NONE',  ( 16.14824862691416740, -5.544579173763282576, 7.158811349119585721 ) ) ;
#15202 = DIRECTION ( 'NONE',  ( 0.000000000000000000, 0.000000000000000000, -1.000000000000000000 ) ) ;
#15203 = DIRECTION ( 'NONE',  ( 1.000000000000000000, 0.000000000000000000, 0.000000000000000000 ) ) ;
#15204 = DIRECTION ( 'NONE',  ( 0.000000000000000000, 0.7709617516270895754, -0.6368814469962912339 ) ) ;
#15205 = DIRECTION ( 'NONE',  ( 1.000000000000000000, 0.000000000000000000, 0.000000000000000000 ) ) ;
#15206 = DIRECTION ( 'NONE',  ( 0.000000000000000000, -1.132880637372608986E-16, 1.000000000000000000 ) ) ;
#15207 = VERTEX_POINT ( 'NONE', #4002 ) ;
#15208 = CARTESIAN_POINT ( 'NONE',  ( -38.00000000000000000, 80.00000000000000000, -7.533656238527846826E-15 ) ) ;
#15209 = CARTESIAN_POINT ( 'NONE',  ( 6.437683520590175235, -6.962021646281549181, 13.00000000000000178 ) ) ;
#15210 = EDGE_LOOP ( 'NONE', ( #13073, #9978, #27432, #9680 ) ) ;
#15211 = VERTEX_POINT ( 'NONE', #27247 ) ;
#15212 = ADVANCED_FACE ( 'NONE', ( #8835 ), #10871, .T. ) ;
#15213 = PLANE ( 'NONE',  #21918 ) ;
#15214 = FACE_OUTER_BOUND ( 'NONE', #20347, .T. ) ;
#15215 = CARTESIAN_POINT ( 'NONE',  ( -0.4913386815044658573, 49.99999999999999289, -70.00000000000001421 ) ) ;
#15216 = CARTESIAN_POINT ( 'NONE',  ( -4.962407341831601038, -39.12863361840854282, 27.50000000000000000 ) ) ;
#15217 = LINE ( 'NONE', #26958, #25627 ) ;
#15218 = AXIS2_PLACEMENT_3D ( 'NONE', #22066, #10218, #19728 ) ;
#15219 = ORIENTED_EDGE ( 'NONE', *, *, #20349, .T. ) ;
#15220 = VERTEX_POINT ( 'NONE', #6340 ) ;
#15221 = ADVANCED_FACE ( 'NONE', ( #1051 ), #27069, .T. ) ;
#15222 = DIRECTION ( 'NONE',  ( 0.8910248307962438385, 0.4539545692076743522, 0.000000000000000000 ) ) ;
#15223 = CARTESIAN_POINT ( 'NONE',  ( 17.90987090234841261, -8.901490003858826938, 6.518927109361837502 ) ) ;
#15224 = AXIS2_PLACEMENT_3D ( 'NONE', #618, #9833, #5303 ) ;
#15225 = DIRECTION ( 'NONE',  ( -1.000000000000000000, 0.000000000000000000, 0.000000000000000000 ) ) ;
#15226 = ORIENTED_EDGE ( 'NONE', *, *, #19478, .F. ) ;
#15227 = DIRECTION ( 'NONE',  ( -1.000000000000000000, 0.000000000000000000, 0.000000000000000000 ) ) ;
#15228 = CARTESIAN_POINT ( 'NONE',  ( 40.05104235265675783, 2.353288714454550679, -11.49999999999999645 ) ) ;
#15229 = CIRCLE ( 'NONE', #1809, 23.20393738267408779 ) ;
#15230 = ORIENTED_EDGE ( 'NONE', *, *, #20682, .F. ) ;
#15231 = EDGE_CURVE ( 'NONE', #5196, #20389, #9601, .T. ) ;
#15232 = CIRCLE ( 'NONE', #9776, 23.20393738267338790 ) ;
#15233 = DIRECTION ( 'NONE',  ( 0.6548607339452782172, -0.7557495743542642641, 0.000000000000000000 ) ) ;
#15234 = LINE ( 'NONE', #29611, #7123 ) ;
#15235 = CARTESIAN_POINT ( 'NONE',  ( 19.73572331631237375, 3.349230485916621092, 5.661398277488801867 ) ) ;
#15236 = CARTESIAN_POINT ( 'NONE',  ( 37.99999999999999289, 80.00000000000000000, 0.000000000000000000 ) ) ;
#15237 = CARTESIAN_POINT ( 'NONE',  ( -10.24254388992509135, -17.19919274694469991, 20.29915277494337644 ) ) ;
#15238 = VECTOR ( 'NONE', #18877, 1000.000000000000000 ) ;
#15239 = CARTESIAN_POINT ( 'NONE',  ( 6.601643239663004076E-16, 42.50000000000000000, 28.83974596215562514 ) ) ;
#15240 = DIRECTION ( 'NONE',  ( 0.000000000000000000, 0.000000000000000000, 1.000000000000000000 ) ) ;
#15241 = CARTESIAN_POINT ( 'NONE',  ( -4.163336342344337027E-14, 1.387778780781445676E-14, 24.50000000000000000 ) ) ;
#15242 = ORIENTED_EDGE ( 'NONE', *, *, #12798, .F. ) ;
#15244 = AXIS2_PLACEMENT_3D ( 'NONE', #17675, #10190, #3026 ) ;
#15243 = CARTESIAN_POINT ( 'NONE',  ( 9.263624429760993095, -14.28705663139043480, 5.940635272151477686 ) ) ;
#15245 = CARTESIAN_POINT ( 'NONE',  ( -28.86331178595770197, 28.58238193408198313, 10.16794702317896615 ) ) ;
#15246 = EDGE_CURVE ( 'NONE', #3146, #6567, #26197, .T. ) ;
#15247 = DIRECTION ( 'NONE',  ( 0.000000000000000000, 0.000000000000000000, -1.000000000000000000 ) ) ;
#15248 = ORIENTED_EDGE ( 'NONE', *, *, #14931, .F. ) ;
#15249 = ORIENTED_EDGE ( 'NONE', *, *, #6115, .F. ) ;
#15250 = CARTESIAN_POINT ( 'NONE',  ( 0.6237340761795171495, -8.999114229549588728, 21.50000000000000000 ) ) ;
#15251 = EDGE_CURVE ( 'NONE', #4887, #27397, #27322, .T. ) ;
#15252 = DIRECTION ( 'NONE',  ( -0.000000000000000000, -0.000000000000000000, 1.000000000000000000 ) ) ;
#15253 = EDGE_CURVE ( 'NONE', #9249, #23905, #29241, .T. ) ;
#15254 = CARTESIAN_POINT ( 'NONE',  ( -5.651831417317677797, 19.20339396603468884, 7.595116371587256054 ) ) ;
#15255 = ORIENTED_EDGE ( 'NONE', *, *, #12246, .T. ) ;
#15256 = DIRECTION ( 'NONE',  ( -0.000000000000000000, -0.000000000000000000, -1.000000000000000000 ) ) ;
#15257 = AXIS2_PLACEMENT_3D ( 'NONE', #30187, #13670, #16454 ) ;
#15258 = CARTESIAN_POINT ( 'NONE',  ( 28.79137815760242702, -9.331429872129930914, 1.500000000000000000 ) ) ;
#15259 = VECTOR ( 'NONE', #19994, 1000.000000000000000 ) ;
#15260 = CARTESIAN_POINT ( 'NONE',  ( -31.61046531695933837, -26.43913157123191482, -9.833326300989435609 ) ) ;
#15261 = VERTEX_POINT ( 'NONE', #19420 ) ;
#15262 = EDGE_CURVE ( 'NONE', #19317, #5791, #11657, .T. ) ;
#15263 = CARTESIAN_POINT ( 'NONE',  ( -10.08096377525215104, -17.27393813307046599, 20.22386025856688718 ) ) ;
#15264 = VECTOR ( 'NONE', #17119, 1000.000000000000000 ) ;
#15265 = CARTESIAN_POINT ( 'NONE',  ( 2.168404344971008868E-16, 30.50000000000000000, 1.500000000000000000 ) ) ;
#15266 = CARTESIAN_POINT ( 'NONE',  ( 19.85280965686022014, 2.565335765644449761, 7.429667576816606278 ) ) ;
#15267 = ORIENTED_EDGE ( 'NONE', *, *, #4804, .T. ) ;
#15268 = AXIS2_PLACEMENT_3D ( 'NONE', #14564, #671, #24060 ) ;
#15269 = CARTESIAN_POINT ( 'NONE',  ( -17.79239818699324616, -14.89473990422481187, -1.500000000000000000 ) ) ;
#15270 = ORIENTED_EDGE ( 'NONE', *, *, #29419, .T. ) ;
#15271 = EDGE_CURVE ( 'NONE', #11996, #8846, #3195, .T. ) ;
#15272 = CARTESIAN_POINT ( 'NONE',  ( 19.18576292979354392, -22.55620591602728453, 24.50000000000000000 ) ) ;
#15273 = CIRCLE ( 'NONE', #1846, 9.000000000000000000 ) ;
#15274 = CARTESIAN_POINT ( 'NONE',  ( 9.169883732660084164, -9.268939115642975679, 24.50000000000000000 ) ) ;
#15275 = CIRCLE ( 'NONE', #28216, 0.7500000000000004441 ) ;
#15276 = EDGE_CURVE ( 'NONE', #29972, #13769, #24095, .T. ) ;
#15277 = ORIENTED_EDGE ( 'NONE', *, *, #6448, .T. ) ;
#15278 = EDGE_CURVE ( 'NONE', #12217, #2701, #3043, .T. ) ;
#15279 = B_SPLINE_CURVE_WITH_KNOTS ( 'NONE', 3,
 ( #3252, #14647, #26660, #9818, #12780, #22280, #26830, #8105, #2798, #923, #17614, #12316, #27130, #15245, #21821, #24776, #12160, #19331, #463, #28854, #28997, #7634, #5290, #24315, #2966, #12482, #5455, #20106, #1690, #20702, #15894, #3889, #18228, #6380, #27281, #15571, #27905, #18400, #20555, #6062, #22589, #20254 ),
 .UNSPECIFIED., .F., .F.,
 ( 4, 2, 2, 2, 2, 2, 2, 2, 2, 2, 2, 2, 2, 2, 2, 2, 2, 2, 2, 2, 4 ),
 ( 0.000000000000000000, 0.002689500986570608678, 0.004034251479855906729, 0.004706626726498557706, 0.005379001973141206948, 0.006723752466426514973, 0.007396127713069166817, 0.008068502959711818662, 0.009413253452997118881, 0.01008562869963976899, 0.01075800394628241910, 0.01143037919292506921, 0.01210275443956771758, 0.01277512968621036943, 0.01344750493285301780, 0.01479225542613831629, 0.01546463067278096813, 0.01613700591942361651, 0.01748175641270892366, 0.01882650690599423082, 0.02151600789256482779 ),
 .UNSPECIFIED. ) ;
#15280 = CARTESIAN_POINT ( 'NONE',  ( -17.26937953831790651, 14.36006998371489551, 1.500000000000000000 ) ) ;
#15281 = DIRECTION ( 'NONE',  ( 0.000000000000000000, 0.000000000000000000, 1.000000000000000000 ) ) ;
#15282 = FACE_OUTER_BOUND ( 'NONE', #3015, .T. ) ;
#15283 = CYLINDRICAL_SURFACE ( 'NONE', #4323, 23.20393738267273420 ) ;
#15284 = AXIS2_PLACEMENT_3D ( 'NONE', #12672, #22166, #29357 ) ;
#15285 = DIRECTION ( 'NONE',  ( -0.000000000000000000, -0.000000000000000000, -1.000000000000000000 ) ) ;
#15286 = CARTESIAN_POINT ( 'NONE',  ( -15.57266529552202883, -38.96488032230103471, 1.500000000000000000 ) ) ;
#15287 = CARTESIAN_POINT ( 'NONE',  ( 0.000000000000000000, 7.794228634059944483, -4.500000000000004441 ) ) ;
#15288 = ORIENTED_EDGE ( 'NONE', *, *, #16452, .T. ) ;
#15289 = CARTESIAN_POINT ( 'NONE',  ( 37.99999999999999289, 80.00000000000001421, 47.91742430504415040 ) ) ;
#15290 = VECTOR ( 'NONE', #18452, 1000.000000000000000 ) ;
#15291 = CARTESIAN_POINT ( 'NONE',  ( -15.84987138805250773, 12.22653209092615612, 19.97651184436794125 ) ) ;
#15292 = CARTESIAN_POINT ( 'NONE',  ( 43.65325317339704014, 67.82531247263540308, 61.81444804503984614 ) ) ;
#15293 = CARTESIAN_POINT ( 'NONE',  ( 0.000000000000000000, 0.000000000000000000, 1.500000000000001332 ) ) ;
#15294 = ORIENTED_EDGE ( 'NONE', *, *, #2235, .F. ) ;
#15295 = AXIS2_PLACEMENT_3D ( 'NONE', #8206, #7909, #19911 ) ;
#15296 = CARTESIAN_POINT ( 'NONE',  ( 28.06623213401399752, -29.50949589058133071, 13.90928673059489284 ) ) ;
#15297 = ADVANCED_FACE ( 'NONE', ( #2738 ), #4174, .T. ) ;
#15298 = DIRECTION ( 'NONE',  ( 0.000000000000000000, 0.000000000000000000, 1.000000000000000000 ) ) ;
#15299 = EDGE_CURVE ( 'NONE', #7775, #5590, #9653, .T. ) ;
#15300 = CARTESIAN_POINT ( 'NONE',  ( -23.72453467988983178, -12.99099554674205947, 47.95154756196049561 ) ) ;
#15301 = FACE_OUTER_BOUND ( 'NONE', #20967, .T. ) ;
#15302 = CYLINDRICAL_SURFACE ( 'NONE', #6166, 9.482273699623480212 ) ;
#15303 = ADVANCED_FACE ( 'NONE', ( #19718 ), #28088, .T. ) ;
#15304 = CARTESIAN_POINT ( 'NONE',  ( -4.163336342344337027E-14, 1.387778780781445676E-14, 1.500000000000000000 ) ) ;
#15305 = CARTESIAN_POINT ( 'NONE',  ( 16.76361099852355352, 3.068725842366666345, 5.651492010659115550 ) ) ;
#15306 = ORIENTED_EDGE ( 'NONE', *, *, #5383, .F. ) ;
#15307 = EDGE_CURVE ( 'NONE', #24053, #10610, #27097, .T. ) ;
#15308 = CIRCLE ( 'NONE', #16810, 4.999999999999997335 ) ;
#15309 = CARTESIAN_POINT ( 'NONE',  ( 24.50428919468314959, 7.442132857256930301, 45.14840622132430781 ) ) ;
#15310 = AXIS2_PLACEMENT_3D ( 'NONE', #15530, #20665, #30188 ) ;
#15311 = CARTESIAN_POINT ( 'NONE',  ( -33.52485258639264032, 10.76172163581451713, 39.79052675593855781 ) ) ;
#15312 = DIRECTION ( 'NONE',  ( -0.000000000000000000, -0.000000000000000000, 1.000000000000000000 ) ) ;
#15313 = VERTEX_POINT ( 'NONE', #26087 ) ;
#15314 = ORIENTED_EDGE ( 'NONE', *, *, #21525, .F. ) ;
#15315 = EDGE_CURVE ( 'NONE', #16202, #3179, #11292, .T. ) ;
#15316 = DIRECTION ( 'NONE',  ( 1.000000000000000000, 0.000000000000000000, 0.000000000000000000 ) ) ;
#15317 = CIRCLE ( 'NONE', #3900, 9.482273699623480212 ) ;
#15318 = CARTESIAN_POINT ( 'NONE',  ( -19.94274101607340910, 1.513210029880959651, 19.61564845152806313 ) ) ;
#15319 = ORIENTED_EDGE ( 'NONE', *, *, #29197, .F. ) ;
#15320 = DIRECTION ( 'NONE',  ( 1.000000000000000000, 0.000000000000000000, -0.000000000000000000 ) ) ;
#15321 = AXIS2_PLACEMENT_3D ( 'NONE', #27962, #18140, #8769 ) ;
#15322 = CARTESIAN_POINT ( 'NONE',  ( 14.80383744458522877, 47.75831397104769849, -57.46711200187744595 ) ) ;
#15323 = DIRECTION ( 'NONE',  ( 0.000000000000000000, 0.000000000000000000, -1.000000000000000000 ) ) ;
#15324 = LINE ( 'NONE', #3025, #18276 ) ;
#15325 = DIRECTION ( 'NONE',  ( 1.000000000000000000, 0.000000000000000000, -0.000000000000000000 ) ) ;
#15326 = CARTESIAN_POINT ( 'NONE',  ( -11.33851205691660624, -16.47545820588255339, 6.913388067999417963 ) ) ;
#15327 = DIRECTION ( 'NONE',  ( -0.000000000000000000, -0.000000000000000000, 1.000000000000000000 ) ) ;
#15328 = DIRECTION ( 'NONE',  ( 0.000000000000000000, 0.000000000000000000, -1.000000000000000000 ) ) ;
#15329 = AXIS2_PLACEMENT_3D ( 'NONE', #22067, #10070, #5696 ) ;
#15330 = ORIENTED_EDGE ( 'NONE', *, *, #28842, .T. ) ;
#15331 = EDGE_CURVE ( 'NONE', #9950, #20399, #18147, .T. ) ;
#15332 = AXIS2_PLACEMENT_3D ( 'NONE', #19033, #4680, #12167 ) ;
#15333 = ADVANCED_FACE ( 'NONE', ( #25492 ), #21237, .F. ) ;
#15334 = VECTOR ( 'NONE', #11579, 1000.000000000000000 ) ;
#15335 = CARTESIAN_POINT ( 'NONE',  ( -10.90225941753887362, -16.78887681002774812, 20.25336174263950184 ) ) ;
#15336 = CARTESIAN_POINT ( 'NONE',  ( -8.499586724479453181, -2.959227181723774525, 21.50000000000000000 ) ) ;
#15337 = DIRECTION ( 'NONE',  ( 0.000000000000000000, 0.000000000000000000, -1.000000000000000000 ) ) ;
#15338 = CARTESIAN_POINT ( 'NONE',  ( 10.50949999207124641, -13.45141484214875227, 7.280727868105637768 ) ) ;
#15339 = CARTESIAN_POINT ( 'NONE',  ( -10.64374042650075403, -42.96126232887726815, -19.50000000000000355 ) ) ;
#15340 = CARTESIAN_POINT ( 'NONE',  ( -8.090471615930056259, 1.687027447297517080, 21.50000000000000000 ) ) ;
#15341 = CIRCLE ( 'NONE', #1901, 0.7500000000000006661 ) ;
#15342 = ORIENTED_EDGE ( 'NONE', *, *, #6695, .T. ) ;
#15343 = ORIENTED_EDGE ( 'NONE', *, *, #28350, .T. ) ;
#15344 = AXIS2_PLACEMENT_3D ( 'NONE', #5053, #11758, #30784 ) ;
#15345 = CARTESIAN_POINT ( 'NONE',  ( 3.808260130855334324E-15, -7.351593252548093815, -5.266666970006190773 ) ) ;
#15346 = CARTESIAN_POINT ( 'NONE',  ( 19.64114023396309960, -37.13592150529014191, -1.500000000000000000 ) ) ;
#15347 = CYLINDRICAL_SURFACE ( 'NONE', #14415, 0.7500000000000006661 ) ;
#15348 = CARTESIAN_POINT ( 'NONE',  ( -0.2028048457436513186, -17.02068360090467536, 6.385774490351131760 ) ) ;
#15349 = ORIENTED_EDGE ( 'NONE', *, *, #17671, .F. ) ;
#15350 = CARTESIAN_POINT ( 'NONE',  ( 35.76344986165623396, 22.29344514668041199, -19.50000000000000355 ) ) ;
#15351 = VECTOR ( 'NONE', #18851, 1000.000000000000000 ) ;
#15352 = ORIENTED_EDGE ( 'NONE', *, *, #25028, .F. ) ;
#15353 = LINE ( 'NONE', #24883, #30222 ) ;
#15354 = B_SPLINE_SURFACE_WITH_KNOTS ( 'NONE', 3, 1, ( 
 ( #20414, #18229 ),
 ( #4333, #28042 ),
 ( #27906, #4180 ),
 ( #30391, #25243 ),
 ( #13707, #13415 ),
 ( #13560, #3890 ),
 ( #1848, #15572 ),
 ( #3735, #6672 ),
 ( #23039, #27750 ),
 ( #18402, #11206 ),
 ( #13251, #25409 ),
 ( #8421, #25092 ),
 ( #6529, #16041 ),
 ( #20866, #9028 ),
 ( #8716, #18541 ),
 ( #22740, #25553 ),
 ( #1398, #22898 ),
 ( #25703, #8878 ),
 ( #15725, #20703 ),
 ( #4033, #16187 ),
 ( #6381, #6219 ),
 ( #13859, #23360 ),
 ( #29781, #15896 ),
 ( #10912, #10744 ),
 ( #20256, #17932 ),
 ( #8574, #30232 ),
 ( #18077, #27597 ),
 ( #1545, #11056 ),
 ( #20556, #30081 ),
 ( #2146, #23648 ),
 ( #16349, #2462 ),
 ( #4952, #25864 ),
 ( #26473, #16955 ),
 ( #18846, #23504 ) ),
 .UNSPECIFIED., .F., .F., .F.,
 ( 4, 2, 2, 2, 2, 2, 2, 2, 2, 2, 2, 2, 2, 2, 2, 2, 4 ),
 ( 2, 2 ),
 ( 0.000000000000000000, 0.06249999999999998612, 0.1249999999999999722, 0.1874999999999999445, 0.2499999999999999445, 0.3125000000000000000, 0.3750000000000000000, 0.4375000000000000000, 0.5000000000000000000, 0.5625000000000001110, 0.6250000000000001110, 0.6875000000000001110, 0.7500000000000000000, 0.8125000000000000000, 0.8750000000000000000, 0.9375000000000000000, 1.000000000000000000 ),
 ( 0.000000000000000000, 1.000000000000000000 ),
 .UNSPECIFIED. ) ;
#15355 = CIRCLE ( 'NONE', #14354, 1.000000000000007772 ) ;
#15356 = VECTOR ( 'NONE', #11976, 1000.000000000000000 ) ;
#15357 = DIRECTION ( 'NONE',  ( -0.000000000000000000, -0.000000000000000000, 1.000000000000000000 ) ) ;
#15358 = CARTESIAN_POINT ( 'NONE',  ( -38.81367831590564066, -4.342395794384154684, 32.17324057660533043 ) ) ;
#15359 = VERTEX_POINT ( 'NONE', #18932 ) ;
#15360 = LINE ( 'NONE', #17411, #19332 ) ;
#15361 = DIRECTION ( 'NONE',  ( 0.000000000000000000, 1.000000000000000000, 0.000000000000000000 ) ) ;
#15362 = VECTOR ( 'NONE', #21636, 1000.000000000000000 ) ;
#15363 = DIRECTION ( 'NONE',  ( 0.000000000000000000, 0.000000000000000000, 1.000000000000000000 ) ) ;
#15364 = VERTEX_POINT ( 'NONE', #2224 ) ;
#15365 = DIRECTION ( 'NONE',  ( -0.000000000000000000, -1.000000000000000000, -0.000000000000000000 ) ) ;
#15366 = CARTESIAN_POINT ( 'NONE',  ( 16.19239463133262191, -5.428304825921630439, 6.521906765011495466 ) ) ;
#15367 = CYLINDRICAL_SURFACE ( 'NONE', #28739, 32.32717498572581860 ) ;
#15368 = ADVANCED_FACE ( 'NONE', ( #15972 ), #20787, .F. ) ;
#15369 = CARTESIAN_POINT ( 'NONE',  ( -40.35775004261427767, 4.707207311767386493, -16.50000000000000711 ) ) ;
#15371 = ADVANCED_FACE ( 'NONE', ( #30459 ), #9102, .T. ) ;
#15370 = DIRECTION ( 'NONE',  ( 0.000000000000000000, 0.000000000000000000, 1.000000000000000000 ) ) ;
#15372 = CARTESIAN_POINT ( 'NONE',  ( 16.91972452348793610, -3.442972353390052920, -0.6213203435596476032 ) ) ;
#15373 = DIRECTION ( 'NONE',  ( 0.000000000000000000, 0.000000000000000000, 1.000000000000000000 ) ) ;
#15374 = ORIENTED_EDGE ( 'NONE', *, *, #24817, .T. ) ;
#15375 =( GEOMETRIC_REPRESENTATION_CONTEXT ( 3 ) GLOBAL_UNCERTAINTY_ASSIGNED_CONTEXT ( ( #13308 ) ) GLOBAL_UNIT_ASSIGNED_CONTEXT ( ( #10564, #30201, #6344 ) ) REPRESENTATION_CONTEXT ( 'NONE', 'WORKASPACE' ) );
#15376 = CARTESIAN_POINT ( 'NONE',  ( 0.000000000000000000, 87.00000000000001421, 15.49999999999998934 ) ) ;
#15377 = DIRECTION ( 'NONE',  ( 0.000000000000000000, 1.000000000000000000, 0.000000000000000000 ) ) ;
#15378 = VECTOR ( 'NONE', #9593, 1000.000000000000000 ) ;
#15379 = EDGE_LOOP ( 'NONE', ( #17152, #5200 ) ) ;
#15380 = AXIS2_PLACEMENT_3D ( 'NONE', #5498, #24512, #12986 ) ;
#15381 = ORIENTED_EDGE ( 'NONE', *, *, #28461, .T. ) ;
#15382 = CYLINDRICAL_SURFACE ( 'NONE', #3501, 9.482273699623480212 ) ;
#15383 = CARTESIAN_POINT ( 'NONE',  ( 13.22505861668195237, -42.10773672056998862, -19.50000000000000355 ) ) ;
#15384 = CARTESIAN_POINT ( 'NONE',  ( 5.130938270761610021, -7.974144905643803405, 1.500000000000001332 ) ) ;
#15385 = ORIENTED_EDGE ( 'NONE', *, *, #11161, .F. ) ;
#15386 = AXIS2_PLACEMENT_3D ( 'NONE', #10460, #3441, #14467 ) ;
#15387 = DIRECTION ( 'NONE',  ( -0.6548607339452852116, 0.7557495743542581579, 0.000000000000000000 ) ) ;
#15388 = CARTESIAN_POINT ( 'NONE',  ( -8.999114229549592281, 0.1262659238205133538, 21.50000000000000000 ) ) ;
#15389 = ORIENTED_EDGE ( 'NONE', *, *, #7482, .T. ) ;
#15390 = VERTEX_POINT ( 'NONE', #11913 ) ;
#15391 = CARTESIAN_POINT ( 'NONE',  ( -16.93532286002824705, 1.879651667671731641, 7.632642797338977658 ) ) ;
#15392 = CARTESIAN_POINT ( 'NONE',  ( 18.22972622987024138, -8.227512309863353579, 7.626647697317575414 ) ) ;
#15393 = CARTESIAN_POINT ( 'NONE',  ( -10.58794734610131805, -16.98849370068515086, 18.34969686940295830 ) ) ;
#15394 = CARTESIAN_POINT ( 'NONE',  ( -47.00000000000000000, 90.00000000000001421, 22.49999999999999289 ) ) ;
#15395 = ORIENTED_EDGE ( 'NONE', *, *, #13176, .T. ) ;
#15396 = DIRECTION ( 'NONE',  ( -0.000000000000000000, -0.000000000000000000, -1.000000000000000000 ) ) ;
#15397 = ORIENTED_EDGE ( 'NONE', *, *, #22763, .T. ) ;
#15398 = DIRECTION ( 'NONE',  ( 0.000000000000000000, -0.8660254037844380415, -0.5000000000000012212 ) ) ;
#15399 = CIRCLE ( 'NONE', #29356, 47.00000000000000000 ) ;
#15400 = ORIENTED_EDGE ( 'NONE', *, *, #10380, .T. ) ;
#15401 = DIRECTION ( 'NONE',  ( -0.000000000000000000, -0.000000000000000000, -1.000000000000000000 ) ) ;
#15402 = CARTESIAN_POINT ( 'NONE',  ( 23.63378365164496486, -33.81425525858435321, 29.65764705046944982 ) ) ;
#15403 = CARTESIAN_POINT ( 'NONE',  ( 16.61573067466907716, 3.902325345048613947, 7.366751648393900176 ) ) ;
#15404 = CARTESIAN_POINT ( 'NONE',  ( -14.94322542805485377, 13.31996107294430942, 18.55820869691756769 ) ) ;
#15405 = VECTOR ( 'NONE', #22293, 1000.000000000000000 ) ;
#15406 = CARTESIAN_POINT ( 'NONE',  ( -8.006961111548649868, -15.06991809617584366, 20.13759033520874908 ) ) ;
#15407 = CARTESIAN_POINT ( 'NONE',  ( -17.05006382470648418, 0.8465830297331881082, 19.96568007040467663 ) ) ;
#15408 = CARTESIAN_POINT ( 'NONE',  ( -17.01654212181476566, 1.203597991882925378, 18.44527579819791185 ) ) ;
#15409 = FACE_OUTER_BOUND ( 'NONE', #4199, .T. ) ;
#15410 = ORIENTED_EDGE ( 'NONE', *, *, #20633, .T. ) ;
#15411 = DIRECTION ( 'NONE',  ( -0.000000000000000000, -0.000000000000000000, -1.000000000000000000 ) ) ;
#15412 = B_SPLINE_CURVE_WITH_KNOTS ( 'NONE', 3,
 ( #13003, #13154, #23106, #29681, #5979, #24851, #22492, #15789, #27816, #6443, #22646, #25474, #13628, #3957, #3792, #1751, #30294, #1139, #8941, #5822, #15479, #15322, #1297, #10651, #25312, #22813, #20162, #17996, #10812, #27504, #20326, #29851, #1464, #6124, #10975, #20475, #25624, #19049, #9533, #28415, #26067, #4239, #16548, #12036, #30443, #13761, #2361, #4698 ),
 .UNSPECIFIED., .F., .F.,
 ( 4, 2, 2, 2, 2, 2, 2, 2, 2, 2, 2, 2, 2, 2, 2, 2, 2, 2, 2, 2, 2, 2, 2, 4 ),
 ( 0.04717002832140662627, 0.04864369486941700488, 0.05011736141742738349, 0.05306469451344814070, 0.05453836106145851931, 0.05601202760946889792, 0.05895936070548962737, 0.06043302725349997823, 0.06190669380151032214, 0.06485402689753103078, 0.06780135999355173249, 0.06927502654156207640, 0.07074869308957243419, 0.07369602618559310814, 0.07516969273360343817, 0.07664335928161378209, 0.07959069237763446991, 0.08253802547365514386, 0.08401169202166547390, 0.08548535856967581781, 0.08843269166569647788, 0.08990635821370680791, 0.09138002476171713795, 0.09432735785773779802 ),
 .UNSPECIFIED. ) ;
#15413 = AXIS2_PLACEMENT_3D ( 'NONE', #9044, #23520, #4511 ) ;
#15414 = DIRECTION ( 'NONE',  ( 1.000000000000000000, 0.000000000000000000, 0.000000000000000000 ) ) ;
#15415 = CARTESIAN_POINT ( 'NONE',  ( 25.64627119138473432, -23.40052582045089480, -16.50001200000000168 ) ) ;
#15416 = EDGE_LOOP ( 'NONE', ( #19705, #21657, #4826, #26246 ) ) ;
#15417 = VERTEX_POINT ( 'NONE', #30313 ) ;
#15418 = CARTESIAN_POINT ( 'NONE',  ( 48.92864595558773999, 69.97303745521041662, 17.94690505038828121 ) ) ;
#15419 = CARTESIAN_POINT ( 'NONE',  ( -7.106594496258223259, -4.390207617113929039, -1.500000000000002220 ) ) ;
#15420 = CARTESIAN_POINT ( 'NONE',  ( -4.997519263521718713, 19.38405562624022593, 6.641371103590088865 ) ) ;
#15421 = VERTEX_POINT ( 'NONE', #9556 ) ;
#15422 = CARTESIAN_POINT ( 'NONE',  ( 126.5359999999999872, 0.000000000000000000, 0.000000000000000000 ) ) ;
#15423 = FACE_OUTER_BOUND ( 'NONE', #16072, .T. ) ;
#15424 = CARTESIAN_POINT ( 'NONE',  ( 12.37236664230077743, -12.04390635323149716, 24.50000000000000000 ) ) ;
#15425 = VERTEX_POINT ( 'NONE', #18771 ) ;
#15426 = LINE ( 'NONE', #26998, #14725 ) ;
#15427 = CIRCLE ( 'NONE', #16412, 3.000000000000002665 ) ;
#15428 = FACE_OUTER_BOUND ( 'NONE', #29301, .T. ) ;
#15429 = CARTESIAN_POINT ( 'NONE',  ( 16.86202325244927636, 2.345734461008499583, 6.111214848085761986 ) ) ;
#15430 = VERTEX_POINT ( 'NONE', #23283 ) ;
#15431 = FACE_OUTER_BOUND ( 'NONE', #9997, .T. ) ;
#15432 = ORIENTED_EDGE ( 'NONE', *, *, #5741, .F. ) ;
#15433 = LINE ( 'NONE', #1568, #28370 ) ;
#15434 = CARTESIAN_POINT ( 'NONE',  ( 30.03865005752671991, -15.52610542268209848, 36.94359686637162099 ) ) ;
#15435 = B_SPLINE_CURVE_WITH_KNOTS ( 'NONE', 3,
 ( #27173, #24664, #12831, #971, #8150, #20458, #1887, #23233, #25452, #27636, #11411, #27944, #13137, #8611, #15614, #6259, #15772, #24977, #29831, #6421 ),
 .UNSPECIFIED., .F., .F.,
 ( 4, 2, 2, 2, 2, 2, 2, 2, 2, 4 ),
 ( 0.000000000000000000, 0.06249999999999958367, 0.1249999999999991673, 0.1874999999999987510, 0.2187499999999988065, 0.2499999999999988898, 0.3124999999999990563, 0.3749999999999991673, 0.4374999999999992784, 0.4999999999999994449 ),
 .UNSPECIFIED. ) ;
#15436 = VECTOR ( 'NONE', #9286, 1000.000000000000000 ) ;
#15437 = VERTEX_POINT ( 'NONE', #28131 ) ;
#15438 = ORIENTED_EDGE ( 'NONE', *, *, #9923, .T. ) ;
#15439 = ADVANCED_FACE ( 'NONE', ( #25642 ), #6464, .F. ) ;
#15440 = CARTESIAN_POINT ( 'NONE',  ( 3.111445993792399278, 16.79059500618347656, 6.341840715582230281 ) ) ;
#15441 = EDGE_CURVE ( 'NONE', #9025, #4691, #1924, .T. ) ;
#15442 = CARTESIAN_POINT ( 'NONE',  ( 16.47768670952434178, 14.41708049311048789, 1.500000000000000000 ) ) ;
#15443 = CARTESIAN_POINT ( 'NONE',  ( 49.99999999999998579, -70.00000000000000000, 12.49999999999999112 ) ) ;
#15444 = DIRECTION ( 'NONE',  ( 0.000000000000000000, -1.132880637372608986E-16, 1.000000000000000000 ) ) ;
#15445 = CARTESIAN_POINT ( 'NONE',  ( 9.864935476506834888, -13.90063640520463650, 18.34798005862930736 ) ) ;
#15446 = EDGE_CURVE ( 'NONE', #22212, #3020, #13933, .T. ) ;
#15447 = CARTESIAN_POINT ( 'NONE',  ( 19.82764810689592849, 2.754998275627143389, 20.25336174263950184 ) ) ;
#15448 = ORIENTED_EDGE ( 'NONE', *, *, #14946, .F. ) ;
#15449 = EDGE_CURVE ( 'NONE', #6070, #9872, #23431, .T. ) ;
#15450 = CARTESIAN_POINT ( 'NONE',  ( -19.71348387055304485, 3.477795851889710299, 19.56050940960062690 ) ) ;
#15451 = CARTESIAN_POINT ( 'NONE',  ( 15.51152286861890239, -7.023094163498096343, 7.359006845440219102 ) ) ;
#15452 = CIRCLE ( 'NONE', #2998, 9.084132297865673777 ) ;
#15453 = CARTESIAN_POINT ( 'NONE',  ( -13.83017030316320728, 10.00185174541443978, 20.06253562465620632 ) ) ;
#15454 = CARTESIAN_POINT ( 'NONE',  ( 42.73635331409263927, 67.00059091328013494, 62.14018542721996141 ) ) ;
#15455 = ORIENTED_EDGE ( 'NONE', *, *, #9602, .T. ) ;
#15456 = DIRECTION ( 'NONE',  ( 1.000000000000000000, 0.000000000000000000, 0.000000000000000000 ) ) ;
#15458 = EDGE_CURVE ( 'NONE', #20399, #9950, #9165, .T. ) ;
#15457 = CARTESIAN_POINT ( 'NONE',  ( -43.96625599154361197, 68.08820126035209341, 61.68658881044186870 ) ) ;
#15459 = CARTESIAN_POINT ( 'NONE',  ( -5.651831417317678685, 19.20339396603469240, 20.29090034784956131 ) ) ;
#15460 = CARTESIAN_POINT ( 'NONE',  ( -20.71335220384823117, -27.86167394782616213, -6.500000000000000888 ) ) ;
#15461 = CARTESIAN_POINT ( 'NONE',  ( -40.05520497409654013, 7.028746409781321702, -16.50000000000000000 ) ) ;
#15462 = EDGE_CURVE ( 'NONE', #8558, #27143, #7681, .T. ) ;
#15463 = DIRECTION ( 'NONE',  ( 1.000000000000000000, 0.000000000000000000, 0.000000000000000000 ) ) ;
#15464 = EDGE_CURVE ( 'NONE', #23060, #4164, #25936, .T. ) ;
#15465 = LINE ( 'NONE', #29518, #16390 ) ;
#15466 = ORIENTED_EDGE ( 'NONE', *, *, #8811, .T. ) ;
#15467 = CARTESIAN_POINT ( 'NONE',  ( -32.28307784207223108, -8.475829241206282560, 37.38016955275590902 ) ) ;
#15468 = ORIENTED_EDGE ( 'NONE', *, *, #20992, .F. ) ;
#15469 = DIRECTION ( 'NONE',  ( 0.000000000000000000, -1.132880637372608986E-16, 1.000000000000000000 ) ) ;
#15470 = LINE ( 'NONE', #27496, #19939 ) ;
#15471 = VERTEX_POINT ( 'NONE', #3428 ) ;
#15472 = ORIENTED_EDGE ( 'NONE', *, *, #11025, .F. ) ;
#15473 = DIRECTION ( 'NONE',  ( 0.000000000000000000, 0.000000000000000000, -1.000000000000000000 ) ) ;
#15474 = VECTOR ( 'NONE', #16199, 1000.000000000000000 ) ;
#15475 = CARTESIAN_POINT ( 'NONE',  ( -19.93487782419341769, 1.613472484145540120, 18.84486140012300126 ) ) ;
#15476 = ORIENTED_EDGE ( 'NONE', *, *, #26618, .T. ) ;
#15477 = DIRECTION ( 'NONE',  ( -0.000000000000000000, -0.000000000000000000, 1.000000000000000000 ) ) ;
#15478 = EDGE_CURVE ( 'NONE', #23438, #9760, #22112, .T. ) ;
#15479 = CARTESIAN_POINT ( 'NONE',  ( 14.51487557364575842, 47.84724665906151131, -58.90888295343145131 ) ) ;
#15480 = EDGE_CURVE ( 'NONE', #14242, #22916, #20625, .T. ) ;
#15481 = CYLINDRICAL_SURFACE ( 'NONE', #14980, 11.46182693247429718 ) ;
#15482 = ADVANCED_FACE ( 'NONE', ( #1248 ), #29160, .F. ) ;
#15483 = CARTESIAN_POINT ( 'NONE',  ( -37.39679457499870807, 12.06383856310230307, 10.63618240372393942 ) ) ;
#15484 = CYLINDRICAL_SURFACE ( 'NONE', #18815, 1.447898107987198646 ) ;
#15485 = EDGE_CURVE ( 'NONE', #29733, #886, #12793, .T. ) ;
#15486 = DIRECTION ( 'NONE',  ( 1.000000000000000000, 0.000000000000000000, 0.000000000000000000 ) ) ;
#15487 = CARTESIAN_POINT ( 'NONE',  ( -5.131244434206278626, -6.812559277181949646, -1.500000000000002665 ) ) ;
#15488 = CARTESIAN_POINT ( 'NONE',  ( 32.98805937973593672, 0.000000000000000000, 13.00000000000000178 ) ) ;
#15489 = CARTESIAN_POINT ( 'NONE',  ( -16.81926493917405807, 2.618766740933698323, 6.910395520694541105 ) ) ;
#15490 = VERTEX_POINT ( 'NONE', #19636 ) ;
#15491 = ADVANCED_FACE ( 'NONE', ( #15423 ), #22445, .F. ) ;
#15492 = CARTESIAN_POINT ( 'NONE',  ( -9.400432693290859731, -14.18986588558385264, 19.33715507985239412 ) ) ;
#15493 = CARTESIAN_POINT ( 'NONE',  ( -17.70591931088122806, -9.338465149306657054, 7.280727868105637768 ) ) ;
#15494 = ADVANCED_FACE ( 'NONE', ( #28587 ), #17308, .T. ) ;
#15495 = CARTESIAN_POINT ( 'NONE',  ( -6.393592071792283171, 18.96945647184856654, 7.559636331181775581 ) ) ;
#15496 = EDGE_CURVE ( 'NONE', #23725, #28435, #2710, .T. ) ;
#15497 = CARTESIAN_POINT ( 'NONE',  ( 32.74775157612609178, -27.21557300919356948, -19.50000000000000355 ) ) ;
#15498 = CIRCLE ( 'NONE', #6042, 0.7499999999999997780 ) ;
#15499 = CARTESIAN_POINT ( 'NONE',  ( -8.999114229549592281, 0.1262659238205133538, 21.50000000000000000 ) ) ;
#15500 = ORIENTED_EDGE ( 'NONE', *, *, #20200, .T. ) ;
#15501 = VERTEX_POINT ( 'NONE', #10604 ) ;
#15502 = CARTESIAN_POINT ( 'NONE',  ( 0.000000000000000000, 90.00000000000001421, 15.49999999999998934 ) ) ;
#15503 = CARTESIAN_POINT ( 'NONE',  ( 10.64374042650304020, -42.96126232887725394, -19.50000000000000355 ) ) ;
#15504 = CARTESIAN_POINT ( 'NONE',  ( -13.35701160122519404, 10.58771215013900502, 5.651989602109218858 ) ) ;
#15505 = DIRECTION ( 'NONE',  ( -1.000000000000000000, 0.000000000000000000, 0.000000000000000000 ) ) ;
#15506 = EDGE_LOOP ( 'NONE', ( #13833, #1787, #30685, #19461 ) ) ;
#15507 = CARTESIAN_POINT ( 'NONE',  ( -20.71335220384823117, 27.86167394782616213, -6.500000000000000888 ) ) ;
#15508 = CARTESIAN_POINT ( 'NONE',  ( 4.336808689942017736E-16, 42.50000000000000000, -1.500000000000000000 ) ) ;
#15509 = EDGE_CURVE ( 'NONE', #3904, #12729, #10679, .T. ) ;
#15510 = CARTESIAN_POINT ( 'NONE',  ( -9.085694127122231123, -14.40282604532832167, 7.429667576816606278 ) ) ;
#15511 = ADVANCED_FACE ( 'NONE', ( #26669 ), #20115, .F. ) ;
#15512 = ORIENTED_EDGE ( 'NONE', *, *, #7057, .T. ) ;
#15513 = AXIS2_PLACEMENT_3D ( 'NONE', #19535, #19680, #2693 ) ;
#15514 = ADVANCED_FACE ( 'NONE', ( #12491 ), #24790, .T. ) ;
#15515 = DIRECTION ( 'NONE',  ( 0.000000000000000000, 0.000000000000000000, -1.000000000000000000 ) ) ;
#15516 = CARTESIAN_POINT ( 'NONE',  ( 19.74251403343738076, 3.198927889078825970, 18.34798005863226678 ) ) ;
#15517 = EDGE_LOOP ( 'NONE', ( #24552, #22470, #14783, #30422 ) ) ;
#15518 = DIRECTION ( 'NONE',  ( -0.000000000000000000, -0.000000000000000000, 1.000000000000000000 ) ) ;
#15519 = DIRECTION ( 'NONE',  ( 1.000000000000000000, 0.000000000000000000, 0.000000000000000000 ) ) ;
#15520 = AXIS2_PLACEMENT_3D ( 'NONE', #2667, #14521, #25074 ) ;
#15521 = LINE ( 'NONE', #13194, #21805 ) ;
#15522 = FACE_OUTER_BOUND ( 'NONE', #13723, .T. ) ;
#15523 = EDGE_LOOP ( 'NONE', ( #9512, #26001, #25762, #5093 ) ) ;
#15524 = CARTESIAN_POINT ( 'NONE',  ( 24.14277784031759566, 13.29036922066994642, 43.19821070588412226 ) ) ;
#15525 = DIRECTION ( 'NONE',  ( 0.000000000000000000, 0.000000000000000000, 1.000000000000000000 ) ) ;
#15526 = DIRECTION ( 'NONE',  ( 0.000000000000000000, 1.132880637372608986E-16, -1.000000000000000000 ) ) ;
#15527 = B_SPLINE_CURVE_WITH_KNOTS ( 'NONE', 3,
 ( #29566, #8199, #5858, #10685, #7903, #7743, #3527, #26773, #29715, #22531, #8361, #17877, #26930, #15049, #20654, #27990, #30176, #25346 ),
 .UNSPECIFIED., .F., .F.,
 ( 4, 2, 2, 2, 2, 2, 2, 2, 4 ),
 ( 0.000000000000000000, 0.0003967869494442896193, 0.0007935738988885792386, 0.001190360848332868912, 0.001587147797777158477, 0.001983934747221448042, 0.002380721696665737824, 0.002777508646110027173, 0.003174295595554316955 ),
 .UNSPECIFIED. ) ;
#15528 = CARTESIAN_POINT ( 'NONE',  ( -50.00000000000000000, 70.00000000000000000, 22.49999999999999289 ) ) ;
#15529 = LINE ( 'NONE', #20056, #19227 ) ;
#15530 = CARTESIAN_POINT ( 'NONE',  ( 12.72536390617885438, -2.839914339433650348, 1.500000000000001332 ) ) ;
#15531 = LINE ( 'NONE', #11170, #28442 ) ;
#15532 = DIRECTION ( 'NONE',  ( 1.000000000000000000, 0.000000000000000000, 0.000000000000000000 ) ) ;
#15533 = ORIENTED_EDGE ( 'NONE', *, *, #11907, .T. ) ;
#15534 = AXIS2_PLACEMENT_3D ( 'NONE', #6906, #14213, #16260 ) ;
#15535 = CARTESIAN_POINT ( 'NONE',  ( -0.8762659238204844048, -8.999114229549588728, 21.50000000000000000 ) ) ;
#15536 = DIRECTION ( 'NONE',  ( 0.000000000000000000, 0.000000000000000000, 1.000000000000000000 ) ) ;
#15537 = DIRECTION ( 'NONE',  ( 1.000000000000000000, 0.000000000000000000, 0.000000000000000000 ) ) ;
#15538 = ORIENTED_EDGE ( 'NONE', *, *, #9965, .F. ) ;
#15539 = EDGE_LOOP ( 'NONE', ( #1197, #16089, #5210 ) ) ;
#15540 = DIRECTION ( 'NONE',  ( 0.000000000000000000, 0.000000000000000000, 1.000000000000000000 ) ) ;
#15541 = CYLINDRICAL_SURFACE ( 'NONE', #698, 20.00000000000000000 ) ;
#15542 = FACE_OUTER_BOUND ( 'NONE', #3664, .T. ) ;
#15543 = ORIENTED_EDGE ( 'NONE', *, *, #11839, .T. ) ;
#15544 = AXIS2_PLACEMENT_3D ( 'NONE', #1830, #9010, #11355 ) ;
#15545 = CARTESIAN_POINT ( 'NONE',  ( -6.315055774950723233, 15.86014940731417866, 18.73314399819311760 ) ) ;
#15546 = CARTESIAN_POINT ( 'NONE',  ( 9.013259606647444855, -14.43917691232923417, 19.47784884541372818 ) ) ;
#15547 = EDGE_CURVE ( 'NONE', #25953, #4649, #29116, .T. ) ;
#15548 = ORIENTED_EDGE ( 'NONE', *, *, #11644, .F. ) ;
#15549 = ORIENTED_EDGE ( 'NONE', *, *, #6192, .T. ) ;
#15550 = DIRECTION ( 'NONE',  ( -0.000000000000000000, -1.000000000000000000, -0.000000000000000000 ) ) ;
#15551 = DIRECTION ( 'NONE',  ( 1.000000000000000000, 0.000000000000000000, 0.000000000000000000 ) ) ;
#15552 = CARTESIAN_POINT ( 'NONE',  ( -25.47847050916411504, 26.57182937991348481, 1.500000000000001332 ) ) ;
#15553 = CARTESIAN_POINT ( 'NONE',  ( -12.58753388439931165, 40.25309894602420258, 34.56092818870066452 ) ) ;
#15554 = ORIENTED_EDGE ( 'NONE', *, *, #26543, .T. ) ;
#15555 = LINE ( 'NONE', #20231, #4882 ) ;
#15556 = ORIENTED_EDGE ( 'NONE', *, *, #25410, .T. ) ;
#15557 = AXIS2_PLACEMENT_3D ( 'NONE', #18922, #6601, #14063 ) ;
#15558 = LINE ( 'NONE', #776, #13044 ) ;
#15559 = CARTESIAN_POINT ( 'NONE',  ( -16.81857544482621236, 2.623036418782660473, 19.08155846658118904 ) ) ;
#15560 = VERTEX_POINT ( 'NONE', #19963 ) ;
#15561 = CARTESIAN_POINT ( 'NONE',  ( -40.00000000000000000, -0.000000000000000000, 62.49999999999999289 ) ) ;
#15562 = FACE_OUTER_BOUND ( 'NONE', #5566, .T. ) ;
#15563 = CARTESIAN_POINT ( 'NONE',  ( 16.73033351903584887, 3.274018421667482137, 5.652605728828373977 ) ) ;
#15564 = CARTESIAN_POINT ( 'NONE',  ( 37.16608720827707657, -51.86186943028246787, 97.07879600563551037 ) ) ;
#15565 = CARTESIAN_POINT ( 'NONE',  ( -7.692543755867210287, -15.24678548464671124, 19.58863275299554019 ) ) ;
#15566 = DIRECTION ( 'NONE',  ( -0.000000000000000000, 1.132880637372608986E-16, -1.000000000000000000 ) ) ;
#15567 = LINE ( 'NONE', #8250, #23456 ) ;
#15568 = CYLINDRICAL_SURFACE ( 'NONE', #28311, 2.898871837527149165 ) ;
#15569 = EDGE_LOOP ( 'NONE', ( #12216, #19669, #27989, #19683 ) ) ;
#15570 = CARTESIAN_POINT ( 'NONE',  ( -8.074094344234884818E-15, 42.50000000000000000, 19.72227980406325543 ) ) ;
#15571 = CARTESIAN_POINT ( 'NONE',  ( -30.29234184432961996, 26.77155622317955164, 17.22256730531661262 ) ) ;
#15572 = CARTESIAN_POINT ( 'NONE',  ( 17.94248964168179583, -34.33858135081684537, 27.49999999999999645 ) ) ;
#15573 = ORIENTED_EDGE ( 'NONE', *, *, #25413, .T. ) ;
#15574 = ORIENTED_EDGE ( 'NONE', *, *, #25043, .T. ) ;
#15575 = CARTESIAN_POINT ( 'NONE',  ( 47.81953956977370979, 69.88199567761851938, 16.25762515829667976 ) ) ;
#15576 = AXIS2_PLACEMENT_3D ( 'NONE', #1484, #8348, #15505 ) ;
#15577 = AXIS2_PLACEMENT_3D ( 'NONE', #11999, #21491, #6696 ) ;
#15578 = DIRECTION ( 'NONE',  ( -0.000000000000000000, -0.000000000000000000, -1.000000000000000000 ) ) ;
#15579 = AXIS2_PLACEMENT_3D ( 'NONE', #25051, #22861, #15537 ) ;
#15580 = CARTESIAN_POINT ( 'NONE',  ( -5.048943207435892866, 19.37072948160042074, 6.974106381145714018 ) ) ;
#15581 = VERTEX_POINT ( 'NONE', #8266 ) ;
#15582 = CARTESIAN_POINT ( 'NONE',  ( 0.000000000000000000, 0.000000000000000000, 1.500000000000000000 ) ) ;
#15583 = CARTESIAN_POINT ( 'NONE',  ( -29.61203839202723032, 15.40012917324033204, 41.62281023987520001 ) ) ;
#15584 = FACE_OUTER_BOUND ( 'NONE', #7940, .T. ) ;
#15585 = ORIENTED_EDGE ( 'NONE', *, *, #23501, .T. ) ;
#15586 = FACE_OUTER_BOUND ( 'NONE', #1963, .T. ) ;
#15587 = CARTESIAN_POINT ( 'NONE',  ( 12.25310179107605890, 11.85582831497230671, 5.661398277488801867 ) ) ;
#15588 = CARTESIAN_POINT ( 'NONE',  ( 16.87674189766845956, 2.217009531549524848, 6.864725433338323413 ) ) ;
#15589 = VERTEX_POINT ( 'NONE', #613 ) ;
#15590 = CARTESIAN_POINT ( 'NONE',  ( 15.04472583903953975, 13.20536594261729491, 5.670038381137163519 ) ) ;
#15591 = ORIENTED_EDGE ( 'NONE', *, *, #28196, .F. ) ;
#15592 = CARTESIAN_POINT ( 'NONE',  ( 0.000000000000000000, 0.000000000000000000, 1.500000000000001332 ) ) ;
#15593 = ORIENTED_EDGE ( 'NONE', *, *, #7287, .T. ) ;
#15594 = VERTEX_POINT ( 'NONE', #26839 ) ;
#15595 = CIRCLE ( 'NONE', #3138, 0.7499999999999988898 ) ;
#15596 = FACE_OUTER_BOUND ( 'NONE', #7978, .T. ) ;
#15597 = CIRCLE ( 'NONE', #1155, 9.000000000000000000 ) ;
#15598 = DIRECTION ( 'NONE',  ( 0.000000000000000000, 1.000000000000000000, 0.000000000000000000 ) ) ;
#15599 = CARTESIAN_POINT ( 'NONE',  ( -38.00000000000000711, 80.00000000000001421, 50.49999999999998579 ) ) ;
#15600 = ORIENTED_EDGE ( 'NONE', *, *, #26727, .F. ) ;
#15601 = CARTESIAN_POINT ( 'NONE',  ( -15.85884089648730644, -35.55173462727348266, 34.80090346875803675 ) ) ;
#15602 = CARTESIAN_POINT ( 'NONE',  ( 9.054000795813630376, -14.41483084819681260, 19.00652017443069752 ) ) ;
#15603 = CARTESIAN_POINT ( 'NONE',  ( -6.414842543015754295, -17.06554576617236307, 1.500000000000000000 ) ) ;
#15604 = ORIENTED_EDGE ( 'NONE', *, *, #20656, .F. ) ;
#15605 = CARTESIAN_POINT ( 'NONE',  ( 7.488956955540400529, 5.141690706682902068, -1.500000000000001110 ) ) ;
#15606 = CARTESIAN_POINT ( 'NONE',  ( 15.63429980755321935, -6.761683097800861297, 5.749228751562096562 ) ) ;
#15607 = CARTESIAN_POINT ( 'NONE',  ( -13.83904721019127848, 9.990416291640219271, 5.951255046771932733 ) ) ;
#15608 = CARTESIAN_POINT ( 'NONE',  ( 3.111445993792395281, 16.79059500618346945, 19.03762469184452755 ) ) ;
#15609 = EDGE_LOOP ( 'NONE', ( #17622, #18468, #2357, #9269, #5969, #18195 ) ) ;
#15610 = ORIENTED_EDGE ( 'NONE', *, *, #17204, .T. ) ;
#15611 = LINE ( 'NONE', #6256, #27273 ) ;
#15612 = CARTESIAN_POINT ( 'NONE',  ( 10.29773160334160131, -13.60426929931266038, 5.759928666072751113 ) ) ;
#15613 = B_SPLINE_SURFACE_WITH_KNOTS ( 'NONE', 3, 1, ( 
 ( #15890, #17758 ),
 ( #8569, #15719 ),
 ( #6215, #29932 ),
 ( #27591, #18395 ),
 ( #27276, #25237 ),
 ( #5909, #15408 ),
 ( #10738, #3884 ),
 ( #20248, #29774 ),
 ( #8415, #13409 ),
 ( #22893, #1541 ),
 ( #11051, #13555 ),
 ( #23035, #1685 ),
 ( #11201, #18534 ),
 ( #26312, #11975 ),
 ( #28039, #21468 ),
 ( #18679, #6667 ),
 ( #7285, #25699 ),
 ( #21002, #20859 ),
 ( #16183, #28186 ),
 ( #30832, #2287 ),
 ( #109, #4327 ),
 ( #9629, #7137 ),
 ( #6817, #16493 ),
 ( #9478, #23643 ),
 ( #13854, #11658 ),
 ( #23497, #2141 ),
 ( #25859, #21312 ),
 ( #13703, #23355 ),
 ( #4491, #2457 ),
 ( #11809, #14289 ),
 ( #1994, #28359 ) ),
 .UNSPECIFIED., .F., .F., .F.,
 ( 4, 3, 3, 3, 3, 3, 3, 3, 3, 3, 4 ),
 ( 2, 2 ),
 ( 0.4999999998345687757, 0.5360336730431939367, 0.5907651151589012883, 0.6456034593241830599, 0.6998270958050434309, 0.7529536536315937223, 0.8052385063053260073, 0.8575343587103997356, 0.9106564858195042023, 0.9648414833209685293, 1.000000006602610014 ),
 ( 0.000000000000000000, 1.000000000000000000 ),
 .UNSPECIFIED. ) ;
#15614 = CARTESIAN_POINT ( 'NONE',  ( 12.88304655974325108, 11.13107787108148550, 6.031926333436654630 ) ) ;
#15615 = CIRCLE ( 'NONE', #2166, 0.7500000000000006661 ) ;
#15616 = DIRECTION ( 'NONE',  ( 1.000000000000000000, 0.000000000000000000, 0.000000000000000000 ) ) ;
#15617 = EDGE_CURVE ( 'NONE', #7784, #28377, #28605, .T. ) ;
#15618 = CARTESIAN_POINT ( 'NONE',  ( -0.1262659238204836554, -8.999114229549588728, 1.500000000000001332 ) ) ;
#15619 = AXIS2_PLACEMENT_3D ( 'NONE', #19632, #21980, #26666 ) ;
#15620 = CARTESIAN_POINT ( 'NONE',  ( -24.03057240117690441, -26.57182937991348481, -6.499999999999999112 ) ) ;
#15621 = B_SPLINE_CURVE_WITH_KNOTS ( 'NONE', 3,
 ( #25898, #4683, #4529, #6572, #21192, #13607 ),
 .UNSPECIFIED., .F., .F.,
 ( 4, 2, 4 ),
 ( 0.003121276445852156928, 0.003498170197137229383, 0.003875063948422301837 ),
 .UNSPECIFIED. ) ;
#15622 = CIRCLE ( 'NONE', #29077, 0.7499999999999988898 ) ;
#15623 = ORIENTED_EDGE ( 'NONE', *, *, #19319, .T. ) ;
#15624 = DIRECTION ( 'NONE',  ( -1.000000000000000000, 0.000000000000000000, 0.000000000000000000 ) ) ;
#15625 = DIRECTION ( 'NONE',  ( 0.000000000000000000, 1.000000000000000000, 0.000000000000000000 ) ) ;
#15626 = DIRECTION ( 'NONE',  ( 0.000000000000000000, 0.000000000000000000, -1.000000000000000000 ) ) ;
#15627 = VERTEX_POINT ( 'NONE', #761 ) ;
#15628 = EDGE_LOOP ( 'NONE', ( #2987, #2143, #23505, #4055 ) ) ;
#15629 = CARTESIAN_POINT ( 'NONE',  ( -8.072557715923444732, 14.41080185948837311, 1.500000000000000000 ) ) ;
#15630 = EDGE_CURVE ( 'NONE', #28141, #18363, #7967, .T. ) ;
#15631 = CARTESIAN_POINT ( 'NONE',  ( -19.84344116185556217, 2.497567387674351824, 20.34789198813115263 ) ) ;
#15632 = VERTEX_POINT ( 'NONE', #5622 ) ;
#15633 = DIRECTION ( 'NONE',  ( 0.000000000000000000, 0.000000000000000000, 1.000000000000000000 ) ) ;
#15634 = PLANE ( 'NONE',  #5827 ) ;
#15635 = DIRECTION ( 'NONE',  ( 0.000000000000000000, 0.000000000000000000, 1.000000000000000000 ) ) ;
#15636 = DIRECTION ( 'NONE',  ( 0.000000000000000000, -0.000000000000000000, -1.000000000000000000 ) ) ;
#15637 = DIRECTION ( 'NONE',  ( 0.000000000000000000, 0.000000000000000000, 1.000000000000000000 ) ) ;
#15638 = EDGE_CURVE ( 'NONE', #9325, #12261, #15114, .T. ) ;
#15639 = AXIS2_PLACEMENT_3D ( 'NONE', #10209, #23938, #24239 ) ;
#15640 = DIRECTION ( 'NONE',  ( -0.2972711322815276280, -0.9547931052914334638, 0.000000000000000000 ) ) ;
#15641 = CARTESIAN_POINT ( 'NONE',  ( 1.139261986572422281, -19.98520933375988662, 7.280727868105637768 ) ) ;
#15642 = CARTESIAN_POINT ( 'NONE',  ( -0.1262659238204836554, -8.999114229549588728, 1.500000000000001332 ) ) ;
#15643 = ORIENTED_EDGE ( 'NONE', *, *, #28270, .T. ) ;
#15644 = CARTESIAN_POINT ( 'NONE',  ( -11.32740345151500172, -16.50481001894685917, 19.00652017443069752 ) ) ;
#15645 = CARTESIAN_POINT ( 'NONE',  ( -14.73262409220166269, -8.633676228711859579, 6.995624166085161910 ) ) ;
#15646 = CARTESIAN_POINT ( 'NONE',  ( 33.16313691975489064, 0.000000000000000000, -1.500000000000000000 ) ) ;
#15647 = CARTESIAN_POINT ( 'NONE',  ( -14.71031647956046129, -8.675071222119056458, 19.14333282897057842 ) ) ;
#15648 = CARTESIAN_POINT ( 'NONE',  ( 49.99999999999998579, -50.00000000000000000, 12.49999999999999112 ) ) ;
#15649 = CARTESIAN_POINT ( 'NONE',  ( -33.51206231511395117, 9.871883628028006896, 35.82171084650917692 ) ) ;
#15650 = ORIENTED_EDGE ( 'NONE', *, *, #25197, .F. ) ;
#15651 = ORIENTED_EDGE ( 'NONE', *, *, #6937, .T. ) ;
#15652 = CARTESIAN_POINT ( 'NONE',  ( -29.81954908927653136, 15.48017614753372051, 37.15913391342354544 ) ) ;
#15653 = CARTESIAN_POINT ( 'NONE',  ( -20.65888525914364493, -38.75220717792906555, -19.50000000000000355 ) ) ;
#15654 = EDGE_CURVE ( 'NONE', #2838, #25122, #20143, .T. ) ;
#15655 = CARTESIAN_POINT ( 'NONE',  ( -15.28428954155913644, 12.92682542062230944, 5.657991946698900598 ) ) ;
#15656 = EDGE_CURVE ( 'NONE', #6824, #6045, #7198, .T. ) ;
#15657 = CARTESIAN_POINT ( 'NONE',  ( -15.57266529552203416, 38.96488032230103471, -1.500000000000000000 ) ) ;
#15658 = ORIENTED_EDGE ( 'NONE', *, *, #17908, .F. ) ;
#15659 = CARTESIAN_POINT ( 'NONE',  ( 34.07766914600081520, 21.40380666527109810, -1.500000000000000000 ) ) ;
#15660 = CARTESIAN_POINT ( 'NONE',  ( -10.89423172471906476, -16.79374140667819759, 5.749228751562096562 ) ) ;
#15661 = VECTOR ( 'NONE', #4042, 1000.000000000000000 ) ;
#15662 = ORIENTED_EDGE ( 'NONE', *, *, #20999, .T. ) ;
#15663 = EDGE_CURVE ( 'NONE', #27328, #1692, #29791, .T. ) ;
#15664 = CARTESIAN_POINT ( 'NONE',  ( -52.16608720827707657, 51.86186943028246787, 57.49999999999999289 ) ) ;
#15665 = CARTESIAN_POINT ( 'NONE',  ( -9.920192004040607969, -41.10915752540522305, 28.96131254832305757 ) ) ;
#15666 = VERTEX_POINT ( 'NONE', #6072 ) ;
#15667 = EDGE_CURVE ( 'NONE', #12057, #13747, #30089, .T. ) ;
#15668 = CYLINDRICAL_SURFACE ( 'NONE', #20340, 9.482273699623480212 ) ;
#15669 = EDGE_CURVE ( 'NONE', #17963, #18819, #10917, .T. ) ;
#15670 = FACE_OUTER_BOUND ( 'NONE', #5889, .T. ) ;
#15671 = CARTESIAN_POINT ( 'NONE',  ( -16.46198811862381817, -1.356593340923033075, 24.50000000000000000 ) ) ;
#15672 = VERTEX_POINT ( 'NONE', #30398 ) ;
#15673 = CARTESIAN_POINT ( 'NONE',  ( 9.169883732660084164, -9.268939115642975679, 24.50000000000000000 ) ) ;
#15674 = EDGE_CURVE ( 'NONE', #22154, #18657, #27605, .T. ) ;
#15675 = B_SPLINE_CURVE_WITH_KNOTS ( 'NONE', 3,
 ( #15265, #25106, #24636, #27610, #16167, #10929, #20271, #13266, #1413, #22298, #10608 ),
 .UNSPECIFIED., .F., .F.,
 ( 4, 1, 1, 1, 1, 1, 1, 1, 4 ),
 ( 0.000000000000000000, 0.3926990816987241395, 0.7853981633974482790, 1.178097245096172418, 1.570796326794896558, 1.963495408493620475, 2.356194490192344837, 2.748893571891068976, 3.141592653589793116 ),
 .UNSPECIFIED. ) ;
#15676 = CARTESIAN_POINT ( 'NONE',  ( 32.14095006730908466, 14.40137518142634399, 35.53782825234915066 ) ) ;
#15677 = DIRECTION ( 'NONE',  ( 0.5406408174555976665, -0.8412535328311810945, -0.000000000000000000 ) ) ;
#15678 = CARTESIAN_POINT ( 'NONE',  ( -19.91398265452221850, -1.852915226174651986, 24.50000000000000000 ) ) ;
#15679 = DIRECTION ( 'NONE',  ( 0.000000000000000000, 1.000000000000000000, 1.132880637372608986E-16 ) ) ;
#15680 = AXIS2_PLACEMENT_3D ( 'NONE', #26451, #5081, #14592 ) ;
#15681 = DIRECTION ( 'NONE',  ( 0.4495526574063634095, -0.8932538319083086487, 0.000000000000000000 ) ) ;
#15682 = CARTESIAN_POINT ( 'NONE',  ( -7.974144905643822945, -5.130938270761581599, 1.500000000000001332 ) ) ;
#15683 = CARTESIAN_POINT ( 'NONE',  ( 9.752055262503102284, -13.97602916338938250, 7.652108011868852699 ) ) ;
#15684 = CARTESIAN_POINT ( 'NONE',  ( 35.46011056729525279, -7.038057716375242023, 34.64849135038199535 ) ) ;
#15685 = CARTESIAN_POINT ( 'NONE',  ( -5.141690706682823020, 7.488956955540454707, -1.500000000000000888 ) ) ;
#15686 = VERTEX_POINT ( 'NONE', #13713 ) ;
#15687 = ORIENTED_EDGE ( 'NONE', *, *, #19872, .F. ) ;
#15688 = CARTESIAN_POINT ( 'NONE',  ( -37.99999999999999289, 90.00000000000001421, -22.50000000000001421 ) ) ;
#15689 = DIRECTION ( 'NONE',  ( 1.000000000000000000, 0.000000000000000000, 0.000000000000000000 ) ) ;
#15690 = EDGE_CURVE ( 'NONE', #6045, #28904, #25100, .T. ) ;
#15691 = DIRECTION ( 'NONE',  ( 0.000000000000000000, 0.000000000000000000, -1.000000000000000000 ) ) ;
#15692 = EDGE_CURVE ( 'NONE', #25420, #4539, #13568, .T. ) ;
#15693 = VERTEX_POINT ( 'NONE', #22750 ) ;
#15694 = FACE_OUTER_BOUND ( 'NONE', #5819, .T. ) ;
#15695 = EDGE_CURVE ( 'NONE', #29091, #8467, #19637, .T. ) ;
#15696 = DIRECTION ( 'NONE',  ( 1.000000000000000000, 0.000000000000000000, -0.000000000000000000 ) ) ;
#15697 = ORIENTED_EDGE ( 'NONE', *, *, #16607, .T. ) ;
#15698 = ORIENTED_EDGE ( 'NONE', *, *, #21608, .T. ) ;
#15699 = B_SPLINE_CURVE_WITH_KNOTS ( 'NONE', 3,
 ( #18132, #22637, #13469, #8314, #1604, #6267, #27346, #17829, #27495, #5971, #20465, #13304, #29843, #15311, #1288, #1455 ),
 .UNSPECIFIED., .F., .F.,
 ( 4, 2, 2, 2, 2, 2, 2, 4 ),
 ( 2.980251112119010967E-07, 0.0009280375473568674505, 0.001391907308479688144, 0.001855777069602508947, 0.002319646830725329966, 0.002783516591848150552, 0.003247386352970971137, 0.003711256114093792156 ),
 .UNSPECIFIED. ) ;
#15700 = CARTESIAN_POINT ( 'NONE',  ( -19.77235582619724141, 3.126546698941333080, 5.862424720655265098 ) ) ;
#15701 = CARTESIAN_POINT ( 'NONE',  ( -30.74147208807243814, -15.49548351932574697, 36.33144972441046150 ) ) ;
#15702 = CARTESIAN_POINT ( 'NONE',  ( -8.738547258790619665, -14.62818084867463142, 18.36582235739946611 ) ) ;
#15703 = CARTESIAN_POINT ( 'NONE',  ( -16.58443505991521150, 38.47295314005269518, 29.20253828648597505 ) ) ;
#15704 = ORIENTED_EDGE ( 'NONE', *, *, #14166, .F. ) ;
#15705 = CARTESIAN_POINT ( 'NONE',  ( -24.03057240117691862, -26.57182937991349903, -1.500000000000000000 ) ) ;
#15706 = VECTOR ( 'NONE', #15120, 1000.000000000000000 ) ;
#15707 = ORIENTED_EDGE ( 'NONE', *, *, #27710, .T. ) ;
#15708 = EDGE_CURVE ( 'NONE', #4843, #16773, #6208, .T. ) ;
#15709 = CARTESIAN_POINT ( 'NONE',  ( 27.03074382657074537, -6.449748410230991880, 47.21042702067962438 ) ) ;
#15710 = DIRECTION ( 'NONE',  ( 0.000000000000000000, 0.5000000000000012212, -0.8660254037844380415 ) ) ;
#15711 = EDGE_LOOP ( 'NONE', ( #25554, #7156 ) ) ;
#15712 = LINE ( 'NONE', #909, #29666 ) ;
#15713 = CARTESIAN_POINT ( 'NONE',  ( 10.13012925513353579, -41.06507652560424049, 28.96509805317834463 ) ) ;
#15714 = CARTESIAN_POINT ( 'NONE',  ( 19.57334175050933212, 4.193940174973930013, 6.672349528511551497 ) ) ;
#15715 = CARTESIAN_POINT ( 'NONE',  ( 28.34828976096172681, -29.18752572968383419, 1.500000000000000000 ) ) ;
#15716 = CIRCLE ( 'NONE', #30713, 5.000000000000004441 ) ;
#15717 = CARTESIAN_POINT ( 'NONE',  ( -9.983339604393954403, -17.35078046477760694, 20.13759033520874908 ) ) ;
#15718 = FACE_OUTER_BOUND ( 'NONE', #10936, .T. ) ;
#15719 = CARTESIAN_POINT ( 'NONE',  ( -16.97503503882429854, 1.572081968053589351, 18.34838970509067479 ) ) ;
#15720 = FACE_BOUND ( 'NONE', #15832, .T. ) ;
#15721 = ORIENTED_EDGE ( 'NONE', *, *, #1983, .T. ) ;
#15722 = ADVANCED_FACE ( 'NONE', ( #25710 ), #4340, .F. ) ;
#15723 = EDGE_CURVE ( 'NONE', #4543, #23230, #29132, .T. ) ;
#15724 = CARTESIAN_POINT ( 'NONE',  ( 11.94785300146925699, -16.06093515404948846, 19.25672174529527325 ) ) ;
#15725 = CARTESIAN_POINT ( 'NONE',  ( 35.76481447503399380, 5.202797454133643917, 34.80090346875810070 ) ) ;
#15726 = EDGE_LOOP ( 'NONE', ( #4335, #19932, #24501, #11211, #22872, #1133 ) ) ;
#15727 = ORIENTED_EDGE ( 'NONE', *, *, #10922, .T. ) ;
#15728 = AXIS2_PLACEMENT_3D ( 'NONE', #14901, #5240, #14738 ) ;
#15729 = CARTESIAN_POINT ( 'NONE',  ( -27.03074382657074537, 6.449748410230988327, -16.55003854064094426 ) ) ;
#15730 = CARTESIAN_POINT ( 'NONE',  ( 11.64054540341803978, 16.26338533980433709, 24.50000000000000000 ) ) ;
#15731 = CARTESIAN_POINT ( 'NONE',  ( -5.475907499891255803, 16.13963752243575200, 5.653912893140659257 ) ) ;
#15732 = ORIENTED_EDGE ( 'NONE', *, *, #6683, .T. ) ;
#15733 = CARTESIAN_POINT ( 'NONE',  ( -40.00000000000000000, 87.00000000000001421, 12.49999999999999112 ) ) ;
#15734 = AXIS2_PLACEMENT_3D ( 'NONE', #25443, #20295, #22931 ) ;
#15735 = CARTESIAN_POINT ( 'NONE',  ( -12.71180423606275767, 11.31964500333552692, 6.714907520933424578 ) ) ;
#15736 = FACE_OUTER_BOUND ( 'NONE', #14974, .T. ) ;
#15737 = ORIENTED_EDGE ( 'NONE', *, *, #19894, .F. ) ;
#15738 = DIRECTION ( 'NONE',  ( 1.000000000000000000, 0.000000000000000000, -0.000000000000000000 ) ) ;
#15739 = VECTOR ( 'NONE', #29388, 1000.000000000000000 ) ;
#15740 = PLANE ( 'NONE',  #16968 ) ;
#15741 = ORIENTED_EDGE ( 'NONE', *, *, #16800, .T. ) ;
#15742 = DIRECTION ( 'NONE',  ( 1.000000000000000000, 0.000000000000000000, 0.000000000000000000 ) ) ;
#15743 = EDGE_LOOP ( 'NONE', ( #5215, #24365, #7335, #7193, #26723, #16037 ) ) ;
#15744 = CARTESIAN_POINT ( 'NONE',  ( -13.54809176563293427, 10.35918576916548695, 20.34789198813115618 ) ) ;
#15745 = PRODUCT_DEFINITION_CONTEXT ( 'detailed design', #25330, 'design' ) ;
#15746 = ORIENTED_EDGE ( 'NONE', *, *, #27865, .T. ) ;
#15747 = ORIENTED_EDGE ( 'NONE', *, *, #1783, .T. ) ;
#15748 = VECTOR ( 'NONE', #1544, 1000.000000000000000 ) ;
#15749 = CARTESIAN_POINT ( 'NONE',  ( 3.352743984114611830, 16.73528478182341672, 7.366751648393900176 ) ) ;
#15750 = AXIS2_PLACEMENT_3D ( 'NONE', #8635, #8328, #11271 ) ;
#15751 = DIRECTION ( 'NONE',  ( 0.000000000000000000, 0.000000000000000000, 1.000000000000000000 ) ) ;
#15752 = DIRECTION ( 'NONE',  ( 0.000000000000000000, 0.000000000000000000, 1.000000000000000000 ) ) ;
#15753 = ORIENTED_EDGE ( 'NONE', *, *, #22707, .F. ) ;
#15754 = AXIS2_PLACEMENT_3D ( 'NONE', #22912, #1561, #20569 ) ;
#15755 = CARTESIAN_POINT ( 'NONE',  ( -2.338573377552017440, -39.49999999999999289, 27.49999999999999645 ) ) ;
#15756 = CARTESIAN_POINT ( 'NONE',  ( 10.34995923732865108, -17.13460031806512873, 18.90679857307105749 ) ) ;
#15757 = DIRECTION ( 'NONE',  ( -1.000000000000000000, 0.000000000000000000, -0.000000000000000000 ) ) ;
#15758 = ORIENTED_EDGE ( 'NONE', *, *, #8843, .F. ) ;
#15759 = FACE_OUTER_BOUND ( 'NONE', #20142, .T. ) ;
#15760 = B_SPLINE_CURVE_WITH_KNOTS ( 'NONE', 3,
 ( #18649, #28154, #13965, #2102, #4910, #26596, #14724, #24232, #16755, #17651, #8145, #27169 ),
 .UNSPECIFIED., .F., .F.,
 ( 4, 2, 2, 2, 2, 4 ),
 ( 2.975096543306551241E-07, 0.0007805422437037919103, 0.001560786977753253132, 0.002341031711802714355, 0.002731154078827435425, 0.003121276445852156928 ),
 .UNSPECIFIED. ) ;
#15761 = CARTESIAN_POINT ( 'NONE',  ( 15.38325456941029579, -7.285321374151288332, 6.641371103590088865 ) ) ;
#15762 = EDGE_CURVE ( 'NONE', #6841, #2309, #25418, .T. ) ;
#15763 = CARTESIAN_POINT ( 'NONE',  ( -15.97321056478110179, 12.06495093120146045, 6.892848776733236704 ) ) ;
#15764 = CARTESIAN_POINT ( 'NONE',  ( 3.978203543573291867, 16.57681993851655022, 20.34789198813115263 ) ) ;
#15765 = ORIENTED_EDGE ( 'NONE', *, *, #19086, .F. ) ;
#15766 = VERTEX_POINT ( 'NONE', #11213 ) ;
#15767 = EDGE_CURVE ( 'NONE', #15364, #14320, #18854, .T. ) ;
#15768 = LINE ( 'NONE', #28085, #26236 ) ;
#15769 = CIRCLE ( 'NONE', #6307, 20.00000000000000000 ) ;
#15770 = CARTESIAN_POINT ( 'NONE',  ( 10.67036453487905767, -13.33339184396348287, 6.917457548096560771 ) ) ;
#15771 = CARTESIAN_POINT ( 'NONE',  ( 15.45572804192158500, 12.69342571624615168, 18.84056766331480404 ) ) ;
#15772 = CARTESIAN_POINT ( 'NONE',  ( 12.69001473637765365, 11.36098604101993637, 5.774779864094941040 ) ) ;
#15773 = CARTESIAN_POINT ( 'NONE',  ( 0.000000000000000000, 0.000000000000000000, 1.500000000000001332 ) ) ;
#15774 = CARTESIAN_POINT ( 'NONE',  ( -27.61994877245214397, 25.33817162612066554, 27.50000000000000000 ) ) ;
#15775 = AXIS2_PLACEMENT_3D ( 'NONE', #2712, #22035, #10187 ) ;
#15776 = DIRECTION ( 'NONE',  ( -0.000000000000000000, 0.000000000000000000, 1.000000000000000000 ) ) ;
#15777 = ORIENTED_EDGE ( 'NONE', *, *, #5581, .F. ) ;
#15778 = CIRCLE ( 'NONE', #18765, 28.20443790117963800 ) ;
#15779 = CIRCLE ( 'NONE', #25752, 9.482273699623480212 ) ;
#15780 = DIRECTION ( 'NONE',  ( 0.000000000000000000, 0.000000000000000000, 1.000000000000000000 ) ) ;
#15781 = DIRECTION ( 'NONE',  ( 0.000000000000000000, 0.000000000000000000, 1.000000000000000000 ) ) ;
#15782 = ORIENTED_EDGE ( 'NONE', *, *, #4748, .F. ) ;
#15783 = ORIENTED_EDGE ( 'NONE', *, *, #8480, .T. ) ;
#15784 = DIRECTION ( 'NONE',  ( -0.000000000000000000, 1.000000000000000000, -0.000000000000000000 ) ) ;
#15785 = B_SPLINE_CURVE_WITH_KNOTS ( 'NONE', 1,
 ( #23677, #14333 ),
 .UNSPECIFIED., .F., .F.,
 ( 2, 2 ),
 ( 0.1666666666666656582, 1.000000000000000000 ),
 .UNSPECIFIED. ) ;
#15786 = DIRECTION ( 'NONE',  ( 0.000000000000000000, 0.000000000000000000, -1.000000000000000000 ) ) ;
#15787 = ORIENTED_EDGE ( 'NONE', *, *, #21146, .F. ) ;
#15788 = CARTESIAN_POINT ( 'NONE',  ( -23.05654803992426949, -35.38768971485402659, -9.833278432273298009 ) ) ;
#15789 = CARTESIAN_POINT ( 'NONE',  ( 6.209160252570208982, 49.61505262654815596, -68.66330880567365114 ) ) ;
#15790 = DIRECTION ( 'NONE',  ( -0.000000000000000000, -0.000000000000000000, 1.000000000000000000 ) ) ;
#15791 = DIRECTION ( 'NONE',  ( -1.000000000000000000, 0.000000000000000000, 0.000000000000000000 ) ) ;
#15792 = VECTOR ( 'NONE', #30143, 1000.000000000000227 ) ;
#15793 = LINE ( 'NONE', #17843, #13344 ) ;
#15794 = VECTOR ( 'NONE', #1337, 1000.000000000000000 ) ;
#15795 = DIRECTION ( 'NONE',  ( -0.000000000000000000, -0.000000000000000000, -1.000000000000000000 ) ) ;
#15796 = CARTESIAN_POINT ( 'NONE',  ( 1.733314906354231910, -16.98782497260186375, 6.995624166085161910 ) ) ;
#15797 = CARTESIAN_POINT ( 'NONE',  ( -16.81857544482355493, 2.623036418797992209, 6.385774490351135313 ) ) ;
#15798 = VERTEX_POINT ( 'NONE', #16505 ) ;
#15799 = CIRCLE ( 'NONE', #23752, 9.000000000000000000 ) ;
#15800 = CARTESIAN_POINT ( 'NONE',  ( 6.778663211761466911, -6.630478080506930105, 1.500000000000001332 ) ) ;
#15801 = DIRECTION ( 'NONE',  ( 0.000000000000000000, 0.000000000000000000, 1.000000000000000000 ) ) ;
#15802 = CARTESIAN_POINT ( 'NONE',  ( -4.769904382622641492, 16.34378370247567247, 7.267659094423558841 ) ) ;
#15803 = CARTESIAN_POINT ( 'NONE',  ( -18.02600256144196678, -8.705149951716494527, 18.34838970509067479 ) ) ;
#15804 = AXIS2_PLACEMENT_3D ( 'NONE', #18056, #4160, #11349 ) ;
#15805 = EDGE_CURVE ( 'NONE', #25108, #11004, #22136, .T. ) ;
#15806 = CARTESIAN_POINT ( 'NONE',  ( -23.96732207939035675, 33.98584080153585774, -1.500000000000000000 ) ) ;
#15807 = AXIS2_PLACEMENT_3D ( 'NONE', #21386, #2054, #14057 ) ;
#15808 = DIRECTION ( 'NONE',  ( -1.000000000000000000, -0.000000000000000000, -0.000000000000000000 ) ) ;
#15809 = CIRCLE ( 'NONE', #27779, 1.447898107987198646 ) ;
#15810 = ORIENTED_EDGE ( 'NONE', *, *, #29867, .F. ) ;
#15811 = CARTESIAN_POINT ( 'NONE',  ( 0.5584673446548731324, -5.621163452808898953, -8.263859302085702296 ) ) ;
#15812 = CARTESIAN_POINT ( 'NONE',  ( 31.18700685317022803, -26.11823559933272421, -1.500000000000000000 ) ) ;
#15813 = CARTESIAN_POINT ( 'NONE',  ( 23.10194695014233091, -34.27363447027268961, 34.50719889637104387 ) ) ;
#15814 = CLOSED_SHELL ( 'NONE', ( #5804, #30028, #978, #17412, #4617, #6888 ) ) ;
#15815 = CARTESIAN_POINT ( 'NONE',  ( -4.163336342344337027E-14, 1.387778780781445676E-14, -1.500000000000000000 ) ) ;
#15816 = VERTEX_POINT ( 'NONE', #2007 ) ;
#15817 = CARTESIAN_POINT ( 'NONE',  ( 3.068634486547840101, 16.80010772488981985, 6.521906765011495466 ) ) ;
#15818 = AXIS2_PLACEMENT_3D ( 'NONE', #18555, #18860, #16201 ) ;
#15819 = CARTESIAN_POINT ( 'NONE',  ( 20.65888525914559892, 38.75220717792412728, -19.50000000000000355 ) ) ;
#15820 = CARTESIAN_POINT ( 'NONE',  ( -2.931009552726342449, 14.22630671667915792, 1.500000000000000000 ) ) ;
#15821 = AXIS2_PLACEMENT_3D ( 'NONE', #1748, #15955, #1904 ) ;
#15822 = VERTEX_POINT ( 'NONE', #12140 ) ;
#15823 = CIRCLE ( 'NONE', #19243, 1.447898107987198646 ) ;
#15824 = CARTESIAN_POINT ( 'NONE',  ( -8.099370871304801156, -15.01721251058671491, 20.24143955528809258 ) ) ;
#15825 = CARTESIAN_POINT ( 'NONE',  ( -10.00000000000004263, 1.387778780781445676E-14, 21.50000000000000000 ) ) ;
#15826 = VERTEX_POINT ( 'NONE', #23656 ) ;
#15827 = CARTESIAN_POINT ( 'NONE',  ( -31.46019086465472725, -15.19107625323260180, 40.06435153370532021 ) ) ;
#15828 = VECTOR ( 'NONE', #30171, 1000.000000000000000 ) ;
#15829 = B_SPLINE_CURVE_WITH_KNOTS ( 'NONE', 3,
 ( #7740, #5086, #14739, #16938, #12424, #21919, #26455, #29099, #7900, #3205, #8050, #17242, #17407, #15824, #22843, #1325 ),
 .UNSPECIFIED., .F., .F.,
 ( 4, 2, 2, 2, 2, 2, 2, 4 ),
 ( 0.5000000000000000000, 0.6250000000000015543, 0.6875000000000021094, 0.7187500000000023315, 0.7500000000000025535, 0.8125000000000014433, 0.8750000000000003331, 1.000000000000000000 ),
 .UNSPECIFIED. ) ;
#15830 = CARTESIAN_POINT ( 'NONE',  ( 31.79271162922634630, -14.90794587988476927, 39.88583012296468411 ) ) ;
#15831 = AXIS2_PLACEMENT_3D ( 'NONE', #28001, #28470, #7095 ) ;
#15832 = EDGE_LOOP ( 'NONE', ( #17837, #6235, #13885, #8575, #27707 ) ) ;
#15833 = DIRECTION ( 'NONE',  ( 0.000000000000000000, 0.000000000000000000, 1.000000000000000000 ) ) ;
#15834 = CARTESIAN_POINT ( 'NONE',  ( 12.88304655979403712, 11.13107787102070745, 18.72771030977187223 ) ) ;
#15835 = ADVANCED_FACE ( 'NONE', ( #120 ), #28517, .F. ) ;
#15836 = DIRECTION ( 'NONE',  ( 1.000000000000000000, 0.000000000000000000, 0.000000000000000000 ) ) ;
#15837 = CARTESIAN_POINT ( 'NONE',  ( -9.216505592218814158, -7.781333699927420966, 1.500000000000000000 ) ) ;
#15838 = AXIS2_PLACEMENT_3D ( 'NONE', #15705, #13080, #12614 ) ;
#15839 = EDGE_CURVE ( 'NONE', #24441, #24048, #11531, .T. ) ;
#15840 = CARTESIAN_POINT ( 'NONE',  ( -15.42263072602161422, -7.221902784682912468, 18.54473042795394733 ) ) ;
#15841 = CIRCLE ( 'NONE', #27815, 9.084132297865673777 ) ;
#15842 = PLANE ( 'NONE',  #18823 ) ;
#15843 = DIRECTION ( 'NONE',  ( -1.000000000000000000, 0.000000000000000000, 0.000000000000000000 ) ) ;
#15844 = EDGE_CURVE ( 'NONE', #15686, #17832, #2471, .T. ) ;
#15845 = FACE_OUTER_BOUND ( 'NONE', #20453, .T. ) ;
#15846 = ADVANCED_FACE ( 'NONE', ( #6830 ), #26021, .T. ) ;
#15847 = CARTESIAN_POINT ( 'NONE',  ( 9.184330860425914622, -14.33603326861445382, 6.031926333436654630 ) ) ;
#15848 = CARTESIAN_POINT ( 'NONE',  ( -9.395348974764861083, -14.19336984580852956, 19.41069149716887665 ) ) ;
#15849 = ORIENTED_EDGE ( 'NONE', *, *, #7514, .F. ) ;
#15850 = ORIENTED_EDGE ( 'NONE', *, *, #26367, .T. ) ;
#15851 = CARTESIAN_POINT ( 'NONE',  ( 4.510281037539698445E-13, -4.926614671774132148E-13, 65.49999999999998579 ) ) ;
#15852 = CARTESIAN_POINT ( 'NONE',  ( 5.374868878255610660, 44.10336124695606230, -19.50000000000000355 ) ) ;
#15853 = CIRCLE ( 'NONE', #28305, 0.7500000000000006661 ) ;
#15854 = EDGE_CURVE ( 'NONE', #19170, #23449, #20648, .T. ) ;
#15855 = CARTESIAN_POINT ( 'NONE',  ( 12.24063095261064404, 4.490763173670002217, 1.500000000000001332 ) ) ;
#15856 = EDGE_LOOP ( 'NONE', ( #10493, #15385, #22443, #14045 ) ) ;
#15857 = VECTOR ( 'NONE', #30182, 1000.000000000000000 ) ;
#15858 = LINE ( 'NONE', #20386, #12913 ) ;
#15859 = EDGE_CURVE ( 'NONE', #5082, #5196, #15144, .T. ) ;
#15860 = VECTOR ( 'NONE', #19827, 1000.000000000000000 ) ;
#15861 = CARTESIAN_POINT ( 'NONE',  ( 39.99999999999998579, 87.00000000000001421, 62.49999999999999289 ) ) ;
#15862 = EDGE_CURVE ( 'NONE', #24493, #24670, #1705, .T. ) ;
#15863 = ORIENTED_EDGE ( 'NONE', *, *, #381, .F. ) ;
#15864 = ORIENTED_EDGE ( 'NONE', *, *, #12056, .F. ) ;
#15865 = CARTESIAN_POINT ( 'NONE',  ( -16.87659098782771849, 2.276273425076629664, 5.862424720655265098 ) ) ;
#15866 = CARTESIAN_POINT ( 'NONE',  ( -30.86161751192252467, -15.46691422980912733, 36.23697955569767970 ) ) ;
#15867 = VECTOR ( 'NONE', #12383, 1000.000000000000000 ) ;
#15868 = CARTESIAN_POINT ( 'NONE',  ( -2.350907959953084880, -44.02170661032951671, -16.49999999999999645 ) ) ;
#15869 = DIRECTION ( 'NONE',  ( 1.000000000000000000, 0.000000000000000000, 0.000000000000000000 ) ) ;
#15870 = EDGE_LOOP ( 'NONE', ( #19645, #13754 ) ) ;
#15871 = CARTESIAN_POINT ( 'NONE',  ( 26.36764545593179676, 31.31467416275351923, 1.500000000000000000 ) ) ;
#15872 = VERTEX_POINT ( 'NONE', #23973 ) ;
#15873 = CYLINDRICAL_SURFACE ( 'NONE', #16040, 0.7500000000000006661 ) ;
#15874 = CARTESIAN_POINT ( 'NONE',  ( -50.00000000000000000, 50.00000000000000000, 12.49999999999999112 ) ) ;
#15875 = ORIENTED_EDGE ( 'NONE', *, *, #1029, .F. ) ;
#15876 = CARTESIAN_POINT ( 'NONE',  ( -39.70095622563229654, 7.028748154183642072, -13.16666434799648755 ) ) ;
#15877 = EDGE_CURVE ( 'NONE', #2660, #1286, #16357, .T. ) ;
#15878 = CARTESIAN_POINT ( 'NONE',  ( 24.50429677314015109, -7.442113211156457631, 45.14840481399649974 ) ) ;
#15879 = AXIS2_PLACEMENT_3D ( 'NONE', #13977, #23165, #23473 ) ;
#15880 = EDGE_CURVE ( 'NONE', #26848, #11554, #21480, .T. ) ;
#15881 = LINE ( 'NONE', #18068, #23042 ) ;
#15882 = B_SPLINE_SURFACE_WITH_KNOTS ( 'NONE', 3, 1, ( 
 ( #25734, #4672 ),
 ( #143, #23992 ),
 ( #14174, #2178 ),
 ( #13886, #21658 ),
 ( #18573, #2325 ),
 ( #23388, #21351 ),
 ( #28079, #9507 ),
 ( #16681, #11550 ),
 ( #19025, #29470 ),
 ( #29151, #7633 ),
 ( #5135, #16982 ),
 ( #26504, #8104 ),
 ( #22279, #748 ),
 ( #12778, #2797 ),
 ( #3417, #24774 ),
 ( #12481, #28996 ),
 ( #17460, #12942 ),
 ( #17295, #922 ),
 ( #29314, #21973 ),
 ( #24467, #22435 ),
 ( #27129, #14646 ),
 ( #5752, #15243 ),
 ( #26829, #5289 ),
 ( #24148, #26982 ),
 ( #21820, #14796 ),
 ( #5608, #26659 ),
 ( #5453, #7487 ),
 ( #602, #10438 ),
 ( #15104, #14956 ),
 ( #19952, #461 ),
 ( #19483, #24619 ) ),
 .UNSPECIFIED., .F., .F., .F.,
 ( 4, 3, 3, 3, 3, 3, 3, 3, 3, 3, 4 ),
 ( 2, 2 ),
 ( 0.000000000000000000, 0.05425176834609633791, 0.1085332949128352958, 0.1623767749169382768, 0.2157504826133063158, 0.2688657508888171455, 0.3218907763505476360, 0.3749548578363336993, 0.4282048033836242107, 0.4818374082110501444, 0.4999999999131655715 ),
 ( 0.000000000000000000, 1.000000000000000000 ),
 .UNSPECIFIED. ) ;
#15883 = CARTESIAN_POINT ( 'NONE',  ( 16.74328840634222715, 3.194145055459935101, 7.652108011868850035 ) ) ;
#15884 = CIRCLE ( 'NONE', #14379, 34.99999999999933920 ) ;
#15885 = VECTOR ( 'NONE', #20860, 1000.000000000000000 ) ;
#15886 = VECTOR ( 'NONE', #24836, 1000.000000000000000 ) ;
#15887 = EDGE_CURVE ( 'NONE', #6434, #20068, #206, .T. ) ;
#15888 = CARTESIAN_POINT ( 'NONE',  ( -7.726154291500652249, -15.22816856119838391, 19.69140814234746273 ) ) ;
#15889 = DIRECTION ( 'NONE',  ( -0.000000000000000000, -0.000000000000000000, -1.000000000000000000 ) ) ;
#15890 = CARTESIAN_POINT ( 'NONE',  ( -19.86132161767506688, 2.497832813224996951, 18.34798005862662507 ) ) ;
#15891 = CARTESIAN_POINT ( 'NONE',  ( 0.4269445148198162121, -2.969464325642846347, 24.50000000000000000 ) ) ;
#15892 = EDGE_LOOP ( 'NONE', ( #8175, #19242, #4618, #24074 ) ) ;
#15893 = ADVANCED_FACE ( 'NONE', ( #18690 ), #25870, .F. ) ;
#15894 = CARTESIAN_POINT ( 'NONE',  ( -29.06468222671494672, 28.34114264639704572, 16.11924918789928185 ) ) ;
#15895 = AXIS2_PLACEMENT_3D ( 'NONE', #725, #17268, #16959 ) ;
#15896 = CARTESIAN_POINT ( 'NONE',  ( 31.18890335284658022, 19.89223002944920538, 27.50000000000001066 ) ) ;
#15897 = ORIENTED_EDGE ( 'NONE', *, *, #13799, .T. ) ;
#15898 = ORIENTED_EDGE ( 'NONE', *, *, #2912, .F. ) ;
#15899 = DIRECTION ( 'NONE',  ( -0.3598999890241659783, -0.9329908884337537733, 0.000000000000000000 ) ) ;
#15900 = CYLINDRICAL_SURFACE ( 'NONE', #18613, 0.7500000000000006661 ) ;
#15901 = ADVANCED_FACE ( 'NONE', ( #2155 ), #12620, .T. ) ;
#15902 = CARTESIAN_POINT ( 'NONE',  ( -5.002692087210952820, 19.38273059899790596, 6.755862304746362845 ) ) ;
#15903 = ORIENTED_EDGE ( 'NONE', *, *, #30373, .F. ) ;
#15904 = AXIS2_PLACEMENT_3D ( 'NONE', #3972, #20492, #8654 ) ;
#15905 = CARTESIAN_POINT ( 'NONE',  ( 8.817355867515813017, 2.185336383880231992, -1.500000000000001554 ) ) ;
#15906 = DIRECTION ( 'NONE',  ( 0.000000000000000000, 0.000000000000000000, 1.000000000000000000 ) ) ;
#15907 = DIRECTION ( 'NONE',  ( 1.000000000000000000, 0.000000000000000000, 0.000000000000000000 ) ) ;
#15908 = ORIENTED_EDGE ( 'NONE', *, *, #23326, .T. ) ;
#15909 = CARTESIAN_POINT ( 'NONE',  ( -15.10419704716067102, -17.26937953831884442, 1.500000000000000000 ) ) ;
#15910 = AXIS2_PLACEMENT_3D ( 'NONE', #11479, #30487, #4747 ) ;
#15911 = CARTESIAN_POINT ( 'NONE',  ( -50.00000000000000000, 70.00000000000000000, -34.49999999999999289 ) ) ;
#15912 = VERTEX_POINT ( 'NONE', #17439 ) ;
#15913 = LINE ( 'NONE', #25425, #29271 ) ;
#15914 = EDGE_LOOP ( 'NONE', ( #25274, #24436, #5457, #19254 ) ) ;
#15915 = EDGE_CURVE ( 'NONE', #19456, #28062, #15217, .T. ) ;
#15916 = DIRECTION ( 'NONE',  ( 1.000000000000000000, 0.000000000000000000, 0.000000000000000000 ) ) ;
#15917 = EDGE_CURVE ( 'NONE', #28288, #3771, #5582, .T. ) ;
#15918 = EDGE_CURVE ( 'NONE', #17265, #10035, #22414, .T. ) ;
#15919 = ORIENTED_EDGE ( 'NONE', *, *, #20894, .T. ) ;
#15920 = AXIS2_PLACEMENT_3D ( 'NONE', #24632, #3265, #10450 ) ;
#15921 = VERTEX_POINT ( 'NONE', #5887 ) ;
#15922 = CARTESIAN_POINT ( 'NONE',  ( 4.982076346116051546, 19.38816267120398606, 7.603368798681074736 ) ) ;
#15923 = CARTESIAN_POINT ( 'NONE',  ( 32.90011853910910844, 8.843064278303863546, 40.93222828939945401 ) ) ;
#15924 = DIRECTION ( 'NONE',  ( -0.000000000000000000, 0.000000000000000000, 1.000000000000000000 ) ) ;
#15925 = EDGE_LOOP ( 'NONE', ( #10517, #5773, #22669, #6411 ) ) ;
#15926 = CIRCLE ( 'NONE', #25383, 21.71568325578202163 ) ;
#15927 = CARTESIAN_POINT ( 'NONE',  ( 9.331524088667743300, -14.24511854140749811, 18.55820869691756769 ) ) ;
#15928 = DIRECTION ( 'NONE',  ( 1.000000000000000000, 0.000000000000000000, 0.000000000000000000 ) ) ;
#15929 = ORIENTED_EDGE ( 'NONE', *, *, #10320, .T. ) ;
#15930 = CARTESIAN_POINT ( 'NONE',  ( 29.61203839202725518, -15.40012917324033381, -16.55003854064094426 ) ) ;
#15931 = CARTESIAN_POINT ( 'NONE',  ( 15.67520293387196517, -6.672517015027196408, 7.595116371587256054 ) ) ;
#15932 = CARTESIAN_POINT ( 'NONE',  ( -13.59008529392185238, 10.30512752726515302, 20.29915277494337644 ) ) ;
#15933 = CARTESIAN_POINT ( 'NONE',  ( 3.160432912108479098, 16.77963207014077796, 19.79423548914561692 ) ) ;
#15934 = EDGE_LOOP ( 'NONE', ( #30643, #27243, #2464, #10034 ) ) ;
#15935 = ORIENTED_EDGE ( 'NONE', *, *, #30731, .F. ) ;
#15936 = DIRECTION ( 'NONE',  ( -0.000000000000000000, -0.000000000000000000, -1.000000000000000000 ) ) ;
#15937 = CARTESIAN_POINT ( 'NONE',  ( 17.26937953831880534, -14.36006998371588317, 1.500000000000000000 ) ) ;
#15938 = CARTESIAN_POINT ( 'NONE',  ( -4.718303904200451093, 16.35736724179925972, 19.87181966307587544 ) ) ;
#15939 = SURFACE_STYLE_USAGE ( .BOTH. , #11104 ) ;
#15940 = CARTESIAN_POINT ( 'NONE',  ( 1.492780340587499928E-15, -12.18947652193949693, 29.43090101791767665 ) ) ;
#15941 = CIRCLE ( 'NONE', #2480, 0.7441270634457163302 ) ;
#15942 = CARTESIAN_POINT ( 'NONE',  ( 6.587096388939653657, -18.88412458026098406, 24.50000000000000000 ) ) ;
#15943 = CARTESIAN_POINT ( 'NONE',  ( 23.07593096178834102, -11.40900259639455072, 49.25816067352246108 ) ) ;
#15944 = VERTEX_POINT ( 'NONE', #24126 ) ;
#15945 = VECTOR ( 'NONE', #7250, 1000.000000000000000 ) ;
#15946 = CARTESIAN_POINT ( 'NONE',  ( 1.164358918501127604, -19.96629823696783035, 6.037995405461183296 ) ) ;
#15947 = CARTESIAN_POINT ( 'NONE',  ( -24.03057240117691862, 26.57182937991348481, 1.500000000000001332 ) ) ;
#15948 = CYLINDRICAL_SURFACE ( 'NONE', #2502, 9.482273699623480212 ) ;
#15949 = VERTEX_POINT ( 'NONE', #2778 ) ;
#15950 = DIRECTION ( 'NONE',  ( 1.000000000000000000, 0.000000000000000000, 0.000000000000000000 ) ) ;
#15951 = VERTEX_POINT ( 'NONE', #12292 ) ;
#15952 = DIRECTION ( 'NONE',  ( 0.000000000000000000, 0.000000000000000000, -1.000000000000000000 ) ) ;
#15953 = CARTESIAN_POINT ( 'NONE',  ( -19.86062922652984852, 2.360743482685567773, 18.34869673959212122 ) ) ;
#15954 = ORIENTED_EDGE ( 'NONE', *, *, #3911, .T. ) ;
#15955 = DIRECTION ( 'NONE',  ( 0.000000000000000000, 0.000000000000000000, -1.000000000000000000 ) ) ;
#15956 = DIRECTION ( 'NONE',  ( -0.5503133621338236470, 0.8349582046168341209, 0.000000000000000000 ) ) ;
#15957 = DIRECTION ( 'NONE',  ( 0.000000000000000000, 1.000000000000000000, 0.000000000000000000 ) ) ;
#15958 = DIRECTION ( 'NONE',  ( 0.000000000000000000, 1.132880637372608986E-16, -1.000000000000000000 ) ) ;
#15959 = CYLINDRICAL_SURFACE ( 'NONE', #8784, 0.7500000000000015543 ) ;
#15960 = CARTESIAN_POINT ( 'NONE',  ( 33.42925964089141644, -11.06161099612213228, 39.78814634291933316 ) ) ;
#15961 = DIRECTION ( 'NONE',  ( 1.000000000000000000, 0.000000000000000000, 0.000000000000000000 ) ) ;
#15962 = CARTESIAN_POINT ( 'NONE',  ( -31.89304216768362110, 14.79375299452194881, 39.84323675255983943 ) ) ;
#15963 = ORIENTED_EDGE ( 'NONE', *, *, #10532, .T. ) ;
#15964 = LINE ( 'NONE', #25779, #29237 ) ;
#15965 = CIRCLE ( 'NONE', #24871, 0.7499999999999997780 ) ;
#15966 = CYLINDRICAL_SURFACE ( 'NONE', #588, 0.7500000000000006661 ) ;
#15967 = CARTESIAN_POINT ( 'NONE',  ( 11.39002951368468253, -16.46174851469273293, 7.603368798681074736 ) ) ;
#15968 = CARTESIAN_POINT ( 'NONE',  ( 5.105024945673418912, -42.22604126506271882, -1.500000000000000000 ) ) ;
#15969 = DIRECTION ( 'NONE',  ( 0.000000000000000000, 0.000000000000000000, -1.000000000000000000 ) ) ;
#15970 = ORIENTED_EDGE ( 'NONE', *, *, #18756, .F. ) ;
#15971 = CYLINDRICAL_SURFACE ( 'NONE', #2448, 0.7500000000000015543 ) ;
#15972 = FACE_OUTER_BOUND ( 'NONE', #9487, .T. ) ;
#15973 = CARTESIAN_POINT ( 'NONE',  ( 20.46113952635996469, -31.44909971395763648, 37.49999999997999112 ) ) ;
#15974 = CARTESIAN_POINT ( 'NONE',  ( -12.54846374865995706, -9.550116103605043705, -0.6213203435596476032 ) ) ;
#15975 = EDGE_LOOP ( 'NONE', ( #23245, #25053, #1496, #7077 ) ) ;
#15976 = AXIS2_PLACEMENT_3D ( 'NONE', #21333, #14158, #19010 ) ;
#15977 = CARTESIAN_POINT ( 'NONE',  ( -13.71169828473024488, 10.15410312375059476, 7.545655578832112909 ) ) ;
#15978 = CARTESIAN_POINT ( 'NONE',  ( 35.76344986163714168, -22.29344514668044752, -19.50000000000000355 ) ) ;
#15979 = CARTESIAN_POINT ( 'NONE',  ( -4.608906612435655248, -7.730328572437724866, 21.50000000000000000 ) ) ;
#15980 = ORIENTED_EDGE ( 'NONE', *, *, #22155, .T. ) ;
#15981 = B_SPLINE_CURVE_WITH_KNOTS ( 'NONE', 3,
 ( #27019, #5647, #15142, #12824 ),
 .UNSPECIFIED., .F., .F.,
 ( 4, 4 ),
 ( 2.143643656977389965E-07, 0.003421830178490238485 ),
 .UNSPECIFIED. ) ;
#15982 = ADVANCED_FACE ( 'NONE', ( #21797 ), #30361, .F. ) ;
#15983 = CARTESIAN_POINT ( 'NONE',  ( -17.87976126528057108, -37.88093910584518653, 34.52266824050962413 ) ) ;
#15984 = VERTEX_POINT ( 'NONE', #23167 ) ;
#15985 = CARTESIAN_POINT ( 'NONE',  ( -29.81956388892671583, -15.48018185647901213, 41.40175883629457587 ) ) ;
#15986 = DIRECTION ( 'NONE',  ( 0.9329908884337542174, 0.3598999890241650901, 0.000000000000000000 ) ) ;
#15987 = DIRECTION ( 'NONE',  ( 0.000000000000000000, -1.132880637372608986E-16, 1.000000000000000000 ) ) ;
#15988 = DIRECTION ( 'NONE',  ( -0.000000000000000000, -0.000000000000000000, 1.000000000000000000 ) ) ;
#15989 = ORIENTED_EDGE ( 'NONE', *, *, #4389, .T. ) ;
#15990 = DIRECTION ( 'NONE',  ( 0.000000000000000000, 0.000000000000000000, 1.000000000000000000 ) ) ;
#15991 = CARTESIAN_POINT ( 'NONE',  ( -32.98805937973593672, 0.000000000000000000, 13.00000000000000178 ) ) ;
#15992 = CARTESIAN_POINT ( 'NONE',  ( -23.07950435457407679, -11.50806656539752737, 49.21048435262065368 ) ) ;
#15993 = AXIS2_PLACEMENT_3D ( 'NONE', #825, #17205, #21888 ) ;
#15994 = CARTESIAN_POINT ( 'NONE',  ( -44.79023165781732274, 69.31820106020313688, 13.69674458689816454 ) ) ;
#15995 = AXIS2_PLACEMENT_3D ( 'NONE', #30076, #1391, #3729 ) ;
#15996 = LINE ( 'NONE', #6632, #7353 ) ;
#15997 = CARTESIAN_POINT ( 'NONE',  ( 19.18576292979354392, -22.55620591602728453, 24.50000000000000000 ) ) ;
#15998 = CARTESIAN_POINT ( 'NONE',  ( -4.163336342344337027E-14, 1.387778780781445676E-14, 1.500000000000000000 ) ) ;
#15999 = DIRECTION ( 'NONE',  ( -0.8910248307962436165, -0.4539545692076746852, 0.000000000000000000 ) ) ;
#16000 = CARTESIAN_POINT ( 'NONE',  ( -4.163336342344337027E-14, -1.387778780781445676E-14, -1.500000000000000000 ) ) ;
#16001 = CARTESIAN_POINT ( 'NONE',  ( 9.644751206715360681, -14.04611738690515566, 5.676815824193228721 ) ) ;
#16002 = CARTESIAN_POINT ( 'NONE',  ( 0.000000000000000000, 0.000000000000000000, -16.50000000000000000 ) ) ;
#16003 = ORIENTED_EDGE ( 'NONE', *, *, #4185, .F. ) ;
#16004 = EDGE_LOOP ( 'NONE', ( #7490, #23443, #2177, #9382 ) ) ;
#16005 = CARTESIAN_POINT ( 'NONE',  ( -4.340342926365016396, -8.430595340551244377, 13.00000000000000178 ) ) ;
#16006 = CARTESIAN_POINT ( 'NONE',  ( -13.22505861668184046, -42.10773672057003125, -19.50000000000000355 ) ) ;
#16007 = DIRECTION ( 'NONE',  ( 1.000000000000000000, 0.000000000000000000, 0.000000000000000000 ) ) ;
#16008 = ORIENTED_EDGE ( 'NONE', *, *, #2498, .F. ) ;
#16009 = DIRECTION ( 'NONE',  ( 1.000000000000000000, 0.000000000000000000, 0.000000000000000000 ) ) ;
#16010 = DIRECTION ( 'NONE',  ( 0.000000000000000000, 0.000000000000000000, 1.000000000000000000 ) ) ;
#16011 = CARTESIAN_POINT ( 'NONE',  ( -7.392982946727046034, 5.278755796068742789, 13.22130136205108819 ) ) ;
#16012 = EDGE_CURVE ( 'NONE', #22374, #9580, #3722, .T. ) ;
#16013 = EDGE_LOOP ( 'NONE', ( #6376, #24548, #11163, #20879 ) ) ;
#16014 = CARTESIAN_POINT ( 'NONE',  ( -10.51100883930070040, -17.01524884273342764, 18.34798005863226678 ) ) ;
#16015 = VECTOR ( 'NONE', #30485, 1000.000000000000000 ) ;
#16016 = CARTESIAN_POINT ( 'NONE',  ( -10.52280129341197323, -17.02885805942690567, 18.34798005862930381 ) ) ;
#16017 = EDGE_CURVE ( 'NONE', #13348, #12864, #4934, .T. ) ;
#16018 = DIRECTION ( 'NONE',  ( 0.000000000000000000, 0.000000000000000000, -1.000000000000000000 ) ) ;
#16019 = VERTEX_POINT ( 'NONE', #6194 ) ;
#16020 = PLANE ( 'NONE',  #25307 ) ;
#16021 = ORIENTED_EDGE ( 'NONE', *, *, #11824, .T. ) ;
#16022 = ADVANCED_FACE ( 'NONE', ( #9002 ), #13220, .F. ) ;
#16023 = DIRECTION ( 'NONE',  ( -0.000000000000000000, -0.000000000000000000, 1.000000000000000000 ) ) ;
#16024 = CARTESIAN_POINT ( 'NONE',  ( -15.34307810681595718, 12.82926163924266483, 7.652108011868850035 ) ) ;
#16025 = ORIENTED_EDGE ( 'NONE', *, *, #6709, .T. ) ;
#16026 = DIRECTION ( 'NONE',  ( 0.000000000000000000, 0.000000000000000000, 1.000000000000000000 ) ) ;
#16027 = FACE_OUTER_BOUND ( 'NONE', #26194, .T. ) ;
#16028 = CIRCLE ( 'NONE', #2585, 20.00000000000000000 ) ;
#16029 = CARTESIAN_POINT ( 'NONE',  ( -50.00000000000000000, 50.00000000000000000, 62.49999999999999289 ) ) ;
#16030 = CARTESIAN_POINT ( 'NONE',  ( 0.3346962451677066297, -17.03061174119336840, 7.557577766377196582 ) ) ;
#16031 = ADVANCED_FACE ( 'NONE', ( #27565 ), #22708, .F. ) ;
#16032 = DIRECTION ( 'NONE',  ( -0.000000000000000000, -0.000000000000000000, 1.000000000000000000 ) ) ;
#16033 = EDGE_CURVE ( 'NONE', #23120, #21154, #8725, .T. ) ;
#16034 = DIRECTION ( 'NONE',  ( 0.000000000000000000, 0.000000000000000000, -1.000000000000000000 ) ) ;
#16035 = CARTESIAN_POINT ( 'NONE',  ( 0.000000000000000000, 1.699320956058915452E-16, -1.500000000000001776 ) ) ;
#16036 = CARTESIAN_POINT ( 'NONE',  ( 0.6210184355499436260, -9.062880100047301823, 13.22130136205108641 ) ) ;
#16037 = ORIENTED_EDGE ( 'NONE', *, *, #23833, .F. ) ;
#16038 = B_SPLINE_CURVE_WITH_KNOTS ( 'NONE', 3,
 ( #10164, #17181, #29512, #24356, #17502, #7683, #19671, #29662, #3299, #15457, #3003, #12982, #7832, #1120, #22472, #29360 ),
 .UNSPECIFIED., .F., .F.,
 ( 4, 2, 2, 2, 2, 2, 2, 4 ),
 ( 3.030954607830198967E-16, 0.001284364552519681778, 0.001926546828779363832, 0.002568729105039046102, 0.003853093657558390259, 0.005137458210077733983, 0.007706187315116445717, 0.01027491642015515745 ),
 .UNSPECIFIED. ) ;
#16039 = CARTESIAN_POINT ( 'NONE',  ( 11.11866356627124297, -16.64591798801204447, 18.34798005862662507 ) ) ;
#16040 = AXIS2_PLACEMENT_3D ( 'NONE', #2128, #16023, #25392 ) ;
#16041 = CARTESIAN_POINT ( 'NONE',  ( 32.31576317091161599, -17.59561277345965280, 27.50000000000000355 ) ) ;
#16042 = EDGE_LOOP ( 'NONE', ( #2694, #20038, #93, #12241 ) ) ;
#16043 = VERTEX_POINT ( 'NONE', #18515 ) ;
#16044 = DIRECTION ( 'NONE',  ( 0.000000000000000000, 0.000000000000000000, 1.000000000000000000 ) ) ;
#16045 = CARTESIAN_POINT ( 'NONE',  ( -4.568010850242218091, 16.39675899511905399, 6.641371103590088865 ) ) ;
#16046 = VERTEX_POINT ( 'NONE', #15861 ) ;
#16047 = CARTESIAN_POINT ( 'NONE',  ( 0.000000000000000000, 1.699320956058915452E-16, -1.500000000000001776 ) ) ;
#16048 = EDGE_CURVE ( 'NONE', #27304, #2787, #3239, .T. ) ;
#16049 = ORIENTED_EDGE ( 'NONE', *, *, #21517, .T. ) ;
#16050 = EDGE_CURVE ( 'NONE', #15430, #25523, #2232, .T. ) ;
#16051 = AXIS2_PLACEMENT_3D ( 'NONE', #17615, #8106, #21696 ) ;
#16052 = CARTESIAN_POINT ( 'NONE',  ( 1.687027447297431371, 8.840471615930075799, 21.50000000000000000 ) ) ;
#16053 = EDGE_CURVE ( 'NONE', #4577, #28559, #27716, .T. ) ;
#16054 = DIRECTION ( 'NONE',  ( -0.000000000000000000, 1.132880637372608986E-16, -1.000000000000000000 ) ) ;
#16055 = ORIENTED_EDGE ( 'NONE', *, *, #16402, .F. ) ;
#16056 = LINE ( 'NONE', #1704, #16819 ) ;
#16057 = ORIENTED_EDGE ( 'NONE', *, *, #18625, .F. ) ;
#16058 = CARTESIAN_POINT ( 'NONE',  ( -7.341751895053199917, 5.349779314757666882, 21.50000000000000000 ) ) ;
#16059 = EDGE_CURVE ( 'NONE', #16132, #12146, #23137, .T. ) ;
#16060 = PRODUCT_DEFINITION_CONTEXT ( 'detailed design', #5010, 'design' ) ;
#16061 = ORIENTED_EDGE ( 'NONE', *, *, #23639, .T. ) ;
#16062 = ORIENTED_EDGE ( 'NONE', *, *, #12650, .F. ) ;
#16063 = EDGE_CURVE ( 'NONE', #9274, #28044, #6502, .T. ) ;
#16064 = EDGE_CURVE ( 'NONE', #14826, #30777, #18190, .T. ) ;
#16065 = DIRECTION ( 'NONE',  ( 0.000000000000000000, 0.000000000000000000, -1.000000000000000000 ) ) ;
#16066 = CARTESIAN_POINT ( 'NONE',  ( 0.5590800469813748119, -9.968355046870097880, -0.7343025909353961822 ) ) ;
#16067 = EDGE_CURVE ( 'NONE', #6047, #24171, #9689, .T. ) ;
#16068 = VECTOR ( 'NONE', #18409, 1000.000000000000000 ) ;
#16069 = AXIS2_PLACEMENT_3D ( 'NONE', #15133, #29028, #3284 ) ;
#16070 = CARTESIAN_POINT ( 'NONE',  ( 11.08678458728283545, -16.66722406908985477, 18.34777357837152323 ) ) ;
#16071 = CARTESIAN_POINT ( 'NONE',  ( 2.959227181723801170, -8.499586724479446076, -3.621320343559650379 ) ) ;
#16072 = EDGE_LOOP ( 'NONE', ( #661, #6156 ) ) ;
#16073 = VECTOR ( 'NONE', #23191, 1000.000000000000000 ) ;
#16074 = CARTESIAN_POINT ( 'NONE',  ( -16.92011235424303450, 1.986018190673852546, 20.29090034784956131 ) ) ;
#16075 = CARTESIAN_POINT ( 'NONE',  ( 17.92217092160593950, -8.916983838001998564, 6.641371103590088865 ) ) ;
#16076 = CARTESIAN_POINT ( 'NONE',  ( -15.89252301733158568, 12.17122019226246721, 7.196036389296800451 ) ) ;
#16077 = CARTESIAN_POINT ( 'NONE',  ( 5.225607896785843920, 19.32380464960333555, 18.34838970509067479 ) ) ;
#16078 = ORIENTED_EDGE ( 'NONE', *, *, #20090, .T. ) ;
#16079 = VERTEX_POINT ( 'NONE', #16320 ) ;
#16080 = DIRECTION ( 'NONE',  ( -1.000000000000000000, -9.769962616701377556E-15, 0.000000000000000000 ) ) ;
#16081 = CARTESIAN_POINT ( 'NONE',  ( 10.66613195287249560, -13.33645323721333220, 6.392658652357120275 ) ) ;
#16082 = CARTESIAN_POINT ( 'NONE',  ( 13.73901823217154750, -39.81659909301839662, 21.93900229243933353 ) ) ;
#16083 = CARTESIAN_POINT ( 'NONE',  ( -4.619434794156388691, 16.38343285047924169, 19.66989035740801839 ) ) ;
#16084 = SURFACE_STYLE_FILL_AREA ( #25453 ) ;
#16085 = CARTESIAN_POINT ( 'NONE',  ( 11.75084321055180858, 12.38658771205033560, 6.147510495896842286 ) ) ;
#16086 = CARTESIAN_POINT ( 'NONE',  ( -13.22604046949001066, 36.76012593405532414, 27.49999999999999645 ) ) ;
#16087 = EDGE_CURVE ( 'NONE', #14124, #26044, #2737, .T. ) ;
#16088 = DIRECTION ( 'NONE',  ( 1.000000000000000000, 0.000000000000000000, 0.000000000000000000 ) ) ;
#16089 = ORIENTED_EDGE ( 'NONE', *, *, #9397, .F. ) ;
#16090 = ADVANCED_FACE ( 'NONE', ( #11958 ), #22330, .T. ) ;
#16091 = CARTESIAN_POINT ( 'NONE',  ( -19.96188467872886463, 1.492656647078446364, 6.782048567692550378 ) ) ;
#16092 = DIRECTION ( 'NONE',  ( -0.000000000000000000, -0.000000000000000000, -1.000000000000000000 ) ) ;
#16093 = DIRECTION ( 'NONE',  ( 1.000000000000000000, 0.000000000000000000, 0.000000000000000000 ) ) ;
#16094 = EDGE_LOOP ( 'NONE', ( #29424, #19361 ) ) ;
#16095 = FACE_OUTER_BOUND ( 'NONE', #25093, .T. ) ;
#16096 = CIRCLE ( 'NONE', #17586, 0.7499999999999988898 ) ;
#16097 = EDGE_CURVE ( 'NONE', #12285, #15984, #19725, .T. ) ;
#16098 = VERTEX_POINT ( 'NONE', #26608 ) ;
#16099 = CARTESIAN_POINT ( 'NONE',  ( 16.06085112851925345, -5.768724642094694488, 5.872146474157316831 ) ) ;
#16100 = AXIS2_PLACEMENT_3D ( 'NONE', #28286, #21401, #30765 ) ;
#16101 = CARTESIAN_POINT ( 'NONE',  ( -1.832066046471847676, 44.03802034382739805, -16.49999999999999645 ) ) ;
#16102 = ORIENTED_EDGE ( 'NONE', *, *, #551, .T. ) ;
#16103 = DIRECTION ( 'NONE',  ( -0.000000000000000000, -0.000000000000000000, 1.000000000000000000 ) ) ;
#16104 = DIRECTION ( 'NONE',  ( 0.000000000000000000, 1.000000000000000000, 0.000000000000000000 ) ) ;
#16105 = CARTESIAN_POINT ( 'NONE',  ( 3.912171961291952105, 8.637616862297853970, 21.50000000000000000 ) ) ;
#16106 = CARTESIAN_POINT ( 'NONE',  ( -25.32744450373244050, -23.23809170341762353, -16.50001200000000168 ) ) ;
#16107 = CARTESIAN_POINT ( 'NONE',  ( -33.01877980957529957, 12.12572312222180493, 35.60092001944732942 ) ) ;
#16108 = CYLINDRICAL_SURFACE ( 'NONE', #6848, 37.60050224823048381 ) ;
#16109 = CARTESIAN_POINT ( 'NONE',  ( -16.87834697512587212, 2.265528671477828215, 7.453286057244489449 ) ) ;
#16110 = VERTEX_POINT ( 'NONE', #8046 ) ;
#16111 = CARTESIAN_POINT ( 'NONE',  ( 5.738360882149947884, 7.548823014270664267, 21.50000000000000000 ) ) ;
#16112 = CYLINDRICAL_SURFACE ( 'NONE', #17277, 1.447898107987198646 ) ;
#16113 = ORIENTED_EDGE ( 'NONE', *, *, #4610, .T. ) ;
#16114 = FACE_OUTER_BOUND ( 'NONE', #8, .T. ) ;
#16115 = AXIS2_PLACEMENT_3D ( 'NONE', #15937, #29974, #30272 ) ;
#16116 = CARTESIAN_POINT ( 'NONE',  ( -17.99270058295304509, -8.773758909272052264, 18.35718225375110180 ) ) ;
#16117 = EDGE_CURVE ( 'NONE', #4652, #19850, #29248, .T. ) ;
#16118 = VECTOR ( 'NONE', #11247, 1000.000000000000000 ) ;
#16119 = CARTESIAN_POINT ( 'NONE',  ( 2.552544030762014415, -42.50000000000000000, -1.500000000000000000 ) ) ;
#16120 = EDGE_CURVE ( 'NONE', #23454, #8444, #7890, .T. ) ;
#16121 = CARTESIAN_POINT ( 'NONE',  ( 13.22505861668195237, -42.10773672056998862, -19.50000000000000355 ) ) ;
#16122 = EDGE_LOOP ( 'NONE', ( #29106, #25528, #9684, #17109 ) ) ;
#16123 = DIRECTION ( 'NONE',  ( 1.000000000000000000, 0.000000000000000000, 0.000000000000000000 ) ) ;
#16124 = DIRECTION ( 'NONE',  ( 1.000000000000000000, 0.000000000000000000, 0.000000000000000000 ) ) ;
#16125 = CARTESIAN_POINT ( 'NONE',  ( 11.91353211314439164, -35.56214078857726690, 37.49999999998971134 ) ) ;
#16126 = FACE_BOUND ( 'NONE', #27421, .T. ) ;
#16127 = ORIENTED_EDGE ( 'NONE', *, *, #968, .T. ) ;
#16128 = CARTESIAN_POINT ( 'NONE',  ( -4.163336342344337027E-14, 1.387778780781445676E-14, 24.50000000000000000 ) ) ;
#16129 = VERTEX_POINT ( 'NONE', #26921 ) ;
#16130 = CARTESIAN_POINT ( 'NONE',  ( -6.980328572437709767, 4.608906612435681005, -1.500000000000001332 ) ) ;
#16131 = FACE_OUTER_BOUND ( 'NONE', #936, .T. ) ;
#16132 = VERTEX_POINT ( 'NONE', #5235 ) ;
#16133 = B_SPLINE_SURFACE_WITH_KNOTS ( 'NONE', 3, 1, ( 
 ( #1432, #8290 ),
 ( #11233, #20729 ),
 ( #30260, #8907 ),
 ( #29963, #27932 ),
 ( #15447, #4206 ),
 ( #27320, #3763 ),
 ( #13730, #30109 ),
 ( #13282, #11088 ),
 ( #3926, #29653 ),
 ( #22620, #22776 ),
 ( #10947, #1270 ),
 ( #13446, #10778 ),
 ( #17806, #20584 ),
 ( #20292, #29819 ),
 ( #8601, #18109 ),
 ( #22929, #27624 ),
 ( #1581, #23221 ),
 ( #11691, #11548 ),
 ( #27354, #21038 ),
 ( #21180, #25888 ),
 ( #18569, #4979 ),
 ( #6852, #9199 ),
 ( #21347, #11850 ),
 ( #2323, #140 ),
 ( #19169, #9659 ),
 ( #18711, #30559 ),
 ( #25731, #28219 ),
 ( #26188, #28387 ),
 ( #9053, #9504 ),
 ( #16373, #7168 ),
 ( #1875, #28077 ) ),
 .UNSPECIFIED., .F., .F., .F.,
 ( 4, 3, 3, 3, 3, 3, 3, 3, 3, 3, 4 ),
 ( 2, 2 ),
 ( 0.000000000000000000, 0.05425176834609614362, 0.1085332949128348518, 0.1623767749169379715, 0.2157504826133058717, 0.2688657508888169789, 0.3218907763505471364, 0.3749548578363334772, 0.4282048033836237666, 0.4818374082110496448, 0.4999999999131653494 ),
 ( 0.000000000000000000, 1.000000000000000000 ),
 .UNSPECIFIED. ) ;
#16134 = CARTESIAN_POINT ( 'NONE',  ( -21.24416681158189135, -35.65075532067091757, 34.51006995843407310 ) ) ;
#16135 = ORIENTED_EDGE ( 'NONE', *, *, #16605, .F. ) ;
#16136 = CARTESIAN_POINT ( 'NONE',  ( -25.88640477275121654, -6.345529225273950580, 44.10491087709822011 ) ) ;
#16137 = AXIS2_PLACEMENT_3D ( 'NONE', #1635, #8962, #6611 ) ;
#16138 = CIRCLE ( 'NONE', #2688, 7.500000000000013323 ) ;
#16139 = CARTESIAN_POINT ( 'NONE',  ( -10.14013680258725358, -17.25966085745526968, 5.749491821935610147 ) ) ;
#16140 = CARTESIAN_POINT ( 'NONE',  ( -40.00000000000002842, 80.00000000000001421, 22.49999999999983302 ) ) ;
#16141 = ORIENTED_EDGE ( 'NONE', *, *, #4314, .F. ) ;
#16142 = CARTESIAN_POINT ( 'NONE',  ( 23.07491035053308437, 11.55692089822198554, 44.95040115375503120 ) ) ;
#16143 = CARTESIAN_POINT ( 'NONE',  ( 0.4564504349074350875, -9.471281197126604212, 13.00000000000000178 ) ) ;
#16144 = PLANE ( 'NONE',  #23691 ) ;
#16145 = CARTESIAN_POINT ( 'NONE',  ( 6.900000000000000355, 0.000000000000000000, 0.000000000000000000 ) ) ;
#16146 = CARTESIAN_POINT ( 'NONE',  ( 25.48568755041062062, -12.36160011285429583, 24.50000000000000000 ) ) ;
#16147 = PLANE ( 'NONE',  #25789 ) ;
#16148 = LINE ( 'NONE', #6487, #21998 ) ;
#16149 = CARTESIAN_POINT ( 'NONE',  ( 3.068634486552013207, 16.80010772488889614, 19.21769074125272780 ) ) ;
#16150 = CARTESIAN_POINT ( 'NONE',  ( -18.40637697828373121, -7.823545570387635983, 19.85261563089511228 ) ) ;
#16151 = B_SPLINE_CURVE_WITH_KNOTS ( 'NONE', 3,
 ( #12237, #21590, #7565, #19989, #223, #28931, #21738, #14581 ),
 .UNSPECIFIED., .F., .F.,
 ( 4, 2, 2, 4 ),
 ( 0.01498083277331300339, 0.01629713195395227077, 0.01761343113459154161, 0.02024602949587007983 ),
 .UNSPECIFIED. ) ;
#16152 = CARTESIAN_POINT ( 'NONE',  ( 4.221020697412598999, 42.26040651453248387, 28.86037875636509398 ) ) ;
#16153 = DIRECTION ( 'NONE',  ( 0.000000000000000000, 1.000000000000000000, 0.000000000000000000 ) ) ;
#16154 = ADVANCED_FACE ( 'NONE', ( #2744 ), #7736, .F. ) ;
#16155 = ORIENTED_EDGE ( 'NONE', *, *, #9417, .T. ) ;
#16156 = VERTEX_POINT ( 'NONE', #29411 ) ;
#16157 = LINE ( 'NONE', #23468, #20908 ) ;
#16158 = AXIS2_PLACEMENT_3D ( 'NONE', #17942, #20873, #16194 ) ;
#16159 = CARTESIAN_POINT ( 'NONE',  ( -7.785146467913381052, -15.19543897952354783, 6.147510495896840510 ) ) ;
#16160 = DIRECTION ( 'NONE',  ( 0.000000000000000000, 0.000000000000000000, 1.000000000000000000 ) ) ;
#16161 = ORIENTED_EDGE ( 'NONE', *, *, #22128, .F. ) ;
#16162 = DIRECTION ( 'NONE',  ( 1.000000000000000000, 0.000000000000000000, 0.000000000000000000 ) ) ;
#16163 = CARTESIAN_POINT ( 'NONE',  ( 15.48289691231202703, -7.082479268569363384, 18.71435384576123440 ) ) ;
#16164 = CARTESIAN_POINT ( 'NONE',  ( 4.155601639749240128, 16.52779251924068760, 5.657991946698900598 ) ) ;
#16165 = ORIENTED_EDGE ( 'NONE', *, *, #15880, .F. ) ;
#16166 = CARTESIAN_POINT ( 'NONE',  ( 22.58267429318974706, -26.57182937991349903, 1.500000000000000000 ) ) ;
#16167 = CARTESIAN_POINT ( 'NONE',  ( -25.48568755041063838, 12.36160011285429583, 1.500000000000000000 ) ) ;
#16168 = DIRECTION ( 'NONE',  ( 0.000000000000000000, -1.132880637372608986E-16, 1.000000000000000000 ) ) ;
#16169 = CARTESIAN_POINT ( 'NONE',  ( -24.03057240117691862, 26.57182937991348481, 26.54355021145562787 ) ) ;
#16170 = VERTEX_POINT ( 'NONE', #15042 ) ;
#16171 =( REPRESENTATION_RELATIONSHIP ('NONE','NONE', #19885, #28257 ) REPRESENTATION_RELATIONSHIP_WITH_TRANSFORMATION ( #20747 )SHAPE_REPRESENTATION_RELATIONSHIP( ) );
#16172 = CARTESIAN_POINT ( 'NONE',  ( 52.16608720827707657, -51.86186943028246787, 97.07879600563551037 ) ) ;
#16173 = CARTESIAN_POINT ( 'NONE',  ( -25.88604317058895177, 6.345278376181627600, 44.10533075955778770 ) ) ;
#16174 = CARTESIAN_POINT ( 'NONE',  ( -14.67633008511251091, 13.58695459845237075, 6.781503518395064489 ) ) ;
#16175 = ORIENTED_EDGE ( 'NONE', *, *, #20617, .T. ) ;
#16176 = VECTOR ( 'NONE', #2854, 1000.000000000000000 ) ;
#16177 = FACE_OUTER_BOUND ( 'NONE', #11541, .T. ) ;
#16178 = DIRECTION ( 'NONE',  ( -1.000000000000000000, 0.000000000000000000, 0.000000000000000000 ) ) ;
#16179 = CARTESIAN_POINT ( 'NONE',  ( 9.675133109038689838, -8.168544852422947145, 1.500000000000000000 ) ) ;
#16180 = FACE_BOUND ( 'NONE', #3858, .T. ) ;
#16181 = DIRECTION ( 'NONE',  ( 0.000000000000000000, 1.000000000000000000, 0.000000000000000000 ) ) ;
#16182 = DIRECTION ( 'NONE',  ( -0.000000000000000000, -0.000000000000000000, -1.000000000000000000 ) ) ;
#16183 = CARTESIAN_POINT ( 'NONE',  ( -19.95735252415838090, 1.552219945263927592, 19.69140814234746273 ) ) ;
#16184 = CARTESIAN_POINT ( 'NONE',  ( 15.57266529552203416, 38.96488032230103471, -1.500000000000000000 ) ) ;
#16185 = ORIENTED_EDGE ( 'NONE', *, *, #5594, .F. ) ;
#16186 = CARTESIAN_POINT ( 'NONE',  ( 10.38186781339405229, -13.54365823448425843, 20.13759033520874908 ) ) ;
#16187 = CARTESIAN_POINT ( 'NONE',  ( 34.83396020575241891, 10.30249279383515848, 27.50000000000001066 ) ) ;
#16188 = VERTEX_POINT ( 'NONE', #24556 ) ;
#16189 = ORIENTED_EDGE ( 'NONE', *, *, #27747, .T. ) ;
#16190 = LINE ( 'NONE', #4956, #16593 ) ;
#16191 = ADVANCED_FACE ( 'NONE', ( #14897 ), #396, .F. ) ;
#16192 = DIRECTION ( 'NONE',  ( 0.000000000000000000, 1.000000000000000000, -0.000000000000000000 ) ) ;
#16193 = ORIENTED_EDGE ( 'NONE', *, *, #9960, .T. ) ;
#16194 = DIRECTION ( 'NONE',  ( 0.000000000000000000, 1.000000000000000000, 0.000000000000000000 ) ) ;
#16195 = AXIS2_PLACEMENT_3D ( 'NONE', #21374, #25613, #21199 ) ;
#16196 = CYLINDRICAL_SURFACE ( 'NONE', #25881, 22.49999999999996447 ) ;
#16197 = EDGE_LOOP ( 'NONE', ( #428, #12578, #25618, #18624 ) ) ;
#16198 = FACE_OUTER_BOUND ( 'NONE', #2468, .T. ) ;
#16199 = DIRECTION ( 'NONE',  ( 1.000000000000000000, -0.000000000000000000, 0.000000000000000000 ) ) ;
#16200 = ORIENTED_EDGE ( 'NONE', *, *, #16237, .T. ) ;
#16201 = DIRECTION ( 'NONE',  ( 0.000000000000000000, 0.000000000000000000, 1.000000000000000000 ) ) ;
#16202 = VERTEX_POINT ( 'NONE', #15188 ) ;
#16203 = CARTESIAN_POINT ( 'NONE',  ( 7.500000000000000000, 10.39230484541327471, 0.000000000000000000 ) ) ;
#16204 = ORIENTED_EDGE ( 'NONE', *, *, #4110, .F. ) ;
#16205 = VERTEX_POINT ( 'NONE', #26760 ) ;
#16206 = CARTESIAN_POINT ( 'NONE',  ( -20.71335220384823117, -27.86167394782616213, -6.500000000000000888 ) ) ;
#16207 = CARTESIAN_POINT ( 'NONE',  ( -0.1008988851360398120, -17.02363397670899303, 18.83976166372256600 ) ) ;
#16208 = ADVANCED_BREP_SHAPE_REPRESENTATION ( '', ( #13239, #7396 ), #1419 ) ;
#16209 = EDGE_CURVE ( 'NONE', #30732, #2852, #5711, .T. ) ;
#16210 = VECTOR ( 'NONE', #13836, 1000.000000000000000 ) ;
#16211 = CARTESIAN_POINT ( 'NONE',  ( -0.1262659238204836554, -8.999114229549588728, -1.500000000000002665 ) ) ;
#16212 = CYLINDRICAL_SURFACE ( 'NONE', #16350, 0.7499999999999997780 ) ;
#16213 = EDGE_CURVE ( 'NONE', #24252, #1827, #12723, .T. ) ;
#16214 = ORIENTED_EDGE ( 'NONE', *, *, #26901, .F. ) ;
#16215 = ADVANCED_FACE ( 'NONE', ( #3352 ), #856, .F. ) ;
#16216 = CARTESIAN_POINT ( 'NONE',  ( -19.81665592078380200, 2.832673353242753933, 18.39701043959520987 ) ) ;
#16217 = CARTESIAN_POINT ( 'NONE',  ( -3.221450758838616757, 1.621276839356792454, 1.500000000000000000 ) ) ;
#16218 = CARTESIAN_POINT ( 'NONE',  ( -15.40257881337303481, 12.78582346615753629, 20.34789198813115263 ) ) ;
#16219 = CARTESIAN_POINT ( 'NONE',  ( 4.537370253389201302, 19.49663512434673507, 19.97651184436794125 ) ) ;
#16220 = EDGE_LOOP ( 'NONE', ( #3314, #15810, #8662, #6913 ) ) ;
#16221 = EDGE_LOOP ( 'NONE', ( #16904, #18451, #14817, #10879 ) ) ;
#16222 = FACE_OUTER_BOUND ( 'NONE', #20581, .T. ) ;
#16223 = DIRECTION ( 'NONE',  ( -0.000000000000000000, -0.000000000000000000, -1.000000000000000000 ) ) ;
#16224 = EDGE_CURVE ( 'NONE', #13283, #29319, #11700, .T. ) ;
#16225 = DIRECTION ( 'NONE',  ( -0.000000000000000000, -1.000000000000000000, -0.000000000000000000 ) ) ;
#16226 = CARTESIAN_POINT ( 'NONE',  ( -9.675133109038686285, -8.168544852422948921, 1.500000000000000000 ) ) ;
#16227 = VECTOR ( 'NONE', #7779, 1000.000000000000000 ) ;
#16228 = DIRECTION ( 'NONE',  ( -0.000000000000000000, -0.000000000000000000, 1.000000000000000000 ) ) ;
#16229 = CARTESIAN_POINT ( 'NONE',  ( -4.163336342344337027E-14, 1.387778780781445676E-14, 62.49999999999999289 ) ) ;
#16230 = EDGE_CURVE ( 'NONE', #27312, #10762, #1019, .T. ) ;
#16231 = ORIENTED_EDGE ( 'NONE', *, *, #12650, .T. ) ;
#16232 = CARTESIAN_POINT ( 'NONE',  ( -17.03551135121416849, 1.010186107319479554, 5.872146474157316831 ) ) ;
#16233 = ADVANCED_FACE ( 'NONE', ( #16933 ), #7580, .F. ) ;
#16234 = CARTESIAN_POINT ( 'NONE',  ( -35.78336344873367381, 4.414649291699865863, 34.71346399078494471 ) ) ;
#16235 = DIRECTION ( 'NONE',  ( -0.000000000000000000, -0.000000000000000000, 1.000000000000000000 ) ) ;
#16236 = VERTEX_POINT ( 'NONE', #24094 ) ;
#16237 = EDGE_CURVE ( 'NONE', #10573, #6567, #29094, .T. ) ;
#16238 = PLANE ( 'NONE',  #9829 ) ;
#16239 = ORIENTED_EDGE ( 'NONE', *, *, #26518, .F. ) ;
#16240 = CARTESIAN_POINT ( 'NONE',  ( 16.09309408545198039, -5.686824080536031722, 5.951255046771932733 ) ) ;
#16241 = AXIS2_PLACEMENT_3D ( 'NONE', #1096, #22141, #24635 ) ;
#16242 = CARTESIAN_POINT ( 'NONE',  ( -21.80735578196799196, 37.17533440937560840, -16.50000000000000000 ) ) ;
#16243 = ORIENTED_EDGE ( 'NONE', *, *, #201, .F. ) ;
#16244 = CARTESIAN_POINT ( 'NONE',  ( 7.730328572437743517, -4.608906612435629491, 21.50000000000000000 ) ) ;
#16245 = CARTESIAN_POINT ( 'NONE',  ( 77.99999999999998579, -42.50000000000002132, 1.500000000000001110 ) ) ;
#16246 = CARTESIAN_POINT ( 'NONE',  ( 23.21352257770656990, 10.78826658734920230, -16.55003854064094426 ) ) ;
#16247 = DIRECTION ( 'NONE',  ( 0.000000000000000000, 1.000000000000000000, 1.193512090021232842E-16 ) ) ;
#16248 = CARTESIAN_POINT ( 'NONE',  ( -5.615427697021304176, 16.09608755218562948, 20.34789198813115263 ) ) ;
#16249 = AXIS2_PLACEMENT_3D ( 'NONE', #24273, #28809, #21932 ) ;
#16250 = AXIS2_PLACEMENT_3D ( 'NONE', #6910, #1919, #9096 ) ;
#16251 = LINE ( 'NONE', #27967, #18594 ) ;
#16252 = CARTESIAN_POINT ( 'NONE',  ( -29.81954908927651360, 15.48017614753370985, 41.40177460054280800 ) ) ;
#16253 = EDGE_CURVE ( 'NONE', #8993, #25738, #17236, .T. ) ;
#16254 = VERTEX_POINT ( 'NONE', #17082 ) ;
#16255 = EDGE_CURVE ( 'NONE', #12567, #28158, #3049, .T. ) ;
#16256 = FACE_OUTER_BOUND ( 'NONE', #27684, .T. ) ;
#16257 = DIRECTION ( 'NONE',  ( 1.000000000000000000, 0.000000000000000000, 0.000000000000000000 ) ) ;
#16258 = EDGE_CURVE ( 'NONE', #2772, #27558, #4727, .T. ) ;
#16259 = EDGE_LOOP ( 'NONE', ( #8220, #11986, #5443, #27907 ) ) ;
#16260 = DIRECTION ( 'NONE',  ( 1.000000000000000000, 0.000000000000000000, -0.000000000000000000 ) ) ;
#16261 = AXIS2_PLACEMENT_3D ( 'NONE', #24902, #27089, #8539 ) ;
#16262 = CARTESIAN_POINT ( 'NONE',  ( -14.77047757180929466, -8.563270617688839792, 18.82680253904184298 ) ) ;
#16263 = CIRCLE ( 'NONE', #2821, 9.482273699623480212 ) ;
#16264 = EDGE_CURVE ( 'NONE', #11996, #12516, #12189, .T. ) ;
#16265 = CARTESIAN_POINT ( 'NONE',  ( -39.00000000000000000, 5.563236990218665134, -1.500000000000000000 ) ) ;
#16266 = AXIS2_PLACEMENT_3D ( 'NONE', #4729, #6198, #23910 ) ;
#16267 = CARTESIAN_POINT ( 'NONE',  ( 19.49999999999992539, 1.387778780781445676E-14, 51.25735931288069480 ) ) ;
#16268 = VERTEX_POINT ( 'NONE', #13031 ) ;
#16269 = CARTESIAN_POINT ( 'NONE',  ( 0.000000000000000000, 0.000000000000000000, 0.000000000000000000 ) ) ;
#16270 = CARTESIAN_POINT ( 'NONE',  ( 4.336808689942017736E-16, 42.50000000000000000, -1.500000000000000000 ) ) ;
#16271 = CARTESIAN_POINT ( 'NONE',  ( 28.82515617888658355, -28.76482263229141978, 34.54546745300068977 ) ) ;
#16272 = ADVANCED_FACE ( 'NONE', ( #1322 ), #17343, .T. ) ;
#16273 = CARTESIAN_POINT ( 'NONE',  ( -6.096671963363472280, 19.04856480014128195, 7.652108011868850035 ) ) ;
#16274 = ORIENTED_EDGE ( 'NONE', *, *, #16067, .T. ) ;
#16275 = B_SPLINE_CURVE_WITH_KNOTS ( 'NONE', 3,
 ( #297, #9819, #19333, #2185, #9209, #18441, #11703, #28235, #27943, #8919, #18119, #15771, #9064, #25601, #27635, #22940, #13457, #13741 ),
 .UNSPECIFIED., .F., .F.,
 ( 4, 2, 2, 2, 2, 2, 2, 2, 4 ),
 ( 0.003174295595554294403, 0.003570702171545527166, 0.003967108747536760363, 0.004363515323527992693, 0.004759921899519225889, 0.005156328475510459086, 0.005552735051501691416, 0.005949141627492923745, 0.006345548203484156942 ),
 .UNSPECIFIED. ) ;
#16276 = CARTESIAN_POINT ( 'NONE',  ( 20.71335220384823117, -27.86167394782616213, -6.500000000000000888 ) ) ;
#16277 = AXIS2_PLACEMENT_3D ( 'NONE', #3034, #2727, #12234 ) ;
#16278 = CARTESIAN_POINT ( 'NONE',  ( -5.105024945673440229, 42.22604126506271172, -1.500000000000000000 ) ) ;
#16279 = DIRECTION ( 'NONE',  ( 0.9594929736144952592, -0.2817325568414371095, 0.000000000000000000 ) ) ;
#16280 = VECTOR ( 'NONE', #7278, 1000.000000000000000 ) ;
#16281 = ORIENTED_EDGE ( 'NONE', *, *, #14489, .T. ) ;
#16282 = AXIS2_PLACEMENT_3D ( 'NONE', #30583, #23550, #13753 ) ;
#16283 = CARTESIAN_POINT ( 'NONE',  ( 16.16296542101254730, 5.939519782021115191, 1.500000000000000000 ) ) ;
#16284 = VERTEX_POINT ( 'NONE', #25799 ) ;
#16285 = DIRECTION ( 'NONE',  ( -0.000000000000000000, -0.000000000000000000, 1.000000000000000000 ) ) ;
#16286 = VECTOR ( 'NONE', #4237, 1000.000000000000000 ) ;
#16287 = ADVANCED_FACE ( 'NONE', ( #4265 ), #4724, .F. ) ;
#16288 = VECTOR ( 'NONE', #26225, 1000.000000000000000 ) ;
#16289 = CARTESIAN_POINT ( 'NONE',  ( -7.809214384344188353, -15.18204291278972029, 7.196036389296800451 ) ) ;
#16290 = EDGE_CURVE ( 'NONE', #21154, #15490, #29139, .T. ) ;
#16291 = CIRCLE ( 'NONE', #7810, 11.99999999999998224 ) ;
#16292 = CARTESIAN_POINT ( 'NONE',  ( -37.99999999999999289, 90.00000000000001421, -75.50000000000000000 ) ) ;
#16293 = LINE ( 'NONE', #25510, #5810 ) ;
#16294 = ORIENTED_EDGE ( 'NONE', *, *, #4808, .T. ) ;
#16295 = CARTESIAN_POINT ( 'NONE',  ( 18.64396409872436777, -7.239577540284316548, 7.272192800924339728 ) ) ;
#16296 = CARTESIAN_POINT ( 'NONE',  ( -4.163336342344337027E-14, 1.387778780781445676E-14, 1.500000000000000000 ) ) ;
#16297 = DIRECTION ( 'NONE',  ( -0.000000000000000000, 0.000000000000000000, 1.000000000000000000 ) ) ;
#16298 = CARTESIAN_POINT ( 'NONE',  ( -13.35701160122519404, 10.58771215013900857, 18.34777357837152323 ) ) ;
#16299 = VERTEX_POINT ( 'NONE', #6617 ) ;
#16300 = CARTESIAN_POINT ( 'NONE',  ( 9.041888939645136958, -0.8750451464062836138, 13.22130136205108819 ) ) ;
#16301 = CARTESIAN_POINT ( 'NONE',  ( 24.03057240117691862, -26.57182937991349903, -6.500000000000000888 ) ) ;
#16302 = DIRECTION ( 'NONE',  ( -0.000000000000000000, -0.000000000000000000, 1.000000000000000000 ) ) ;
#16303 = DIRECTION ( 'NONE',  ( 0.000000000000000000, -0.000000000000000000, -1.000000000000000000 ) ) ;
#16304 = CARTESIAN_POINT ( 'NONE',  ( 37.99999999999999289, 90.00000000000001421, -75.50000000000001421 ) ) ;
#16305 = CARTESIAN_POINT ( 'NONE',  ( -18.25569084301827161, -8.169747224523364437, 18.47110296274026098 ) ) ;
#16306 = CIRCLE ( 'NONE', #2858, 9.482273699623480212 ) ;
#16307 = CARTESIAN_POINT ( 'NONE',  ( -18.39183130958319978, -7.903152449895381793, 19.96783386855779341 ) ) ;
#16308 = DIRECTION ( 'NONE',  ( -0.9096319953545185522, 0.4154150130018859355, 0.000000000000000000 ) ) ;
#16309 = VECTOR ( 'NONE', #25573, 1000.000000000000000 ) ;
#16310 = ORIENTED_EDGE ( 'NONE', *, *, #24044, .T. ) ;
#16311 = ORIENTED_EDGE ( 'NONE', *, *, #21608, .F. ) ;
#16312 = AXIS2_PLACEMENT_3D ( 'NONE', #23633, #6807, #4313 ) ;
#16313 = DIRECTION ( 'NONE',  ( 0.000000000000000000, 0.000000000000000000, 1.000000000000000000 ) ) ;
#16314 = CARTESIAN_POINT ( 'NONE',  ( -7.695850205876553218, -15.24499612924144465, 6.917457548096560771 ) ) ;
#16315 = CARTESIAN_POINT ( 'NONE',  ( 0.000000000000000000, 42.50000000000000000, 24.50000000000000000 ) ) ;
#16316 = ORIENTED_EDGE ( 'NONE', *, *, #20649, .T. ) ;
#16317 = CARTESIAN_POINT ( 'NONE',  ( -50.00000000000000000, 50.00000000000000000, 70.00000000000000000 ) ) ;
#16318 = VECTOR ( 'NONE', #8109, 1000.000000000000000 ) ;
#16319 = CARTESIAN_POINT ( 'NONE',  ( -5.544451647051928944, 16.11829164193971664, 20.34789198813115263 ) ) ;
#16320 = CARTESIAN_POINT ( 'NONE',  ( 37.16608720827707657, 65.00000000000000000, 12.49999999999999112 ) ) ;
#16321 = AXIS2_PLACEMENT_3D ( 'NONE', #19729, #22389, #28949 ) ;
#16322 = ORIENTED_EDGE ( 'NONE', *, *, #13499, .T. ) ;
#16323 = CARTESIAN_POINT ( 'NONE',  ( -16.83986259902030014, 2.499865191129254871, 6.111214848085761986 ) ) ;
#16324 = CARTESIAN_POINT ( 'NONE',  ( 14.53258460577762889, 13.76634464516646617, 7.500147780736496017 ) ) ;
#16325 = AXIS2_PLACEMENT_3D ( 'NONE', #26115, #30632, #21435 ) ;
#16326 = CARTESIAN_POINT ( 'NONE',  ( -15.69194956178364109, -40.64901747633663831, -16.49999999999999645 ) ) ;
#16327 = CARTESIAN_POINT ( 'NONE',  ( -29.92052531042452301, 27.29380315016930325, 30.33179664086772576 ) ) ;
#16328 = VERTEX_POINT ( 'NONE', #11298 ) ;
#16329 = DIRECTION ( 'NONE',  ( 0.000000000000000000, 1.000000000000000000, 0.000000000000000000 ) ) ;
#16330 = CARTESIAN_POINT ( 'NONE',  ( -14.71865621671073932, -8.659590923291235143, 6.392658652357120275 ) ) ;
#16331 = CARTESIAN_POINT ( 'NONE',  ( -24.35970437652574105, -13.37404834226503070, 47.21042702067970254 ) ) ;
#16332 = VECTOR ( 'NONE', #4933, 1000.000000000000000 ) ;
#16333 = ADVANCED_FACE ( 'NONE', ( #28444 ), #23439, .F. ) ;
#16334 = ORIENTED_EDGE ( 'NONE', *, *, #4245, .F. ) ;
#16335 = CIRCLE ( 'NONE', #26226, 0.7500000000000002220 ) ;
#16336 = ADVANCED_FACE ( 'NONE', ( #9421 ), #14401, .F. ) ;
#16337 = CARTESIAN_POINT ( 'NONE',  ( 16.87629972246788768, 2.221555249144609334, 19.08155846658118904 ) ) ;
#16338 = DIRECTION ( 'NONE',  ( -0.000000000000000000, -0.000000000000000000, -1.000000000000000000 ) ) ;
#16339 = CARTESIAN_POINT ( 'NONE',  ( -2.931009552726342449, 14.22630671667915792, -1.500000000000000000 ) ) ;
#16340 = CARTESIAN_POINT ( 'NONE',  ( -57.50000000000001421, -50.00000000000000000, 62.49999999999999289 ) ) ;
#16341 = DIRECTION ( 'NONE',  ( 0.000000000000000000, 0.000000000000000000, -1.000000000000000000 ) ) ;
#16342 = CARTESIAN_POINT ( 'NONE',  ( 5.352643706120459477, 7.827050521741900191, 1.500000000000001332 ) ) ;
#16343 = LINE ( 'NONE', #18994, #26461 ) ;
#16344 = CARTESIAN_POINT ( 'NONE',  ( -9.406652940105978189, 1.195154792889487227, 21.50000000000000000 ) ) ;
#16345 = ORIENTED_EDGE ( 'NONE', *, *, #15276, .F. ) ;
#16346 = CIRCLE ( 'NONE', #13374, 0.7499999999999997780 ) ;
#16347 = VECTOR ( 'NONE', #6287, 1000.000000000000000 ) ;
#16348 = CARTESIAN_POINT ( 'NONE',  ( 11.89619695863782667, -16.09924856797056947, 19.69140814234746273 ) ) ;
#16349 = CARTESIAN_POINT ( 'NONE',  ( 9.268856789657291984, 38.25380398711768493, 34.80090346875810070 ) ) ;
#16350 = AXIS2_PLACEMENT_3D ( 'NONE', #16521, #18873, #14172 ) ;
#16351 = ORIENTED_EDGE ( 'NONE', *, *, #770, .T. ) ;
#16352 = ORIENTED_EDGE ( 'NONE', *, *, #18174, .F. ) ;
#16353 = CARTESIAN_POINT ( 'NONE',  ( -49.01087064057495724, 69.97702420031504289, 56.88420116493780654 ) ) ;
#16354 = CYLINDRICAL_SURFACE ( 'NONE', #13857, 7.500000000000000000 ) ;
#16355 = ORIENTED_EDGE ( 'NONE', *, *, #27689, .T. ) ;
#16356 = AXIS2_PLACEMENT_3D ( 'NONE', #8053, #10222, #10388 ) ;
#16357 = LINE ( 'NONE', #16962, #27116 ) ;
#16358 = SURFACE_STYLE_USAGE ( .BOTH. , #16814 ) ;
#16359 = VERTEX_POINT ( 'NONE', #7069 ) ;
#16360 = CARTESIAN_POINT ( 'NONE',  ( 8.430595340551262140, -4.340342926364987086, 1.500000000000001332 ) ) ;
#16361 = PLANE ( 'NONE',  #8518 ) ;
#16362 = VERTEX_POINT ( 'NONE', #28594 ) ;
#16363 = ORIENTED_EDGE ( 'NONE', *, *, #20994, .T. ) ;
#16364 = DIRECTION ( 'NONE',  ( -1.000000000000000000, -0.000000000000000000, -0.000000000000000000 ) ) ;
#16365 = CIRCLE ( 'NONE', #17346, 1.447898107987198646 ) ;
#16366 = ORIENTED_EDGE ( 'NONE', *, *, #6132, .T. ) ;
#16367 = AXIS2_PLACEMENT_3D ( 'NONE', #18396, #13247, #11052 ) ;
#16368 = VERTEX_POINT ( 'NONE', #16130 ) ;
#16369 = DIRECTION ( 'NONE',  ( 0.000000000000000000, 1.000000000000000000, 1.193512090021232842E-16 ) ) ;
#16370 = CARTESIAN_POINT ( 'NONE',  ( -0.02429396246983370547, -17.02566277816918117, 18.72771030977187934 ) ) ;
#16371 = DIRECTION ( 'NONE',  ( 0.000000000000000000, 1.132880637372608986E-16, -1.000000000000000000 ) ) ;
#16372 = CARTESIAN_POINT ( 'NONE',  ( -8.999114229549592281, 0.1262659238205133538, 1.500000000000001332 ) ) ;
#16373 = CARTESIAN_POINT ( 'NONE',  ( 19.76665705046225696, 3.161078882829539971, 18.34777357837152323 ) ) ;
#16374 = ORIENTED_EDGE ( 'NONE', *, *, #13979, .F. ) ;
#16375 = CARTESIAN_POINT ( 'NONE',  ( -19.86132377132436488, 2.497833445081384607, 18.34798005862930381 ) ) ;
#16376 = DIRECTION ( 'NONE',  ( 1.000000000000000000, 0.000000000000000000, 0.000000000000000000 ) ) ;
#16377 = DIRECTION ( 'NONE',  ( -0.000000000000000000, -0.000000000000000000, 1.000000000000000000 ) ) ;
#16378 = VERTEX_POINT ( 'NONE', #7218 ) ;
#16379 = EDGE_LOOP ( 'NONE', ( #17409, #30133, #817, #3932, #28049, #7401 ) ) ;
#16380 = CARTESIAN_POINT ( 'NONE',  ( -77.99999999999998579, 42.50000000000000711, 1.500000000000001110 ) ) ;
#16381 = DIRECTION ( 'NONE',  ( 0.000000000000000000, 0.000000000000000000, 1.000000000000000000 ) ) ;
#16382 = CARTESIAN_POINT ( 'NONE',  ( 64.99999999999998579, 36.86186943028246787, 57.49999999999999289 ) ) ;
#16383 = CYLINDRICAL_SURFACE ( 'NONE', #21315, 20.00000000000000000 ) ;
#16384 = LINE ( 'NONE', #26051, #8649 ) ;
#16385 = CIRCLE ( 'NONE', #23859, 3.559164065751841743 ) ;
#16386 = CARTESIAN_POINT ( 'NONE',  ( -24.41454739814620822, 29.13939308268315287, 27.50000000000000711 ) ) ;
#16387 = CARTESIAN_POINT ( 'NONE',  ( -5.000852292258042731, 19.36469665082833203, 6.781503518395070707 ) ) ;
#16388 = EDGE_LOOP ( 'NONE', ( #19392, #27950, #13061, #5278 ) ) ;
#16389 = CARTESIAN_POINT ( 'NONE',  ( -17.05973338880502865, 0.7261025713186443076, 6.233981582756856987 ) ) ;
#16390 = VECTOR ( 'NONE', #22177, 1000.000000000000000 ) ;
#16391 = CARTESIAN_POINT ( 'NONE',  ( 14.88222593340886668, 13.36111339922579866, 20.34789198813115263 ) ) ;
#16392 = CARTESIAN_POINT ( 'NONE',  ( -6.437683520590124608, 6.962021646281596254, 13.00000000000000178 ) ) ;
#16393 = VERTEX_POINT ( 'NONE', #27984 ) ;
#16394 = DIRECTION ( 'NONE',  ( -0.000000000000000000, -0.000000000000000000, 1.000000000000000000 ) ) ;
#16395 = ORIENTED_EDGE ( 'NONE', *, *, #12646, .T. ) ;
#16396 = PLANE ( 'NONE',  #14423 ) ;
#16397 = CARTESIAN_POINT ( 'NONE',  ( 11.10715495309693424, -16.63223102436629475, 20.34789198813115263 ) ) ;
#16398 = EDGE_CURVE ( 'NONE', #7304, #13794, #10208, .T. ) ;
#16399 = EDGE_LOOP ( 'NONE', ( #15088, #8291, #9992, #8075 ) ) ;
#16400 = CARTESIAN_POINT ( 'NONE',  ( 27.66896717189014510, 25.39816801983182515, 27.50000000000000355 ) ) ;
#16401 = CARTESIAN_POINT ( 'NONE',  ( 0.000000000000000000, 42.50000000000000000, 1.500000000000001332 ) ) ;
#16402 = EDGE_CURVE ( 'NONE', #26020, #11549, #11214, .T. ) ;
#16403 = CARTESIAN_POINT ( 'NONE',  ( 127.5000000000000000, 6.757601037695096551E-16, -5.035999999999999588 ) ) ;
#16404 = CARTESIAN_POINT ( 'NONE',  ( -18.25684187146043413, -8.167166100028891762, 7.526993102356321685 ) ) ;
#16405 = LINE ( 'NONE', #25920, #25293 ) ;
#16406 = DIRECTION ( 'NONE',  ( 1.000000000000000000, 0.000000000000000000, 0.000000000000000000 ) ) ;
#16407 = CARTESIAN_POINT ( 'NONE',  ( -32.28307784207223108, 8.475829241206282560, -16.55003854064094426 ) ) ;
#16408 = CARTESIAN_POINT ( 'NONE',  ( -6.187077094091591789, 11.47693674426096955, 24.50000000000000000 ) ) ;
#16409 = EDGE_CURVE ( 'NONE', #21650, #28935, #14180, .T. ) ;
#16410 = ORIENTED_EDGE ( 'NONE', *, *, #1327, .T. ) ;
#16411 = CARTESIAN_POINT ( 'NONE',  ( 15.38599937579231103, -7.279790735017091841, 6.714907520933426355 ) ) ;
#16412 = AXIS2_PLACEMENT_3D ( 'NONE', #19155, #21017, #26169 ) ;
#16413 = EDGE_CURVE ( 'NONE', #13876, #27501, #27594, .T. ) ;
#16414 = DIRECTION ( 'NONE',  ( -1.000000000000000000, 0.000000000000000000, 0.000000000000000000 ) ) ;
#16415 = DIRECTION ( 'NONE',  ( 0.000000000000000000, -1.132880637372608986E-16, 1.000000000000000000 ) ) ;
#16416 = ORIENTED_EDGE ( 'NONE', *, *, #4806, .T. ) ;
#16417 = DIRECTION ( 'NONE',  ( -0.000000000000000000, 1.132880637372608986E-16, -1.000000000000000000 ) ) ;
#16418 = ADVANCED_FACE ( 'NONE', ( #10336 ), #17512, .F. ) ;
#16419 = CARTESIAN_POINT ( 'NONE',  ( -18.06093561247158519, -8.632161831585831280, 20.34789198813115263 ) ) ;
#16420 = DIRECTION ( 'NONE',  ( 1.000000000000000000, 0.000000000000000000, 0.000000000000000000 ) ) ;
#16421 = CARTESIAN_POINT ( 'NONE',  ( -4.138038291653009905E-15, 8.014718854569428785, 4.118099735505521330 ) ) ;
#16422 = VECTOR ( 'NONE', #6641, 1000.000000000000000 ) ;
#16423 = CARTESIAN_POINT ( 'NONE',  ( 37.16608720827707657, 65.00000000000000000, 97.07879600563551037 ) ) ;
#16424 = ORIENTED_EDGE ( 'NONE', *, *, #8311, .T. ) ;
#16425 = CARTESIAN_POINT ( 'NONE',  ( 2.352830851074115159, 9.185733585337917617, 21.50000000000000000 ) ) ;
#16426 = DIRECTION ( 'NONE',  ( -0.000000000000000000, -0.000000000000000000, 1.000000000000000000 ) ) ;
#16427 = CARTESIAN_POINT ( 'NONE',  ( 23.42821736844243929, -34.00757704900313172, 29.63783715387382856 ) ) ;
#16428 = DIRECTION ( 'NONE',  ( -0.000000000000000000, -0.000000000000000000, -1.000000000000000000 ) ) ;
#16429 = ORIENTED_EDGE ( 'NONE', *, *, #23033, .T. ) ;
#16430 = CARTESIAN_POINT ( 'NONE',  ( -13.93204262646994529, 9.869472133046889084, 7.158811349119583944 ) ) ;
#16431 = DIRECTION ( 'NONE',  ( -0.3598999890241668664, 0.9329908884337534403, 0.000000000000000000 ) ) ;
#16432 = FACE_OUTER_BOUND ( 'NONE', #21744, .T. ) ;
#16433 = ORIENTED_EDGE ( 'NONE', *, *, #4203, .T. ) ;
#16434 = EDGE_CURVE ( 'NONE', #24153, #18657, #1574, .T. ) ;
#16435 = ORIENTED_EDGE ( 'NONE', *, *, #18571, .F. ) ;
#16436 = ADVANCED_FACE ( 'NONE', ( #29055 ), #24518, .F. ) ;
#16437 = CARTESIAN_POINT ( 'NONE',  ( 8.840471615930072247, -1.687027447297460236, 21.50000000000000000 ) ) ;
#16438 = EDGE_CURVE ( 'NONE', #27530, #23584, #15163, .T. ) ;
#16439 = VECTOR ( 'NONE', #4088, 1000.000000000000000 ) ;
#16440 = ORIENTED_EDGE ( 'NONE', *, *, #4209, .F. ) ;
#16441 = CARTESIAN_POINT ( 'NONE',  ( 0.2430132208050651554, -17.02994525543106263, 18.49267272388512140 ) ) ;
#16442 = EDGE_CURVE ( 'NONE', #8763, #16733, #1727, .T. ) ;
#16443 = CARTESIAN_POINT ( 'NONE',  ( -9.833673822381062024, -17.43574673801737163, 6.041646659195333058 ) ) ;
#16444 = DIRECTION ( 'NONE',  ( 0.000000000000000000, -1.000000000000000000, 0.000000000000000000 ) ) ;
#16445 = CARTESIAN_POINT ( 'NONE',  ( 0.7902931953360861073, -20.00234323981188922, 20.25542030744407640 ) ) ;
#16446 = VERTEX_POINT ( 'NONE', #813 ) ;
#16447 = EDGE_CURVE ( 'NONE', #16170, #26054, #21877, .T. ) ;
#16448 = CARTESIAN_POINT ( 'NONE',  ( 18.71865409427298843, -7.043577866502358731, 6.523620417364442758 ) ) ;
#16449 = CARTESIAN_POINT ( 'NONE',  ( 4.390207617113956573, -7.856594496258208160, 1.500000000000001332 ) ) ;
#16450 = CARTESIAN_POINT ( 'NONE',  ( 11.66141461333273099, 12.47704237144457551, 19.47783254395485031 ) ) ;
#16451 = CYLINDRICAL_SURFACE ( 'NONE', #19115, 0.7499999999999997780 ) ;
#16452 = EDGE_CURVE ( 'NONE', #5107, #22385, #662, .T. ) ;
#16453 = VERTEX_POINT ( 'NONE', #7697 ) ;
#16454 = DIRECTION ( 'NONE',  ( 1.000000000000000000, 0.000000000000000000, 0.000000000000000000 ) ) ;
#16455 = CARTESIAN_POINT ( 'NONE',  ( -12.97606618386100585, 11.02883152172955938, 18.54473042795395443 ) ) ;
#16456 = CARTESIAN_POINT ( 'NONE',  ( 69.99999999999998579, 50.00000000000000000, 59.49999999999999289 ) ) ;
#16457 = CARTESIAN_POINT ( 'NONE',  ( 4.045242219987651211, 16.55840560649980731, 18.34798005863078885 ) ) ;
#16458 = LINE ( 'NONE', #8987, #963 ) ;
#16459 = DIRECTION ( 'NONE',  ( -0.6548607339452851006, -0.7557495743542582689, 0.000000000000000000 ) ) ;
#16460 = AXIS2_PLACEMENT_3D ( 'NONE', #2947, #22420, #17443 ) ;
#16461 = DIRECTION ( 'NONE',  ( 0.000000000000000000, 0.000000000000000000, 1.000000000000000000 ) ) ;
#16462 = VERTEX_POINT ( 'NONE', #19389 ) ;
#16463 = ORIENTED_EDGE ( 'NONE', *, *, #4260, .F. ) ;
#16464 = DIRECTION ( 'NONE',  ( 0.000000000000000000, 0.000000000000000000, 1.000000000000000000 ) ) ;
#16465 = CARTESIAN_POINT ( 'NONE',  ( -8.546423435383420752, -14.74799740001550141, 5.652196082368483587 ) ) ;
#16466 = EDGE_CURVE ( 'NONE', #10973, #26160, #27032, .T. ) ;
#16467 = CARTESIAN_POINT ( 'NONE',  ( -13.88429941593315853, -16.69721919944146649, 1.500000000000000000 ) ) ;
#16468 = CARTESIAN_POINT ( 'NONE',  ( 11.22181534970139083, -16.55562029408562807, 18.34869673959212122 ) ) ;
#16469 = ORIENTED_EDGE ( 'NONE', *, *, #16645, .F. ) ;
#16470 = CARTESIAN_POINT ( 'NONE',  ( -6.812559277181930106, 5.881244434206302607, 1.500000000000001332 ) ) ;
#16471 = CARTESIAN_POINT ( 'NONE',  ( 6.124711512895117060, 19.05797279266333888, 6.111214848085761986 ) ) ;
#16472 = EDGE_CURVE ( 'NONE', #10292, #27407, #2552, .T. ) ;
#16473 = VERTEX_POINT ( 'NONE', #12064 ) ;
#16474 = CARTESIAN_POINT ( 'NONE',  ( 4.964892671625812604, 16.28226395658651171, 19.00652017443069752 ) ) ;
#16475 = EDGE_CURVE ( 'NONE', #28836, #8257, #13201, .T. ) ;
#16476 = CARTESIAN_POINT ( 'NONE',  ( 11.65981318837299341, 12.47865322263302978, 6.672349528511551497 ) ) ;
#16477 = DIRECTION ( 'NONE',  ( -0.2817325568414293380, -0.9594929736144974797, 0.000000000000000000 ) ) ;
#16478 = CARTESIAN_POINT ( 'NONE',  ( -29.47411470116815835, 23.31420789013893824, 37.50000000004725109 ) ) ;
#16479 = EDGE_LOOP ( 'NONE', ( #11072, #4236, #6065, #29320 ) ) ;
#16480 = CARTESIAN_POINT ( 'NONE',  ( 0.000000000000000000, 0.000000000000000000, -11.49999999999999645 ) ) ;
#16481 = AXIS2_PLACEMENT_3D ( 'NONE', #20506, #25181, #22678 ) ;
#16482 = DIRECTION ( 'NONE',  ( -0.000000000000000000, -0.000000000000000000, 1.000000000000000000 ) ) ;
#16483 = AXIS2_PLACEMENT_3D ( 'NONE', #18177, #27683, #6311 ) ;
#16484 = DIRECTION ( 'NONE',  ( -0.000000000000000000, -0.000000000000000000, 1.000000000000000000 ) ) ;
#16485 = VERTEX_POINT ( 'NONE', #9711 ) ;
#16486 = DIRECTION ( 'NONE',  ( -1.000000000000000000, 0.000000000000000000, 0.000000000000000000 ) ) ;
#16487 = DIRECTION ( 'NONE',  ( -0.000000000000000000, -0.000000000000000000, 1.000000000000000000 ) ) ;
#16488 = CARTESIAN_POINT ( 'NONE',  ( 26.58597676761595352, -6.321098805557485711, 43.43030304422416066 ) ) ;
#16489 = CARTESIAN_POINT ( 'NONE',  ( 23.27838111857050407, -36.10018641471199174, -16.50000599999999906 ) ) ;
#16490 = CARTESIAN_POINT ( 'NONE',  ( -0.02177409673011703947, -17.02558975896787885, 7.272049892295485485 ) ) ;
#16491 = CARTESIAN_POINT ( 'NONE',  ( 26.81381729043377860, -6.366069288663353198, 47.44085139292776887 ) ) ;
#16492 = CARTESIAN_POINT ( 'NONE',  ( 1.734723475976807094E-15, 44.07656352898514740, -6.500000000000000888 ) ) ;
#16493 = CARTESIAN_POINT ( 'NONE',  ( -17.04208893090348198, 0.9369385374313018433, 20.06253562465620632 ) ) ;
#16494 = DIRECTION ( 'NONE',  ( 0.7071067811865487940, 0.000000000000000000, -0.7071067811865463515 ) ) ;
#16495 = ORIENTED_EDGE ( 'NONE', *, *, #28412, .F. ) ;
#16496 = CARTESIAN_POINT ( 'NONE',  ( -6.507549961782351566, 15.78987431823413168, 6.588756557121048907 ) ) ;
#16497 = CARTESIAN_POINT ( 'NONE',  ( -8.249114229549590505, 0.1262659238205133538, 21.50000000000000000 ) ) ;
#16498 = ORIENTED_EDGE ( 'NONE', *, *, #22144, .T. ) ;
#16499 = ORIENTED_EDGE ( 'NONE', *, *, #207, .T. ) ;
#16500 = LINE ( 'NONE', #28665, #159 ) ;
#16501 = EDGE_CURVE ( 'NONE', #23899, #10056, #3058, .T. ) ;
#16502 = SHAPE_REPRESENTATION_RELATIONSHIP ( 'NONE' , 'NONE' ,  #12322, #16208 ) ;
#16503 = EDGE_LOOP ( 'NONE', ( #5023, #9902, #9300, #26586 ) ) ;
#16504 =( BOUNDED_CURVE ( )  B_SPLINE_CURVE ( 3, ( #19818, #26535, #5316, #26686 ),
 .UNSPECIFIED., .F., .T. ) 
 B_SPLINE_CURVE_WITH_KNOTS ( ( 4, 4 ),
 ( 3.141592653589793116, 6.283185307179586232 ),
 .UNSPECIFIED. ) 
 CURVE ( )  GEOMETRIC_REPRESENTATION_ITEM ( )  RATIONAL_B_SPLINE_CURVE ( ( 1.000000000000000000, 0.3333333333333333703, 0.3333333333333333703, 1.000000000000000000 ) ) 
 REPRESENTATION_ITEM ( '' )  );
#16505 = CARTESIAN_POINT ( 'NONE',  ( -1.897971151300065476E-14, 80.00000000000000000, 22.49999999999999289 ) ) ;
#16506 = ORIENTED_EDGE ( 'NONE', *, *, #2539, .F. ) ;
#16507 = CARTESIAN_POINT ( 'NONE',  ( 18.69797757513549996, -7.147916136757722860, 19.79423548914561692 ) ) ;
#16508 = CARTESIAN_POINT ( 'NONE',  ( 16.57326105224177581, 4.109591991357616436, 18.92976555901915603 ) ) ;
#16509 = CARTESIAN_POINT ( 'NONE',  ( -50.00000000000000000, 70.00000000000000000, 52.49999999999999289 ) ) ;
#16510 = ORIENTED_EDGE ( 'NONE', *, *, #24351, .F. ) ;
#16511 = ORIENTED_EDGE ( 'NONE', *, *, #5276, .F. ) ;
#16512 = AXIS2_PLACEMENT_3D ( 'NONE', #7326, #11546, #18709 ) ;
#16513 = EDGE_LOOP ( 'NONE', ( #28986, #21677, #30584, #4913 ) ) ;
#16514 = VERTEX_POINT ( 'NONE', #17042 ) ;
#16515 = DIRECTION ( 'NONE',  ( -1.000000000000000000, 0.000000000000000000, 0.000000000000000000 ) ) ;
#16516 = CARTESIAN_POINT ( 'NONE',  ( 0.1595703637281291887, -17.02896808596822709, 20.14907003336613300 ) ) ;
#16517 = AXIS2_PLACEMENT_3D ( 'NONE', #101, #4769, #23795 ) ;
#16518 = CARTESIAN_POINT ( 'NONE',  ( 1.780236034000288736, -16.98472935612792156, 6.447548852708279377 ) ) ;
#16519 = DIRECTION ( 'NONE',  ( 1.000000000000000000, 0.000000000000000000, 0.000000000000000000 ) ) ;
#16520 = CARTESIAN_POINT ( 'NONE',  ( 7.028330626922776325, 10.93629592680536966, 1.500000000000001332 ) ) ;
#16521 = CARTESIAN_POINT ( 'NONE',  ( 2.959227181723801170, -8.499586724479446076, 1.500000000000001332 ) ) ;
#16522 = ORIENTED_EDGE ( 'NONE', *, *, #13837, .T. ) ;
#16523 = DIRECTION ( 'NONE',  ( -0.000000000000000000, -0.000000000000000000, -1.000000000000000000 ) ) ;
#16524 = CARTESIAN_POINT ( 'NONE',  ( 18.22691194910808576, -34.07746802688367893, 34.49999999999999289 ) ) ;
#16525 = FACE_OUTER_BOUND ( 'NONE', #6952, .T. ) ;
#16526 = DIRECTION ( 'NONE',  ( 0.000000000000000000, 0.000000000000000000, 1.000000000000000000 ) ) ;
#16527 = ORIENTED_EDGE ( 'NONE', *, *, #23679, .F. ) ;
#16528 = ORIENTED_EDGE ( 'NONE', *, *, #22090, .T. ) ;
#16529 = FACE_OUTER_BOUND ( 'NONE', #26100, .T. ) ;
#16530 = CARTESIAN_POINT ( 'NONE',  ( -29.55332031600174858, 27.89853503084644260, -1.500000000000009992 ) ) ;
#16531 = CARTESIAN_POINT ( 'NONE',  ( -39.52380524535560369, 7.028748154183623420, -11.49999999999999645 ) ) ;
#16532 = CARTESIAN_POINT ( 'NONE',  ( -5.978582851986702806, 19.10413308555695622, 18.34798005862930381 ) ) ;
#16533 = CARTESIAN_POINT ( 'NONE',  ( -6.482337650448453559, -6.364020599487773211, 21.50000000000000000 ) ) ;
#16534 = CARTESIAN_POINT ( 'NONE',  ( -27.75715622479468081, 2.303929616531696922E-16, 24.50000000000000000 ) ) ;
#16535 = VERTEX_POINT ( 'NONE', #16897 ) ;
#16536 = AXIS2_PLACEMENT_3D ( 'NONE', #2865, #22353, #17367 ) ;
#16537 = CARTESIAN_POINT ( 'NONE',  ( -17.01545599012841237, 1.214108451629968055, 7.559636331181775581 ) ) ;
#16538 = LINE ( 'NONE', #14043, #3760 ) ;
#16539 = CARTESIAN_POINT ( 'NONE',  ( 6.962021646281529641, 6.437683520590196551, 21.50000000000000000 ) ) ;
#16540 = ORIENTED_EDGE ( 'NONE', *, *, #15877, .F. ) ;
#16541 = DIRECTION ( 'NONE',  ( 0.000000000000000000, 1.000000000000000000, 1.193512090021232842E-16 ) ) ;
#16542 = ORIENTED_EDGE ( 'NONE', *, *, #20992, .T. ) ;
#16543 = EDGE_CURVE ( 'NONE', #13000, #3499, #14554, .T. ) ;
#16544 = DIRECTION ( 'NONE',  ( 0.000000000000000000, 0.000000000000000000, -1.000000000000000000 ) ) ;
#16545 = DIRECTION ( 'NONE',  ( 0.000000000000000000, 0.000000000000000000, 1.000000000000000000 ) ) ;
#16546 = ORIENTED_EDGE ( 'NONE', *, *, #17216, .T. ) ;
#16547 = CARTESIAN_POINT ( 'NONE',  ( 30.94848640118418714, 20.21248784850468638, 27.49999999999999289 ) ) ;
#16548 = CARTESIAN_POINT ( 'NONE',  ( 4.851918296810534770, 49.76630973909864508, -40.79771880416375751 ) ) ;
#16549 = VECTOR ( 'NONE', #7289, 1000.000000000000000 ) ;
#16550 = DIRECTION ( 'NONE',  ( -1.000000000000000000, 0.000000000000000000, 0.000000000000000000 ) ) ;
#16551 = CARTESIAN_POINT ( 'NONE',  ( -15.16307827826492449, -7.786259562520723598, 18.34798005863078885 ) ) ;
#16552 = CARTESIAN_POINT ( 'NONE',  ( -6.426383236738485216, 15.81971323177987898, 18.92976555901915603 ) ) ;
#16553 = DIRECTION ( 'NONE',  ( 0.000000000000000000, -0.000000000000000000, -1.000000000000000000 ) ) ;
#16554 = LINE ( 'NONE', #16408, #402 ) ;
#16555 = ORIENTED_EDGE ( 'NONE', *, *, #20251, .F. ) ;
#16556 = CARTESIAN_POINT ( 'NONE',  ( 15.81223572262637589, -6.365019322297389870, 7.652108011868850923 ) ) ;
#16557 = CARTESIAN_POINT ( 'NONE',  ( 39.00000000000000000, -5.563236990218592304, -1.500000000000000000 ) ) ;
#16558 = LINE ( 'NONE', #14211, #20760 ) ;
#16559 = ADVANCED_FACE ( 'NONE', ( #26715 ), #26568, .F. ) ;
#16560 = ORIENTED_EDGE ( 'NONE', *, *, #15638, .T. ) ;
#16561 = CARTESIAN_POINT ( 'NONE',  ( 0.000000000000000000, 0.000000000000000000, -87.50000000000000000 ) ) ;
#16562 = DIRECTION ( 'NONE',  ( -1.000000000000000000, 0.000000000000000000, 0.000000000000000000 ) ) ;
#16563 = LINE ( 'NONE', #28432, #11742 ) ;
#16564 = DIRECTION ( 'NONE',  ( 0.000000000000000000, -1.132880637372608986E-16, 1.000000000000000000 ) ) ;
#16565 = FACE_OUTER_BOUND ( 'NONE', #4958, .T. ) ;
#16566 = VERTEX_POINT ( 'NONE', #24673 ) ;
#16567 = DIRECTION ( 'NONE',  ( 0.000000000000000000, -1.132880637372608986E-16, 1.000000000000000000 ) ) ;
#16568 = VECTOR ( 'NONE', #7321, 1000.000000000000000 ) ;
#16569 = EDGE_CURVE ( 'NONE', #28836, #154, #3782, .T. ) ;
#16570 = DIRECTION ( 'NONE',  ( -0.000000000000000000, -0.000000000000000000, 1.000000000000000000 ) ) ;
#16571 = CARTESIAN_POINT ( 'NONE',  ( 29.66037709627321917, 27.60437511129337196, 30.29918945543065334 ) ) ;
#16572 = EDGE_CURVE ( 'NONE', #10874, #7455, #15699, .T. ) ;
#16574 = VECTOR ( 'NONE', #7567, 1000.000000000000000 ) ;
#16573 = DIRECTION ( 'NONE',  ( 1.000000000000000000, 0.000000000000000000, 0.000000000000000000 ) ) ;
#16575 = ORIENTED_EDGE ( 'NONE', *, *, #1567, .F. ) ;
#16576 = DIRECTION ( 'NONE',  ( 1.000000000000000000, 0.000000000000000000, 0.000000000000000000 ) ) ;
#16577 = ORIENTED_EDGE ( 'NONE', *, *, #21570, .F. ) ;
#16578 = CARTESIAN_POINT ( 'NONE',  ( -31.18700685316050780, 26.11823559932051353, -1.500000000000000000 ) ) ;
#16579 = LINE ( 'NONE', #26716, #6003 ) ;
#16580 = B_SPLINE_CURVE_WITH_KNOTS ( 'NONE', 3,
 ( #10626, #19986, #790, #643, #17648, #2833, #5792, #24348, #29505, #5488, #8141, #21859 ),
 .UNSPECIFIED., .F., .F.,
 ( 4, 2, 2, 2, 2, 4 ),
 ( 2.975219550396606016E-07, 0.0009689891316535842632, 0.001937680741352128993, 0.002906372351050673722, 0.003390718155899950965, 0.003875063960749227775 ),
 .UNSPECIFIED. ) ;
#16581 = EDGE_LOOP ( 'NONE', ( #27940, #6860 ) ) ;
#16582 = VERTEX_POINT ( 'NONE', #29521 ) ;
#16583 = DIRECTION ( 'NONE',  ( 0.000000000000000000, 0.000000000000000000, 1.000000000000000000 ) ) ;
#16584 = ORIENTED_EDGE ( 'NONE', *, *, #6530, .T. ) ;
#16585 = ORIENTED_EDGE ( 'NONE', *, *, #12452, .F. ) ;
#16586 = CARTESIAN_POINT ( 'NONE',  ( -0.07785784566753434222, -17.02422498921964689, 18.80699882434806369 ) ) ;
#16587 = EDGE_CURVE ( 'NONE', #7713, #14972, #23657, .T. ) ;
#16588 = CARTESIAN_POINT ( 'NONE',  ( -8.172867764805141988, -14.97344430594796272, 7.559636331181775581 ) ) ;
#16589 = CARTESIAN_POINT ( 'NONE',  ( -33.62559477039935985, 21.53957619641537491, 17.96845262558712975 ) ) ;
#16590 = CARTESIAN_POINT ( 'NONE',  ( 1.797484530300065053, -16.98352104300882459, 19.25672174529527325 ) ) ;
#16591 = ORIENTED_EDGE ( 'NONE', *, *, #9602, .F. ) ;
#16592 = CARTESIAN_POINT ( 'NONE',  ( 32.82330813384650270, 22.94799032727486932, -1.500000000000000000 ) ) ;
#16593 = VECTOR ( 'NONE', #14008, 1000.000000000000000 ) ;
#16594 = CYLINDRICAL_SURFACE ( 'NONE', #14866, 4.999999999999997335 ) ;
#16595 = CARTESIAN_POINT ( 'NONE',  ( 14.26939381558975839, 14.03892697587676963, 19.79423548914561692 ) ) ;
#16596 = PLANE ( 'NONE',  #13655 ) ;
#16597 = VERTEX_POINT ( 'NONE', #25138 ) ;
#16598 = CIRCLE ( 'NONE', #3162, 9.084132297865673777 ) ;
#16599 = EDGE_CURVE ( 'NONE', #21613, #6566, #7242, .T. ) ;
#16600 = DIRECTION ( 'NONE',  ( 0.000000000000000000, 0.000000000000000000, 1.000000000000000000 ) ) ;
#16601 = CARTESIAN_POINT ( 'NONE',  ( -14.87733195063809966, -8.360270151095063440, 5.872146474157316831 ) ) ;
#16602 = CARTESIAN_POINT ( 'NONE',  ( 7.827050521741877098, -5.352643706120495004, 13.00000000000000178 ) ) ;
#16603 = CARTESIAN_POINT ( 'NONE',  ( -23.07950435457407679, -11.50806656539752737, 49.21048435262065368 ) ) ;
#16604 = CARTESIAN_POINT ( 'NONE',  ( -18.45589647530844957, -7.705834498630346197, 19.47728749465736442 ) ) ;
#16605 = EDGE_CURVE ( 'NONE', #10893, #4652, #3313, .T. ) ;
#16606 = AXIS2_PLACEMENT_3D ( 'NONE', #30463, #30772, #23134 ) ;
#16607 = EDGE_CURVE ( 'NONE', #30448, #20257, #21265, .T. ) ;
#16608 = CARTESIAN_POINT ( 'NONE',  ( 9.864937699929955173, -13.90063973435163724, 5.652196082368482699 ) ) ;
#16609 = DIRECTION ( 'NONE',  ( 1.000000000000000000, 0.000000000000000000, -0.000000000000000000 ) ) ;
#16610 = ORIENTED_EDGE ( 'NONE', *, *, #28026, .F. ) ;
#16611 = ORIENTED_EDGE ( 'NONE', *, *, #29046, .F. ) ;
#16612 = LINE ( 'NONE', #18358, #6967 ) ;
#16613 = ADVANCED_FACE ( 'NONE', ( #20608 ), #25166, .T. ) ;
#16614 = CARTESIAN_POINT ( 'NONE',  ( -23.96732207938974213, -33.98584080153308662, -1.500000000000000000 ) ) ;
#16615 = CARTESIAN_POINT ( 'NONE',  ( 0.1262659238204208167, 8.999114229549594057, -1.500000000000000888 ) ) ;
#16616 = EDGE_CURVE ( 'NONE', #12630, #15107, #9228, .T. ) ;
#16617 = CARTESIAN_POINT ( 'NONE',  ( 11.93826604606910990, -16.04611492155650865, 19.48477075383301127 ) ) ;
#16618 = VERTEX_POINT ( 'NONE', #24986 ) ;
#16619 =( NAMED_UNIT ( * ) PLANE_ANGLE_UNIT ( ) SI_UNIT ( $, .RADIAN. ) );
#16620 = AXIS2_PLACEMENT_3D ( 'NONE', #28072, #28214, #6697 ) ;
#16621 = CARTESIAN_POINT ( 'NONE',  ( -5.796781398543691566, 16.03935303270020185, 20.34789198813114552 ) ) ;
#16622 = CARTESIAN_POINT ( 'NONE',  ( 6.218621694205430650, 19.02754758079138853, 6.310736198168394928 ) ) ;
#16623 = EDGE_CURVE ( 'NONE', #4949, #13171, #20001, .T. ) ;
#16624 = AXIS2_PLACEMENT_3D ( 'NONE', #19178, #16381, #2648 ) ;
#16625 = ADVANCED_FACE ( 'NONE', ( #3478 ), #20317, .T. ) ;
#16626 = ORIENTED_EDGE ( 'NONE', *, *, #2561, .F. ) ;
#16627 = CIRCLE ( 'NONE', #5615, 0.7499999999999988898 ) ;
#16628 = CARTESIAN_POINT ( 'NONE',  ( 5.997818345539173812, 19.09841206584651729, 20.05479082170252525 ) ) ;
#16629 = CARTESIAN_POINT ( 'NONE',  ( 14.19872765237045087, 14.11031447301239616, 6.672349528511551497 ) ) ;
#16630 = EDGE_CURVE ( 'NONE', #9405, #29550, #20687, .T. ) ;
#16631 = FACE_OUTER_BOUND ( 'NONE', #25118, .T. ) ;
#16632 = CARTESIAN_POINT ( 'NONE',  ( -24.31965562422391969, 28.55126061725682973, 37.50000000003461764 ) ) ;
#16633 = ORIENTED_EDGE ( 'NONE', *, *, #12007, .T. ) ;
#16634 = LINE ( 'NONE', #26138, #28296 ) ;
#16635 = EDGE_CURVE ( 'NONE', #13230, #5725, #10801, .T. ) ;
#16636 = B_SPLINE_CURVE_WITH_KNOTS ( 'NONE', 3,
 ( #18027, #11005, #20803, #30329, #18179, #18486, #6623 ),
 .UNSPECIFIED., .F., .F.,
 ( 4, 3, 4 ),
 ( 0.000000000000000000, 0.005028111721571001773, 0.01005622344661834602 ),
 .UNSPECIFIED. ) ;
#16637 = B_SPLINE_CURVE_WITH_KNOTS ( 'NONE', 3,
 ( #1630, #17687, #11141, #29697, #6295, #20339, #27666 ),
 .UNSPECIFIED., .F., .F.,
 ( 4, 3, 4 ),
 ( 0.000000000000000000, 0.005031266823721201875, 0.01006253384080261354 ),
 .UNSPECIFIED. ) ;
#16638 = CARTESIAN_POINT ( 'NONE',  ( 7.341751895053238108, -5.349779314757616255, -1.500000000000002442 ) ) ;
#16639 = CARTESIAN_POINT ( 'NONE',  ( -32.82330813384598400, -22.94799032726886523, -1.500000000000000000 ) ) ;
#16640 = ORIENTED_EDGE ( 'NONE', *, *, #7260, .F. ) ;
#16641 = CARTESIAN_POINT ( 'NONE',  ( -18.41388790264793940, -7.851569931599772012, 6.111214848085761986 ) ) ;
#16642 = DIRECTION ( 'NONE',  ( -0.000000000000000000, -0.000000000000000000, -1.000000000000000000 ) ) ;
#16643 = CARTESIAN_POINT ( 'NONE',  ( -32.81350286003733885, 7.028748154183637631, -6.500000000000000888 ) ) ;
#16644 = CARTESIAN_POINT ( 'NONE',  ( 0.5572578986459522099, -17.03042415120789954, 5.670038381137163519 ) ) ;
#16645 = EDGE_CURVE ( 'NONE', #19224, #17270, #4238, .T. ) ;
#16646 = DIRECTION ( 'NONE',  ( -0.000000000000000000, -0.000000000000000000, 1.000000000000000000 ) ) ;
#16647 = FACE_OUTER_BOUND ( 'NONE', #23830, .T. ) ;
#16648 = CARTESIAN_POINT ( 'NONE',  ( 32.98805937973592961, -22.67054169308934064, 18.00000000000000000 ) ) ;
#16649 = DIRECTION ( 'NONE',  ( -0.000000000000000000, 1.132880637372608986E-16, -1.000000000000000000 ) ) ;
#16650 = EDGE_LOOP ( 'NONE', ( #29810, #25928, #16363, #27660 ) ) ;
#16651 = ADVANCED_FACE ( 'NONE', ( #18284 ), #6432, .F. ) ;
#16652 = EDGE_CURVE ( 'NONE', #15594, #27497, #23154, .T. ) ;
#16653 = CARTESIAN_POINT ( 'NONE',  ( 9.922755320353058295, -13.86203410616581522, 20.34789198813115263 ) ) ;
#16654 = PLANE ( 'NONE',  #8604 ) ;
#16655 = ORIENTED_EDGE ( 'NONE', *, *, #3282, .T. ) ;
#16656 = ADVANCED_FACE ( 'NONE', ( #18896 ), #13749, .F. ) ;
#16657 = ORIENTED_EDGE ( 'NONE', *, *, #18947, .F. ) ;
#16658 = CARTESIAN_POINT ( 'NONE',  ( 4.307942169702174695, 19.53053083060025230, 19.21940439362674624 ) ) ;
#16659 = ORIENTED_EDGE ( 'NONE', *, *, #2117, .T. ) ;
#16660 = DIRECTION ( 'NONE',  ( 0.000000000000000000, -0.000000000000000000, 1.000000000000000000 ) ) ;
#16661 = FACE_BOUND ( 'NONE', #3016, .T. ) ;
#16662 = EDGE_CURVE ( 'NONE', #25790, #8546, #8738, .T. ) ;
#16663 = ORIENTED_EDGE ( 'NONE', *, *, #22907, .T. ) ;
#16664 = CARTESIAN_POINT ( 'NONE',  ( 16.19464367748837219, -5.422319245274325183, 19.36813350477385143 ) ) ;
#16665 = CARTESIAN_POINT ( 'NONE',  ( 16.57618148055192009, 4.095680178559272022, 19.79423548914561692 ) ) ;
#16666 = DIRECTION ( 'NONE',  ( 0.000000000000000000, 0.000000000000000000, 1.000000000000000000 ) ) ;
#16667 = ORIENTED_EDGE ( 'NONE', *, *, #5362, .T. ) ;
#16668 = CARTESIAN_POINT ( 'NONE',  ( 9.249586724479433641, 2.959227181723830036, 1.500000000000001332 ) ) ;
#16669 = AXIS2_PLACEMENT_3D ( 'NONE', #28670, #11987, #7150 ) ;
#16670 = ORIENTED_EDGE ( 'NONE', *, *, #29023, .T. ) ;
#16671 = ORIENTED_EDGE ( 'NONE', *, *, #28234, .F. ) ;
#16672 = ADVANCED_FACE ( 'NONE', ( #28554 ), #11253, .F. ) ;
#16673 = CARTESIAN_POINT ( 'NONE',  ( 7.548823014270646503, -5.738360882149970976, 13.00000000000000178 ) ) ;
#16674 = CARTESIAN_POINT ( 'NONE',  ( -17.76524000349413868, -9.187221810585024073, 5.853797745100182581 ) ) ;
#16675 = EDGE_CURVE ( 'NONE', #24160, #10973, #7870, .T. ) ;
#16676 = CARTESIAN_POINT ( 'NONE',  ( 1.316598178790385321, -17.01073877869967887, 7.500147780736496017 ) ) ;
#16677 = CARTESIAN_POINT ( 'NONE',  ( -15.04923167470879797, -8.024232118851555740, 18.34938820207544907 ) ) ;
#16678 = CARTESIAN_POINT ( 'NONE',  ( 1.588511040599926760, -16.99700008609428181, 19.96568007040468373 ) ) ;
#16679 = FACE_BOUND ( 'NONE', #18629, .T. ) ;
#16680 = VERTEX_POINT ( 'NONE', #30580 ) ;
#16681 = CARTESIAN_POINT ( 'NONE',  ( 10.50588106577561653, -17.03964880432503293, 7.359006845440219102 ) ) ;
#16682 = LINE ( 'NONE', #21337, #23195 ) ;
#16683 = CARTESIAN_POINT ( 'NONE',  ( -13.71804704112738982, 10.14464636835443123, 7.500147780736496017 ) ) ;
#16684 = CARTESIAN_POINT ( 'NONE',  ( -31.56327786402390245, -10.34181101807378944, -16.55003854064094426 ) ) ;
#16685 = ORIENTED_EDGE ( 'NONE', *, *, #22321, .T. ) ;
#16686 = ORIENTED_EDGE ( 'NONE', *, *, #16587, .F. ) ;
#16687 = VECTOR ( 'NONE', #13500, 1000.000000000000000 ) ;
#16688 = FACE_OUTER_BOUND ( 'NONE', #7997, .T. ) ;
#16689 = CARTESIAN_POINT ( 'NONE',  ( 21.65446070919043109, -23.85364010248227018, -16.50001200000000168 ) ) ;
#16690 = PLANE ( 'NONE',  #15332 ) ;
#16691 = CARTESIAN_POINT ( 'NONE',  ( -5.225937649208972857, 16.21530267322276586, 18.39701043959520987 ) ) ;
#16692 = CARTESIAN_POINT ( 'NONE',  ( -15.56680656382032168, -6.886169722869405874, 6.385774490351136201 ) ) ;
#16693 = CARTESIAN_POINT ( 'NONE',  ( 7.500000000000000000, 0.000000000000000000, 0.000000000000000000 ) ) ;
#16694 = CARTESIAN_POINT ( 'NONE',  ( 0.8038475772933646457, 5.196152422706634688, -9.000000000000001776 ) ) ;
#16695 = ORIENTED_EDGE ( 'NONE', *, *, #28061, .T. ) ;
#16696 = CARTESIAN_POINT ( 'NONE',  ( 0.6154569680868984261, -19.99089747819056129, 7.626218077512941562 ) ) ;
#16697 = CARTESIAN_POINT ( 'NONE',  ( -17.58178100985203685, -9.533151461302381335, 19.48477075383300772 ) ) ;
#16698 = DIRECTION ( 'NONE',  ( -1.000000000000000000, 0.000000000000000000, 0.000000000000000000 ) ) ;
#16699 = ORIENTED_EDGE ( 'NONE', *, *, #5162, .F. ) ;
#16700 = CARTESIAN_POINT ( 'NONE',  ( 12.51082390549571421, 11.56795297236522657, 7.632642797338977658 ) ) ;
#16701 = EDGE_LOOP ( 'NONE', ( #16667, #11600, #22511, #22995 ) ) ;
#16702 = CARTESIAN_POINT ( 'NONE',  ( 18.62671295915898639, -7.331958482175751080, 7.366751648393900176 ) ) ;
#16703 = UNCERTAINTY_MEASURE_WITH_UNIT (LENGTH_MEASURE( 1.000000000000000082E-05 ), #9309, 'distance_accuracy_value', 'NONE');
#16704 = CARTESIAN_POINT ( 'NONE',  ( -16.18009747266616571, 40.48382543897108832, -16.50000000000000355 ) ) ;
#16705 = ORIENTED_EDGE ( 'NONE', *, *, #9247, .T. ) ;
#16706 = CARTESIAN_POINT ( 'NONE',  ( 34.93512232095646652, 9.847170278758666129, 27.50000000000000711 ) ) ;
#16707 = CARTESIAN_POINT ( 'NONE',  ( -39.87350638641265732, -4.706224724266461656, -11.49999999999999645 ) ) ;
#16708 = CARTESIAN_POINT ( 'NONE',  ( -8.499586724479453181, -2.959227181723774525, 21.50000000000000000 ) ) ;
#16709 = DIRECTION ( 'NONE',  ( 1.000000000000000000, 0.000000000000000000, 0.000000000000000000 ) ) ;
#16710 = EDGE_CURVE ( 'NONE', #6692, #19471, #2759, .T. ) ;
#16711 = ADVANCED_FACE ( 'NONE', ( #30283 ), #25905, .F. ) ;
#16712 = DIRECTION ( 'NONE',  ( -0.000000000000000000, -0.000000000000000000, -1.000000000000000000 ) ) ;
#16713 = LINE ( 'NONE', #13920, #15334 ) ;
#16714 = ORIENTED_EDGE ( 'NONE', *, *, #25270, .F. ) ;
#16715 = CARTESIAN_POINT ( 'NONE',  ( 69.99999999999998579, -50.00000000000000000, 12.49999999999999112 ) ) ;
#16716 = CARTESIAN_POINT ( 'NONE',  ( 5.105024945674004222, 42.22604126506330857, -1.500000000000000000 ) ) ;
#16717 = CIRCLE ( 'NONE', #3269, 0.7499999999999993339 ) ;
#16718 = CARTESIAN_POINT ( 'NONE',  ( 14.89473990422475680, -17.79239818699420539, 1.500000000000000000 ) ) ;
#16719 = ORIENTED_EDGE ( 'NONE', *, *, #24819, .T. ) ;
#16720 = DIRECTION ( 'NONE',  ( 0.8910248307962433945, -0.4539545692076750738, 0.000000000000000000 ) ) ;
#16721 = DIRECTION ( 'NONE',  ( 0.7071067811865487940, 0.000000000000000000, -0.7071067811865463515 ) ) ;
#16722 = CARTESIAN_POINT ( 'NONE',  ( -17.22181377296915272, -14.41708049311147555, -1.500000000000000000 ) ) ;
#16723 = B_SPLINE_CURVE_WITH_KNOTS ( 'NONE', 3,
 ( #7420, #16468, #9604, #21598, #9455, #8884, #14259, #28631, #25983, #16617, #18971, #2260, #23940, #25417, #2740, #19113, #235, #16928 ),
 .UNSPECIFIED., .F., .F.,
 ( 4, 2, 2, 2, 2, 2, 2, 2, 4 ),
 ( 0.000000000000000000, 0.0003967869494442910830, 0.0007935738988885821660, 0.001190360848332873249, 0.001587147797777164332, 0.001983934747221455415, 0.002380721696665746498, 0.002777508646110037581, 0.003174295595554328664 ),
 .UNSPECIFIED. ) ;
#16724 = CARTESIAN_POINT ( 'NONE',  ( 4.823417668075713927, 16.32807078414248991, 7.267659094423558841 ) ) ;
#16725 = DIRECTION ( 'NONE',  ( 1.000000000000000000, 0.000000000000000000, 0.000000000000000000 ) ) ;
#16726 = ORIENTED_EDGE ( 'NONE', *, *, #15458, .T. ) ;
#16727 = CARTESIAN_POINT ( 'NONE',  ( 38.30271738069522058, 8.424491356373369655, 35.00506926609056535 ) ) ;
#16728 = CARTESIAN_POINT ( 'NONE',  ( -6.458857079295999171, 18.92875833827542209, 5.779535427900762024 ) ) ;
#16729 = ORIENTED_EDGE ( 'NONE', *, *, #29199, .T. ) ;
#16730 = ORIENTED_EDGE ( 'NONE', *, *, #652, .T. ) ;
#16731 = CARTESIAN_POINT ( 'NONE',  ( -3.196529495465446402, -8.413215745754985875, 21.50000000000000000 ) ) ;
#16732 = DIRECTION ( 'NONE',  ( -1.000000000000000000, -0.000000000000000000, -0.000000000000000000 ) ) ;
#16733 = VERTEX_POINT ( 'NONE', #28405 ) ;
#16734 = ORIENTED_EDGE ( 'NONE', *, *, #17743, .F. ) ;
#16735 = DIRECTION ( 'NONE',  ( 1.000000000000000000, 0.000000000000000000, 0.000000000000000000 ) ) ;
#16736 = AXIS2_PLACEMENT_3D ( 'NONE', #30830, #16032, #23186 ) ;
#16737 = ORIENTED_EDGE ( 'NONE', *, *, #575, .T. ) ;
#16738 = ORIENTED_EDGE ( 'NONE', *, *, #6742, .F. ) ;
#16739 = CARTESIAN_POINT ( 'NONE',  ( 0.3493064693810321586, -20.01473674030432193, 20.34789198813115263 ) ) ;
#16740 = DIRECTION ( 'NONE',  ( 1.000000000000000000, 0.000000000000000000, 0.000000000000000000 ) ) ;
#16741 = CYLINDRICAL_SURFACE ( 'NONE', #16845, 0.7500000000000006661 ) ;
#16742 = ORIENTED_EDGE ( 'NONE', *, *, #9043, .T. ) ;
#16743 = LINE ( 'NONE', #23599, #4325 ) ;
#16744 = EDGE_CURVE ( 'NONE', #20718, #6357, #18213, .T. ) ;
#16745 = CARTESIAN_POINT ( 'NONE',  ( 23.16753610420047949, 35.74416778161837982, -13.16661230991478071 ) ) ;
#16746 = CARTESIAN_POINT ( 'NONE',  ( 11.73047935159229027, 12.40726572549739615, 19.79423548914561692 ) ) ;
#16747 = CARTESIAN_POINT ( 'NONE',  ( -2.081668171172168513E-14, 75.00000000000001421, 37.49999999999999289 ) ) ;
#16748 = ORIENTED_EDGE ( 'NONE', *, *, #8241, .F. ) ;
#16749 = CIRCLE ( 'NONE', #28716, 0.7500000000000006661 ) ;
#16750 = AXIS2_PLACEMENT_3D ( 'NONE', #25142, #22345, #24846 ) ;
#16751 = CYLINDRICAL_SURFACE ( 'NONE', #1868, 15.00000000000000000 ) ;
#16752 = CARTESIAN_POINT ( 'NONE',  ( -15.71962203721309592, -1.249857212218242752, -0.6213203435596476032 ) ) ;
#16753 = DIRECTION ( 'NONE',  ( 1.000000000000000000, 0.000000000000000000, 0.000000000000000000 ) ) ;
#16754 = PLANE ( 'NONE',  #14270 ) ;
#16755 = CARTESIAN_POINT ( 'NONE',  ( -23.12946144662536341, 11.96621729904739695, 44.71596222159476497 ) ) ;
#16756 = DIRECTION ( 'NONE',  ( -0.000000000000000000, -0.000000000000000000, 1.000000000000000000 ) ) ;
#16757 = EDGE_CURVE ( 'NONE', #2810, #950, #16538, .T. ) ;
#16758 = CARTESIAN_POINT ( 'NONE',  ( 23.96732207938043402, -33.98584080152387088, -1.500000000000000000 ) ) ;
#16759 = VECTOR ( 'NONE', #23928, 1000.000000000000000 ) ;
#16760 = ORIENTED_EDGE ( 'NONE', *, *, #8243, .F. ) ;
#16761 = ORIENTED_EDGE ( 'NONE', *, *, #30561, .F. ) ;
#16762 = CARTESIAN_POINT ( 'NONE',  ( 0.000000000000000000, 0.000000000000000000, 63.50000000000000000 ) ) ;
#16763 = AXIS2_PLACEMENT_3D ( 'NONE', #20305, #29832, #8303 ) ;
#16764 = CARTESIAN_POINT ( 'NONE',  ( -7.850819104130406068, -15.15878979527105841, 6.037360021877317351 ) ) ;
#16765 = CYLINDRICAL_SURFACE ( 'NONE', #2940, 0.6002263538043648428 ) ;
#16766 = CARTESIAN_POINT ( 'NONE',  ( 5.349779314757592275, 7.341751895053254096, 13.22130136205108819 ) ) ;
#16767 = VERTEX_POINT ( 'NONE', #11565 ) ;
#16768 = ITEM_DEFINED_TRANSFORMATION ( 'NONE', 'NONE', #20352,  #7396 ) ;
#16769 = FACE_OUTER_BOUND ( 'NONE', #16964, .T. ) ;
#16770 = VECTOR ( 'NONE', #3051, 1000.000000000000000 ) ;
#16771 = CARTESIAN_POINT ( 'NONE',  ( 4.659914667891708717, 16.37914622779767981, 7.429667576816606278 ) ) ;
#16772 = VECTOR ( 'NONE', #27240, 1000.000000000000000 ) ;
#16773 = VERTEX_POINT ( 'NONE', #26056 ) ;
#16774 = CARTESIAN_POINT ( 'NONE',  ( 5.828790066614889298, 19.15065750257362609, 20.19668224736330941 ) ) ;
#16775 = CARTESIAN_POINT ( 'NONE',  ( 39.99999999999998579, 80.00000000000001421, 52.49999999999999289 ) ) ;
#16776 = AXIS2_PLACEMENT_3D ( 'NONE', #6948, #10590, #8254 ) ;
#16777 = DIRECTION ( 'NONE',  ( -0.000000000000000000, -0.000000000000000000, -1.000000000000000000 ) ) ;
#16778 = CARTESIAN_POINT ( 'NONE',  ( -35.72251933182172934, 17.10365394847838161, 31.35234673342428380 ) ) ;
#16779 = ORIENTED_EDGE ( 'NONE', *, *, #5011, .F. ) ;
#16780 = DIRECTION ( 'NONE',  ( 0.000000000000000000, 1.000000000000000000, 1.193512090021232842E-16 ) ) ;
#16781 = EDGE_CURVE ( 'NONE', #5107, #8541, #24676, .T. ) ;
#16782 = EDGE_CURVE ( 'NONE', #29877, #14704, #11230, .T. ) ;
#16783 = DIRECTION ( 'NONE',  ( 1.000000000000000000, 0.000000000000000000, 0.000000000000000000 ) ) ;
#16784 = DIRECTION ( 'NONE',  ( -0.000000000000000000, -0.000000000000000000, -1.000000000000000000 ) ) ;
#16785 = VECTOR ( 'NONE', #24033, 1000.000000000000000 ) ;
#16786 = EDGE_CURVE ( 'NONE', #7581, #8115, #26478, .T. ) ;
#16787 = ORIENTED_EDGE ( 'NONE', *, *, #25211, .T. ) ;
#16788 = EDGE_CURVE ( 'NONE', #346, #29075, #29155, .T. ) ;
#16789 = PLANE ( 'NONE',  #11370 ) ;
#16790 = CARTESIAN_POINT ( 'NONE',  ( 64.99999999999998579, 36.86186943028246787, 97.07879600563551037 ) ) ;
#16791 = EDGE_CURVE ( 'NONE', #28030, #22385, #24154, .T. ) ;
#16792 = CARTESIAN_POINT ( 'NONE',  ( -0.1765357775187666733, -17.02148976770177669, 6.310736198168394928 ) ) ;
#16793 = CIRCLE ( 'NONE', #12848, 1.447898107987198646 ) ;
#16794 = CARTESIAN_POINT ( 'NONE',  ( 0.000000000000000000, 42.50000000000000000, 27.50000000000000355 ) ) ;
#16795 = AXIS2_PLACEMENT_3D ( 'NONE', #7402, #2719, #7232 ) ;
#16796 = CARTESIAN_POINT ( 'NONE',  ( -20.71335220384823117, -27.86167394782616213, -16.50001200000000168 ) ) ;
#16797 = CARTESIAN_POINT ( 'NONE',  ( 28.34828976096172681, 29.18752572968383419, -1.500000000000000000 ) ) ;
#16798 = LINE ( 'NONE', #419, #3434 ) ;
#16799 = VERTEX_POINT ( 'NONE', #14970 ) ;
#16800 = EDGE_CURVE ( 'NONE', #386, #5107, #10724, .T. ) ;
#16801 = FACE_OUTER_BOUND ( 'NONE', #5611, .T. ) ;
#16802 = DIRECTION ( 'NONE',  ( -0.000000000000000000, -0.000000000000000000, 1.000000000000000000 ) ) ;
#16803 = EDGE_CURVE ( 'NONE', #14860, #15627, #21838, .T. ) ;
#16804 = ORIENTED_EDGE ( 'NONE', *, *, #14533, .F. ) ;
#16805 = ORIENTED_EDGE ( 'NONE', *, *, #26164, .T. ) ;
#16806 = EDGE_CURVE ( 'NONE', #584, #30261, #5250, .T. ) ;
#16807 = CARTESIAN_POINT ( 'NONE',  ( -49.75043292984307897, 69.99853936330177362, 54.74343500730861223 ) ) ;
#16808 = CIRCLE ( 'NONE', #23759, 5.000000000000004441 ) ;
#16809 = CARTESIAN_POINT ( 'NONE',  ( -9.906018991686922348, 49.01040375155087503, -43.72563556200963575 ) ) ;
#16810 = AXIS2_PLACEMENT_3D ( 'NONE', #8740, #18260, #8906 ) ;
#16811 = ORIENTED_EDGE ( 'NONE', *, *, #11617, .T. ) ;
#16812 = CIRCLE ( 'NONE', #4875, 23.20393738267408779 ) ;
#16813 = DIRECTION ( 'NONE',  ( 1.000000000000000000, 0.000000000000000000, 0.000000000000000000 ) ) ;
#16814 = SURFACE_SIDE_STYLE ('',( #11532 ) ) ;
#16815 = AXIS2_PLACEMENT_3D ( 'NONE', #6405, #15924, #1108 ) ;
#16816 = ORIENTED_EDGE ( 'NONE', *, *, #29186, .F. ) ;
#16817 = CARTESIAN_POINT ( 'NONE',  ( 16.11883921216212201, -5.620554474281627577, 18.73743063545763121 ) ) ;
#16818 = LINE ( 'NONE', #19464, #18258 ) ;
#16819 = VECTOR ( 'NONE', #30248, 1000.000000000000000 ) ;
#16820 = DIRECTION ( 'NONE',  ( 0.000000000000000000, 0.000000000000000000, -1.000000000000000000 ) ) ;
#16821 = ORIENTED_EDGE ( 'NONE', *, *, #13732, .T. ) ;
#16822 = VECTOR ( 'NONE', #27265, 1000.000000000000000 ) ;
#16823 = CARTESIAN_POINT ( 'NONE',  ( -2.523760598493569596, 1.621922452366830747, 24.50000000000000000 ) ) ;
#16824 = ADVANCED_FACE ( 'NONE', ( #5149 ), #12649, .F. ) ;
#16825 = ORIENTED_EDGE ( 'NONE', *, *, #22130, .F. ) ;
#16826 = EDGE_CURVE ( 'NONE', #15068, #9540, #10290, .T. ) ;
#16827 = ADVANCED_FACE ( 'NONE', ( #19186, #2978, #9834 ), #12495, .T. ) ;
#16828 = EDGE_LOOP ( 'NONE', ( #6244, #22320, #22626, #15543 ) ) ;
#16829 = EDGE_CURVE ( 'NONE', #28720, #27915, #5734, .T. ) ;
#16830 = CARTESIAN_POINT ( 'NONE',  ( 23.63178464412187907, 33.91383858794676343, 29.64624590982186447 ) ) ;
#16831 = CARTESIAN_POINT ( 'NONE',  ( -12.77302042131097792, 11.25334833650868838, 19.77662771831109367 ) ) ;
#16832 = CIRCLE ( 'NONE', #4381, 0.7499999999999997780 ) ;
#16833 = VECTOR ( 'NONE', #9235, 1000.000000000000000 ) ;
#16834 = CARTESIAN_POINT ( 'NONE',  ( -8.546421331151638157, -14.74799399427946156, 18.34798005862662507 ) ) ;
#16835 = CARTESIAN_POINT ( 'NONE',  ( 16.16296542101254730, 5.939519782021115191, 24.50000000000000000 ) ) ;
#16836 = DIRECTION ( 'NONE',  ( 0.000000000000000000, 1.132880637372608986E-16, -1.000000000000000000 ) ) ;
#16837 = FACE_BOUND ( 'NONE', #3542, .T. ) ;
#16838 = ORIENTED_EDGE ( 'NONE', *, *, #28461, .F. ) ;
#16839 = EDGE_CURVE ( 'NONE', #14360, #25524, #24483, .T. ) ;
#16840 = CARTESIAN_POINT ( 'NONE',  ( -16.86382086101523470, 2.355052171780695591, 18.63641924841378028 ) ) ;
#16841 = CARTESIAN_POINT ( 'NONE',  ( -8.159193615868369776, 3.993622308618967498, 13.22130136205108819 ) ) ;
#16842 = DIRECTION ( 'NONE',  ( 0.000000000000000000, 0.000000000000000000, 1.000000000000000000 ) ) ;
#16843 = EDGE_LOOP ( 'NONE', ( #10525, #9554 ) ) ;
#16844 = VERTEX_POINT ( 'NONE', #19350 ) ;
#16845 = AXIS2_PLACEMENT_3D ( 'NONE', #26424, #14086, #14414 ) ;
#16846 = DIRECTION ( 'NONE',  ( -0.000000000000000000, -0.000000000000000000, -1.000000000000000000 ) ) ;
#16847 = CARTESIAN_POINT ( 'NONE',  ( -70.00000000000000000, 70.00000000000000000, -92.50000000000000000 ) ) ;
#16848 = CARTESIAN_POINT ( 'NONE',  ( -39.52380524535560369, 7.028748154183623420, -6.500000000000000888 ) ) ;
#16849 = CARTESIAN_POINT ( 'NONE',  ( 18.57699708025014829, -7.409721753143986511, 18.54958172136249672 ) ) ;
#16850 = CARTESIAN_POINT ( 'NONE',  ( -15.22163550579135283, -7.663797071142820272, 7.652108011868851811 ) ) ;
#16851 = CARTESIAN_POINT ( 'NONE',  ( -34.32465979325662886, 12.16814152140377558, 27.50000000000000355 ) ) ;
#16852 = CARTESIAN_POINT ( 'NONE',  ( -5.378544123449405134, 19.26344156360741167, 7.454139397117727661 ) ) ;
#16853 = EDGE_CURVE ( 'NONE', #24237, #23890, #26818, .T. ) ;
#16854 = ORIENTED_EDGE ( 'NONE', *, *, #20077, .T. ) ;
#16855 = AXIS2_PLACEMENT_3D ( 'NONE', #14240, #24070, #12228 ) ;
#16856 = ADVANCED_FACE ( 'NONE', ( #21516 ), #475, .F. ) ;
#16857 = DIRECTION ( 'NONE',  ( 0.000000000000000000, -1.132880637372608986E-16, 1.000000000000000000 ) ) ;
#16858 = CIRCLE ( 'NONE', #22842, 12.18947652193948272 ) ;
#16859 = CARTESIAN_POINT ( 'NONE',  ( -17.92868989761418419, -8.864358285757582223, 20.32200205377525393 ) ) ;
#16860 = DIRECTION ( 'NONE',  ( 0.000000000000000000, 0.000000000000000000, 1.000000000000000000 ) ) ;
#16861 = ORIENTED_EDGE ( 'NONE', *, *, #28246, .T. ) ;
#16862 = CARTESIAN_POINT ( 'NONE',  ( 12.91913032519424398, 11.08701612049550178, 7.176035686813569292 ) ) ;
#16863 = VERTEX_POINT ( 'NONE', #22449 ) ;
#16864 = CARTESIAN_POINT ( 'NONE',  ( 15.89967663190788905, -6.161197767010750503, 7.627891251804737927 ) ) ;
#16865 = CARTESIAN_POINT ( 'NONE',  ( 9.755064781586030520, 13.32952022457704544, 1.500000000000000000 ) ) ;
#16866 = DIRECTION ( 'NONE',  ( 0.000000000000000000, 1.000000000000000000, 0.000000000000000000 ) ) ;
#16867 = EDGE_LOOP ( 'NONE', ( #24005, #9008, #13273, #18808 ) ) ;
#16868 = LINE ( 'NONE', #7515, #20746 ) ;
#16869 = CARTESIAN_POINT ( 'NONE',  ( 10.66613195287592752, -13.33645323721078668, 19.08844262864050023 ) ) ;
#16870 = CARTESIAN_POINT ( 'NONE',  ( -18.09892777451933554, -8.511549950051181312, 5.651480102388684479 ) ) ;
#16871 = SHAPE_REPRESENTATION ( 'Cartridge Outer Retaining Cylinder', ( #7396 ), #14351 ) ;
#16872 = CARTESIAN_POINT ( 'NONE',  ( -26.41394434536854874, -32.09691347257047767, -6.500000000000000888 ) ) ;
#16873 = CARTESIAN_POINT ( 'NONE',  ( 33.51937758206383222, -10.82799271170304323, 39.77598051165973914 ) ) ;
#16874 = ORIENTED_EDGE ( 'NONE', *, *, #14707, .F. ) ;
#16875 = CARTESIAN_POINT ( 'NONE',  ( 26.36764545593179676, 31.31467416275351923, 1.500000000000000000 ) ) ;
#16876 = CIRCLE ( 'NONE', #19303, 32.32717498572574755 ) ;
#16877 = AXIS2_PLACEMENT_3D ( 'NONE', #9317, #18842, #28360 ) ;
#16878 = CARTESIAN_POINT ( 'NONE',  ( -19.64114023396299302, -37.13592150529018454, -1.500000000000000000 ) ) ;
#16879 = CIRCLE ( 'NONE', #10410, 9.084132297865673777 ) ;
#16880 = CARTESIAN_POINT ( 'NONE',  ( -4.163336342344337027E-14, 1.387778780781445676E-14, 24.50000000000000000 ) ) ;
#16881 = ORIENTED_EDGE ( 'NONE', *, *, #26402, .T. ) ;
#16882 = CARTESIAN_POINT ( 'NONE',  ( 0.000000000000000000, 0.000000000000000000, 21.50000000000000000 ) ) ;
#16883 = LINE ( 'NONE', #338, #24745 ) ;
#16884 = CARTESIAN_POINT ( 'NONE',  ( 4.510281037539698445E-13, -4.926614671774132148E-13, 79.49999999999998579 ) ) ;
#16885 = CYLINDRICAL_SURFACE ( 'NONE', #10285, 4.999999999999997335 ) ;
#16886 = CARTESIAN_POINT ( 'NONE',  ( 39.00000000000000000, -5.563236990218592304, -1.500000000000000000 ) ) ;
#16887 = VECTOR ( 'NONE', #9454, 1000.000000000000000 ) ;
#16888 = VERTEX_POINT ( 'NONE', #3270 ) ;
#16889 = CARTESIAN_POINT ( 'NONE',  ( 0.3567147238643519902, -19.99681861211371370, 18.34798005863226678 ) ) ;
#16890 = CARTESIAN_POINT ( 'NONE',  ( 24.38609055551176397, 33.28642614059371141, 34.50551068831410362 ) ) ;
#16891 = EDGE_CURVE ( 'NONE', #25685, #24048, #23336, .T. ) ;
#16892 = CARTESIAN_POINT ( 'NONE',  ( 19.74251403343738076, 3.198927889078825970, 5.652196082369965069 ) ) ;
#16893 = ORIENTED_EDGE ( 'NONE', *, *, #24437, .F. ) ;
#16894 = AXIS2_PLACEMENT_3D ( 'NONE', #23430, #28289, #1632 ) ;
#16895 = DIRECTION ( 'NONE',  ( 1.000000000000000000, 0.000000000000000000, 0.000000000000000000 ) ) ;
#16896 = EDGE_LOOP ( 'NONE', ( #7617, #14094, #30480, #15319 ) ) ;
#16897 = CARTESIAN_POINT ( 'NONE',  ( -3.640207617113898841, 7.856594496258241023, -1.500000000000000888 ) ) ;
#16898 = DIRECTION ( 'NONE',  ( 0.000000000000000000, 0.000000000000000000, 1.000000000000000000 ) ) ;
#16899 = ORIENTED_EDGE ( 'NONE', *, *, #11693, .F. ) ;
#16900 = ORIENTED_EDGE ( 'NONE', *, *, #21022, .F. ) ;
#16901 = CARTESIAN_POINT ( 'NONE',  ( -9.815074746723995602, -17.42621888692031007, 6.037995405461177079 ) ) ;
#16902 = PRODUCT_DEFINITION_SHAPE ( 'NONE', 'NONE',  #30866 ) ;
#16903 = TOROIDAL_SURFACE ( 'NONE', #1468, 37.99999999999933920, 3.000000000000000000 ) ;
#16904 = ORIENTED_EDGE ( 'NONE', *, *, #8197, .T. ) ;
#16905 = ORIENTED_EDGE ( 'NONE', *, *, #11258, .T. ) ;
#16906 = CARTESIAN_POINT ( 'NONE',  ( -0.1834311997418882345, -17.02123387943971977, 19.66989035740801839 ) ) ;
#16907 = CARTESIAN_POINT ( 'NONE',  ( -9.895604986052594754, -17.40083251127919084, 5.951255046771932733 ) ) ;
#16908 = DIRECTION ( 'NONE',  ( 0.000000000000000000, 1.000000000000000000, 1.193512090021232842E-16 ) ) ;
#16909 = CARTESIAN_POINT ( 'NONE',  ( 1.315538599303259781, -19.97434797600633871, 19.03762469184452755 ) ) ;
#16910 = EDGE_LOOP ( 'NONE', ( #7803, #11673 ) ) ;
#16911 = CARTESIAN_POINT ( 'NONE',  ( -8.757878075398936701, -7.394122547431892123, -1.500000000000000000 ) ) ;
#16912 = DIRECTION ( 'NONE',  ( -0.9898214418809327952, -0.1423148382732853101, 0.000000000000000000 ) ) ;
#16913 = CARTESIAN_POINT ( 'NONE',  ( 12.35522127307955209, 11.74279147895035891, 18.34798005862662507 ) ) ;
#16914 = CARTESIAN_POINT ( 'NONE',  ( -4.163336342344337027E-14, 1.387778780781445676E-14, 37.50000000000000000 ) ) ;
#16915 = B_SPLINE_CURVE_WITH_KNOTS ( 'NONE', 3,
 ( #5089, #23950, #23794, #2753 ),
 .UNSPECIFIED., .F., .F.,
 ( 4, 4 ),
 ( 3.018024802580205417E-07, 0.007932103453629119755 ),
 .UNSPECIFIED. ) ;
#16916 = DIRECTION ( 'NONE',  ( -0.000000000000000000, -0.000000000000000000, 1.000000000000000000 ) ) ;
#16917 = CARTESIAN_POINT ( 'NONE',  ( -17.61017686385352121, -9.517781650307568952, 6.892848776733236704 ) ) ;
#16918 = CARTESIAN_POINT ( 'NONE',  ( -6.157909564977939176, 15.91569265719595982, 5.872146474157316831 ) ) ;
#16919 = CARTESIAN_POINT ( 'NONE',  ( -19.94474618696874302, 1.485631111656370518, 6.788986777570692688 ) ) ;
#16920 = LINE ( 'NONE', #28773, #3459 ) ;
#16921 = CARTESIAN_POINT ( 'NONE',  ( -15.45998620766333076, -7.136073936211796642, 18.63641924841378028 ) ) ;
#16922 = CYLINDRICAL_SURFACE ( 'NONE', #1652, 0.7500000000000006661 ) ;
#16923 = ORIENTED_EDGE ( 'NONE', *, *, #15446, .F. ) ;
#16924 = ORIENTED_EDGE ( 'NONE', *, *, #22910, .F. ) ;
#16925 = FACE_OUTER_BOUND ( 'NONE', #1112, .T. ) ;
#16926 = CARTESIAN_POINT ( 'NONE',  ( -5.124412594240626895, 19.33243322302222111, 19.85261563089510872 ) ) ;
#16927 = CARTESIAN_POINT ( 'NONE',  ( -15.28186893989758488, 12.93018916568089338, 7.652108011868850035 ) ) ;
#16928 = CARTESIAN_POINT ( 'NONE',  ( 11.10715495309693424, -16.63223102436629475, 20.34789198813115263 ) ) ;
#16929 = ORIENTED_EDGE ( 'NONE', *, *, #24286, .T. ) ;
#16930 = SHAPE_DEFINITION_REPRESENTATION ( #11925, #12322 ) ;
#16931 = CIRCLE ( 'NONE', #20904, 9.482273699623480212 ) ;
#16932 = CARTESIAN_POINT ( 'NONE',  ( 18.32239734440381440, -8.062462575157598010, 18.34969686940296185 ) ) ;
#16933 = FACE_OUTER_BOUND ( 'NONE', #15569, .T. ) ;
#16934 = ORIENTED_EDGE ( 'NONE', *, *, #3258, .T. ) ;
#16935 = CARTESIAN_POINT ( 'NONE',  ( 4.476939094886639658, 16.43504713094787206, 20.25336174263950184 ) ) ;
#16936 = DIRECTION ( 'NONE',  ( 0.9329908884337539954, -0.3598999890241654231, 0.000000000000000000 ) ) ;
#16937 = VECTOR ( 'NONE', #6339, 1000.000000000000000 ) ;
#16938 = CARTESIAN_POINT ( 'NONE',  ( -7.850819104082916056, -15.15878979529809811, 18.73314399819311760 ) ) ;
#16939 = CARTESIAN_POINT ( 'NONE',  ( -27.47456215299179050, 30.17515099587704341, 34.53186466379878539 ) ) ;
#16940 = EDGE_LOOP ( 'NONE', ( #30206, #8198, #23845, #27297 ) ) ;
#16941 = DIRECTION ( 'NONE',  ( 0.000000000000000000, 0.000000000000000000, -1.000000000000000000 ) ) ;
#16942 = CARTESIAN_POINT ( 'NONE',  ( 33.56327786402390245, 10.22184702512350363, 35.67222522295137566 ) ) ;
#16943 = CARTESIAN_POINT ( 'NONE',  ( 2.075483152176834878, 44.03327996489939977, -16.50000000000000000 ) ) ;
#16944 = ORIENTED_EDGE ( 'NONE', *, *, #4936, .T. ) ;
#16945 = CARTESIAN_POINT ( 'NONE',  ( 37.16608720827707657, 65.00000000000000000, 57.49999999999999289 ) ) ;
#16946 = CARTESIAN_POINT ( 'NONE',  ( 14.87898868866547097, 13.36471831362574747, 5.652196082369964181 ) ) ;
#16947 = LINE ( 'NONE', #23802, #13301 ) ;
#16948 = CIRCLE ( 'NONE', #27917, 1.000000000000011324 ) ;
#16949 = DIRECTION ( 'NONE',  ( -0.000000000000000000, -0.000000000000000000, 1.000000000000000000 ) ) ;
#16950 = CYLINDRICAL_SURFACE ( 'NONE', #6829, 0.7500000000000006661 ) ;
#16951 = CARTESIAN_POINT ( 'NONE',  ( 33.63479021130299174, -21.55299138689128213, 8.000000000000007105 ) ) ;
#16952 = CARTESIAN_POINT ( 'NONE',  ( -77.99999999999998579, -42.49999999999998579, 27.50000000000000000 ) ) ;
#16953 = ORIENTED_EDGE ( 'NONE', *, *, #13604, .F. ) ;
#16954 = CARTESIAN_POINT ( 'NONE',  ( -46.99999999999955236, -4.869056272214205871E-13, 79.49999999999998579 ) ) ;
#16955 = CARTESIAN_POINT ( 'NONE',  ( 2.338573377552017440, 39.50000000000000711, 27.50000000000001776 ) ) ;
#16956 = ORIENTED_EDGE ( 'NONE', *, *, #28037, .F. ) ;
#16957 = EDGE_LOOP ( 'NONE', ( #24087, #30814, #12528, #9796 ) ) ;
#16958 = LINE ( 'NONE', #5425, #28579 ) ;
#16959 = DIRECTION ( 'NONE',  ( 1.000000000000000000, 0.000000000000000000, 0.000000000000000000 ) ) ;
#16960 = ORIENTED_EDGE ( 'NONE', *, *, #21146, .T. ) ;
#16961 = ADVANCED_FACE ( 'NONE', ( #5626 ), #18092, .F. ) ;
#16962 = CARTESIAN_POINT ( 'NONE',  ( 6.899999999999999467, 5.196152422706634688, -9.000000000000001776 ) ) ;
#16963 = DIRECTION ( 'NONE',  ( 1.000000000000000000, 0.000000000000000000, -0.000000000000000000 ) ) ;
#16964 = EDGE_LOOP ( 'NONE', ( #3780, #25379, #19611, #10869 ) ) ;
#16965 = EDGE_CURVE ( 'NONE', #23272, #10393, #15675, .T. ) ;
#16966 = CARTESIAN_POINT ( 'NONE',  ( 15.98815986143406143, -5.948957736846852029, 18.44527579819791185 ) ) ;
#16967 = CARTESIAN_POINT ( 'NONE',  ( 1.073881485057758711, 0.9711784013061475207, 1.500000000000000000 ) ) ;
#16968 = AXIS2_PLACEMENT_3D ( 'NONE', #27918, #16054, #25571 ) ;
#16969 = CARTESIAN_POINT ( 'NONE',  ( 49.99999999999998579, -50.00000000000000000, 62.49999999999999289 ) ) ;
#16970 = ORIENTED_EDGE ( 'NONE', *, *, #26550, .T. ) ;
#16971 = CARTESIAN_POINT ( 'NONE',  ( 24.35970437652574816, -13.37404834226503958, 42.96778633356033339 ) ) ;
#16972 = EDGE_CURVE ( 'NONE', #27445, #25738, #19688, .T. ) ;
#16973 = EDGE_LOOP ( 'NONE', ( #11142, #11022, #664, #28312 ) ) ;
#16974 = EDGE_CURVE ( 'NONE', #5082, #17339, #20119, .T. ) ;
#16975 = CARTESIAN_POINT ( 'NONE',  ( -2.081668171172168513E-14, 80.00000000000000000, 37.49999999999999289 ) ) ;
#16976 = CARTESIAN_POINT ( 'NONE',  ( -12.71685080539083934, 11.31419172277363927, 19.22654678686458141 ) ) ;
#16977 = CARTESIAN_POINT ( 'NONE',  ( -9.661386603328292466, -17.53179420831166269, 19.14333282897057842 ) ) ;
#16978 = CARTESIAN_POINT ( 'NONE',  ( 49.99999999999998579, -70.00000000000000000, -92.50000000000000000 ) ) ;
#16979 = CARTESIAN_POINT ( 'NONE',  ( 0.1262659238204208167, 8.999114229549594057, 21.50000000000000000 ) ) ;
#16980 = DIRECTION ( 'NONE',  ( -0.000000000000000000, -1.000000000000000000, 0.000000000000000000 ) ) ;
#16981 = ORIENTED_EDGE ( 'NONE', *, *, #29590, .F. ) ;
#16982 = CARTESIAN_POINT ( 'NONE',  ( 9.085188746210626221, -14.39608436040016315, 7.080843742048788414 ) ) ;
#16983 = CARTESIAN_POINT ( 'NONE',  ( 21.52288024096207764, -31.67788091438591991, 34.49999999999999289 ) ) ;
#16984 = CIRCLE ( 'NONE', #29451, 2.898871837527151385 ) ;
#16985 = CARTESIAN_POINT ( 'NONE',  ( 4.049916830765387665, 16.55712665160098851, 20.34789198813115263 ) ) ;
#16986 = ORIENTED_EDGE ( 'NONE', *, *, #9470, .F. ) ;
#16987 = ORIENTED_EDGE ( 'NONE', *, *, #27313, .T. ) ;
#16988 = FACE_OUTER_BOUND ( 'NONE', #10804, .T. ) ;
#16989 = ADVANCED_FACE ( 'NONE', ( #15428 ), #8271, .F. ) ;
#16990 = CARTESIAN_POINT ( 'NONE',  ( -32.82330813384395185, 22.94799032727105370, -1.500000000000000000 ) ) ;
#16991 = ADVANCED_FACE ( 'NONE', ( #3435 ), #17601, .T. ) ;
#16992 = CARTESIAN_POINT ( 'NONE',  ( -5.020628478053031252, 16.27454347535058332, 7.500898271101006820 ) ) ;
#16993 = CARTESIAN_POINT ( 'NONE',  ( -15.49717968184286931, -7.050617358874958107, 6.031926333436657295 ) ) ;
#16994 = EDGE_CURVE ( 'NONE', #13279, #30435, #30654, .T. ) ;
#16995 = CARTESIAN_POINT ( 'NONE',  ( 8.539720164285627899E-15, -30.50000000000000711, 24.50000000000000000 ) ) ;
#16996 = ORIENTED_EDGE ( 'NONE', *, *, #6714, .F. ) ;
#16997 = EDGE_CURVE ( 'NONE', #30243, #12174, #23174, .T. ) ;
#16998 = ORIENTED_EDGE ( 'NONE', *, *, #2320, .T. ) ;
#16999 = DIRECTION ( 'NONE',  ( 0.000000000000000000, 0.000000000000000000, 1.000000000000000000 ) ) ;
#17000 = DIRECTION ( 'NONE',  ( 0.000000000000000000, 0.000000000000000000, -1.000000000000000000 ) ) ;
#17001 = CARTESIAN_POINT ( 'NONE',  ( -4.163336342344337027E-14, 1.387778780781445676E-14, 21.50000000000000000 ) ) ;
#17002 = ADVANCED_FACE ( 'NONE', ( #25842 ), #4620, .F. ) ;
#17003 = EDGE_LOOP ( 'NONE', ( #23997, #25387, #607 ) ) ;
#17004 = CARTESIAN_POINT ( 'NONE',  ( 12.43449883826693103, 11.65450130491726632, 7.652108011868850035 ) ) ;
#17005 = ORIENTED_EDGE ( 'NONE', *, *, #25211, .F. ) ;
#17006 = EDGE_CURVE ( 'NONE', #25672, #27411, #14269, .T. ) ;
#17007 = CARTESIAN_POINT ( 'NONE',  ( 18.41033144393026078, -7.859752488074923882, 7.643931100913408550 ) ) ;
#17008 = UNCERTAINTY_MEASURE_WITH_UNIT (LENGTH_MEASURE( 1.000000000000000082E-05 ), #9640, 'distance_accuracy_value', 'NONE');
#17009 = CARTESIAN_POINT ( 'NONE',  ( 16.74250988114177474, 3.198928528055117404, 18.34798005863078885 ) ) ;
#17010 = VECTOR ( 'NONE', #20371, 1000.000000000000000 ) ;
#17011 = LINE ( 'NONE', #29340, #9552 ) ;
#17012 = ORIENTED_EDGE ( 'NONE', *, *, #16652, .T. ) ;
#17013 = EDGE_CURVE ( 'NONE', #160, #16773, #7118, .T. ) ;
#17014 = DIRECTION ( 'NONE',  ( 1.000000000000000000, 0.000000000000000000, 0.000000000000000000 ) ) ;
#17015 = DIRECTION ( 'NONE',  ( -1.000000000000000000, 0.000000000000000000, 0.000000000000000000 ) ) ;
#17016 = DIRECTION ( 'NONE',  ( -0.000000000000000000, -0.000000000000000000, 1.000000000000000000 ) ) ;
#17017 = CARTESIAN_POINT ( 'NONE',  ( 5.412540532954977194E-16, -0.8794428697894915992, -9.000000000000001776 ) ) ;
#17018 = CYLINDRICAL_SURFACE ( 'NONE', #10405, 0.7500000000000024425 ) ;
#17019 = DIRECTION ( 'NONE',  ( 1.000000000000000000, 0.000000000000000000, 0.000000000000000000 ) ) ;
#17020 = CARTESIAN_POINT ( 'NONE',  ( 0.3570196857253488676, 6.047589086024998117, -7.525268439705683043 ) ) ;
#17021 = EDGE_LOOP ( 'NONE', ( #24593, #27463, #1315, #17279 ) ) ;
#17022 = AXIS2_PLACEMENT_3D ( 'NONE', #22021, #17190, #10027 ) ;
#17023 = DIRECTION ( 'NONE',  ( 0.000000000000000000, 0.000000000000000000, -1.000000000000000000 ) ) ;
#17024 = CARTESIAN_POINT ( 'NONE',  ( -25.19442432475474902, -35.44676296258422354, -19.50000000000000355 ) ) ;
#17025 = CARTESIAN_POINT ( 'NONE',  ( 11.21147646446735102, -30.29926891764210595, 1.500000000000000000 ) ) ;
#17026 = EDGE_LOOP ( 'NONE', ( #15314, #10969 ) ) ;
#17027 = DIRECTION ( 'NONE',  ( -0.000000000000000000, 0.000000000000000000, 1.000000000000000000 ) ) ;
#17028 = EDGE_CURVE ( 'NONE', #20269, #2425, #5758, .T. ) ;
#17029 = CARTESIAN_POINT ( 'NONE',  ( -32.51029856060266354, 26.37762524645828321, -16.50000000000000355 ) ) ;
#17030 = ADVANCED_FACE ( 'NONE', ( #4927 ), #2120, .F. ) ;
#17031 = CARTESIAN_POINT ( 'NONE',  ( -14.67633008511251802, 13.58695459845238318, 19.47728749465736797 ) ) ;
#17032 = CARTESIAN_POINT ( 'NONE',  ( 4.819993392629171147, 16.32915940664440058, 6.031926333436655518 ) ) ;
#17033 = CIRCLE ( 'NONE', #23503, 0.7500000000000006661 ) ;
#17034 = CARTESIAN_POINT ( 'NONE',  ( -10.64374042650306862, 42.96126232887723972, -19.50000000000000355 ) ) ;
#17035 = EDGE_CURVE ( 'NONE', #13676, #18657, #21605, .T. ) ;
#17036 = CYLINDRICAL_SURFACE ( 'NONE', #8002, 32.32717498572574755 ) ;
#17037 = CARTESIAN_POINT ( 'NONE',  ( 32.80643058142531743, 23.14278286313888700, 34.65133582147071678 ) ) ;
#17038 = DIRECTION ( 'NONE',  ( -0.000000000000000000, -0.000000000000000000, 1.000000000000000000 ) ) ;
#17039 = ORIENTED_EDGE ( 'NONE', *, *, #5164, .T. ) ;
#17040 = CARTESIAN_POINT ( 'NONE',  ( -1.000000000000008438, 19.97498435543819539, 24.50000000000000000 ) ) ;
#17041 = ORIENTED_EDGE ( 'NONE', *, *, #7124, .T. ) ;
#17042 = CARTESIAN_POINT ( 'NONE',  ( 8.099999999999999645, 0.000000000000000000, 6.000000000000001776 ) ) ;
#17043 = DIRECTION ( 'NONE',  ( 1.000000000000000000, 0.000000000000000000, 0.000000000000000000 ) ) ;
#17044 = VERTEX_POINT ( 'NONE', #7582 ) ;
#17045 = ORIENTED_EDGE ( 'NONE', *, *, #27910, .T. ) ;
#17046 = CARTESIAN_POINT ( 'NONE',  ( -9.748913725731204849, -17.46314199939011402, 6.149077423860693337 ) ) ;
#17047 = VERTEX_POINT ( 'NONE', #2905 ) ;
#17048 = ORIENTED_EDGE ( 'NONE', *, *, #2670, .F. ) ;
#17049 = CARTESIAN_POINT ( 'NONE',  ( 0.7788148826605763020, -17.02744010918315709, 20.34789198813115263 ) ) ;
#17050 = CARTESIAN_POINT ( 'NONE',  ( -23.08950671686661948, 11.27322061222802496, 49.30570747941608545 ) ) ;
#17051 = CARTESIAN_POINT ( 'NONE',  ( 2.168404344971008868E-16, 30.50000000000000000, 1.500000000000000000 ) ) ;
#17052 = CARTESIAN_POINT ( 'NONE',  ( 12.33859880789482233, -8.132258305203423632, -1.500000000000000000 ) ) ;
#17053 = CARTESIAN_POINT ( 'NONE',  ( -20.45518110071315832, 26.46109910111415786, -16.50001199999999812 ) ) ;
#17054 = VERTEX_POINT ( 'NONE', #24410 ) ;
#17055 = DIRECTION ( 'NONE',  ( 1.000000000000000000, 0.000000000000000000, 0.000000000000000000 ) ) ;
#17056 = CARTESIAN_POINT ( 'NONE',  ( 11.83251621799620779, -42.16142857676437217, -16.50000000000000000 ) ) ;
#17057 = CARTESIAN_POINT ( 'NONE',  ( 12.12755608862868328, 11.99246096336392320, 18.39992786714538298 ) ) ;
#17058 = FACE_OUTER_BOUND ( 'NONE', #14692, .T. ) ;
#17059 = ORIENTED_EDGE ( 'NONE', *, *, #30170, .T. ) ;
#17060 = ADVANCED_FACE ( 'NONE', ( #21761 ), #28948, .F. ) ;
#17061 = EDGE_CURVE ( 'NONE', #17300, #15425, #12258, .T. ) ;
#17062 = CIRCLE ( 'NONE', #21032, 0.7499999999999997780 ) ;
#17063 = DIRECTION ( 'NONE',  ( -0.000000000000000000, -0.000000000000000000, 1.000000000000000000 ) ) ;
#17064 = DIRECTION ( 'NONE',  ( -0.000000000000000000, -1.000000000000000000, -0.000000000000000000 ) ) ;
#17065 = CARTESIAN_POINT ( 'NONE',  ( -6.123826420728666342, 19.05819691457235621, 5.661398277488801867 ) ) ;
#17066 = VECTOR ( 'NONE', #18621, 1000.000000000000114 ) ;
#17067 = VECTOR ( 'NONE', #22616, 1000.000000000000000 ) ;
#17068 = CARTESIAN_POINT ( 'NONE',  ( 0.000000000000000000, 0.000000000000000000, 1.500000000000001332 ) ) ;
#17069 = CARTESIAN_POINT ( 'NONE',  ( -70.00000000000000000, -70.00000000000000000, 12.49999999999999112 ) ) ;
#17070 = VECTOR ( 'NONE', #20522, 1000.000000000000000 ) ;
#17071 = CARTESIAN_POINT ( 'NONE',  ( -18.05883950494727230, -8.636531109380523930, 18.34798005862930381 ) ) ;
#17072 = DIRECTION ( 'NONE',  ( -0.000000000000000000, -0.000000000000000000, 1.000000000000000000 ) ) ;
#17073 = ORIENTED_EDGE ( 'NONE', *, *, #5594, .T. ) ;
#17074 = ORIENTED_EDGE ( 'NONE', *, *, #24890, .T. ) ;
#17075 = CARTESIAN_POINT ( 'NONE',  ( 9.131494062835612269, 2.555255504830998170, 1.500000000000001332 ) ) ;
#17076 = CARTESIAN_POINT ( 'NONE',  ( 49.99999999999998579, 50.00000000000000000, 59.49999999999999289 ) ) ;
#17077 = CARTESIAN_POINT ( 'NONE',  ( -12.71124774491287823, 11.32026698792773800, 6.755862304746362845 ) ) ;
#17078 = CARTESIAN_POINT ( 'NONE',  ( -0.1008988851204854764, -17.02363397670944067, 6.143977687428010093 ) ) ;
#17079 = ORIENTED_EDGE ( 'NONE', *, *, #13466, .T. ) ;
#17080 = APPLICATION_PROTOCOL_DEFINITION ( 'draft international standard', 'automotive_design', 1998, #24920 ) ;
#17081 = DIRECTION ( 'NONE',  ( -0.000000000000000000, -0.000000000000000000, -1.000000000000000000 ) ) ;
#17082 = CARTESIAN_POINT ( 'NONE',  ( -22.95669091611927826, -27.54300778121952220, -1.500000000000000000 ) ) ;
#17083 = VERTEX_POINT ( 'NONE', #15045 ) ;
#17084 = CARTESIAN_POINT ( 'NONE',  ( 5.021901920966173272, 16.26348455184632513, 19.33715507985239412 ) ) ;
#17085 = DIRECTION ( 'NONE',  ( -0.000000000000000000, 1.132880637372608986E-16, -1.000000000000000000 ) ) ;
#17086 = CARTESIAN_POINT ( 'NONE',  ( -13.38160118231794371, 10.55829203257429860, 18.34798005863078885 ) ) ;
#17087 = CARTESIAN_POINT ( 'NONE',  ( -38.27812018866794830, -8.165225598437423571, 32.01105402497861263 ) ) ;
#17088 = VERTEX_POINT ( 'NONE', #7739 ) ;
#17089 = CARTESIAN_POINT ( 'NONE',  ( 23.21352257770656990, 10.78826658734920230, 45.15942333309104129 ) ) ;
#17090 = CIRCLE ( 'NONE', #23551, 2.999999999999999112 ) ;
#17091 = VECTOR ( 'NONE', #16308, 1000.000000000000227 ) ;
#17092 = DIRECTION ( 'NONE',  ( 0.000000000000000000, 1.000000000000000000, 0.000000000000000000 ) ) ;
#17093 = CARTESIAN_POINT ( 'NONE',  ( 22.85913406299476591, 36.41590270059426615, -16.50000000000000000 ) ) ;
#17094 = ORIENTED_EDGE ( 'NONE', *, *, #19009, .T. ) ;
#17095 = CARTESIAN_POINT ( 'NONE',  ( -18.43314756787626507, -7.806103702558631063, 6.211014596808754007 ) ) ;
#17096 = CYLINDRICAL_SURFACE ( 'NONE', #423, 23.20393738267338790 ) ;
#17098 = CARTESIAN_POINT ( 'NONE',  ( 1.000000000000000000, 29.50000000000000000, 1.500000000000001332 ) ) ;
#17097 = AXIS2_PLACEMENT_3D ( 'NONE', #7066, #18936, #11597 ) ;
#17099 = CARTESIAN_POINT ( 'NONE',  ( 0.2775250113394570617, -20.01590685155468918, 5.653912893140659257 ) ) ;
#17100 = EDGE_CURVE ( 'NONE', #25215, #29085, #1291, .T. ) ;
#17101 = CARTESIAN_POINT ( 'NONE',  ( -16.96556290498877573, 1.647560670993253540, 5.652196082368482699 ) ) ;
#17102 = CARTESIAN_POINT ( 'NONE',  ( 14.99999999999995737, 1.387778780781445676E-14, 67.49999999999997158 ) ) ;
#17103 = DIRECTION ( 'NONE',  ( -1.000000000000000000, 0.000000000000000000, 0.000000000000000000 ) ) ;
#17104 = DIRECTION ( 'NONE',  ( 0.000000000000000000, -1.000000000000000000, -1.132880637372608986E-16 ) ) ;
#17105 = VERTEX_POINT ( 'NONE', #24256 ) ;
#17106 = CARTESIAN_POINT ( 'NONE',  ( 0.000000000000000000, 0.000000000000000000, -16.50000000000000000 ) ) ;
#17107 = AXIS2_PLACEMENT_3D ( 'NONE', #2570, #6941, #7405 ) ;
#17108 = CARTESIAN_POINT ( 'NONE',  ( 4.333676792162783009, 19.52490442444424801, 6.392525840300347539 ) ) ;
#17109 = ORIENTED_EDGE ( 'NONE', *, *, #63, .F. ) ;
#17110 = EDGE_LOOP ( 'NONE', ( #3684, #19569, #8193, #6775 ) ) ;
#17111 = AXIS2_PLACEMENT_3D ( 'NONE', #16847, #9208, #9825 ) ;
#17112 = DIRECTION ( 'NONE',  ( 0.000000000000000000, 0.5000000000000015543, -0.8660254037844378194 ) ) ;
#17113 = CARTESIAN_POINT ( 'NONE',  ( -13.66229526048730669, 48.09760637535989503, -48.78872922615590824 ) ) ;
#17114 = CIRCLE ( 'NONE', #9145, 7.500000000000008882 ) ;
#17115 = ORIENTED_EDGE ( 'NONE', *, *, #11545, .F. ) ;
#17116 = CARTESIAN_POINT ( 'NONE',  ( 14.89413762494257476, 13.37445394317134273, 18.34798005862930736 ) ) ;
#17117 = CARTESIAN_POINT ( 'NONE',  ( -10.98804681698542751, -16.73276138505788779, 7.500898271101006820 ) ) ;
#17118 = ORIENTED_EDGE ( 'NONE', *, *, #7062, .F. ) ;
#17119 = DIRECTION ( 'NONE',  ( -0.000000000000000000, -0.000000000000000000, 1.000000000000000000 ) ) ;
#17120 = PLANE ( 'NONE',  #12291 ) ;
#17121 = CARTESIAN_POINT ( 'NONE',  ( -6.812559277181930106, 5.881244434206302607, -1.500000000000000888 ) ) ;
#17122 = ORIENTED_EDGE ( 'NONE', *, *, #17188, .T. ) ;
#17123 = CARTESIAN_POINT ( 'NONE',  ( 15.70758541206063796, -6.601999697741291584, 18.37259980046034613 ) ) ;
#17124 = ORIENTED_EDGE ( 'NONE', *, *, #20679, .T. ) ;
#17125 = VERTEX_POINT ( 'NONE', #26767 ) ;
#17126 = CIRCLE ( 'NONE', #6666, 1.447898107987170890 ) ;
#17127 = VECTOR ( 'NONE', #14324, 1000.000000000000114 ) ;
#17128 = CARTESIAN_POINT ( 'NONE',  ( 37.16608720827707657, -36.86186943028246787, 12.49999999999999112 ) ) ;
#17129 = CARTESIAN_POINT ( 'NONE',  ( -6.300265418930215411, 19.00075578015506039, 18.39992786714538298 ) ) ;
#17130 = CARTESIAN_POINT ( 'NONE',  ( -14.72004833196315410, 13.56602982695842208, 19.66989035740801839 ) ) ;
#17131 = CARTESIAN_POINT ( 'NONE',  ( -23.17581250239728519, 34.50630206824671831, -1.499999999999999778 ) ) ;
#17132 = CARTESIAN_POINT ( 'NONE',  ( -38.89958629580320348, 3.114405769308834948, 32.20030128012836457 ) ) ;
#17133 = DIRECTION ( 'NONE',  ( 0.000000000000000000, 0.000000000000000000, 1.000000000000000000 ) ) ;
#17134 = ADVANCED_FACE ( 'NONE', ( #7898 ), #26925, .T. ) ;
#17135 = DIRECTION ( 'NONE',  ( -0.000000000000000000, 1.000000000000000000, 0.000000000000000000 ) ) ;
#17136 = ORIENTED_EDGE ( 'NONE', *, *, #17400, .F. ) ;
#17137 = ADVANCED_FACE ( 'NONE', ( #702 ), #19429, .F. ) ;
#17138 = CARTESIAN_POINT ( 'NONE',  ( -19.87079772360653251, 2.422354609568012851, 5.652605728828373977 ) ) ;
#17139 = CARTESIAN_POINT ( 'NONE',  ( 23.83037915021597186, -29.68074934824784350, 34.49999999999999289 ) ) ;
#17140 = CARTESIAN_POINT ( 'NONE',  ( -17.75446986341067301, 9.207540381081360081, 24.50000000000000000 ) ) ;
#17141 = EDGE_LOOP ( 'NONE', ( #21245, #9413 ) ) ;
#17142 = ORIENTED_EDGE ( 'NONE', *, *, #21576, .F. ) ;
#17143 = CARTESIAN_POINT ( 'NONE',  ( -38.00000000000000711, 80.00000000000000000, 50.49999999999998579 ) ) ;
#17144 = CARTESIAN_POINT ( 'NONE',  ( 10.36464550818151586, -17.10487384371580788, 6.144783687052520094 ) ) ;
#17145 = AXIS2_PLACEMENT_3D ( 'NONE', #23265, #11436, #18003 ) ;
#17146 = PRODUCT_DEFINITION_SHAPE ( 'NONE', 'NONE',  #30862 ) ;
#17147 = FACE_BOUND ( 'NONE', #13969, .T. ) ;
#17148 = DIRECTION ( 'NONE',  ( 0.000000000000000000, 0.000000000000000000, -1.000000000000000000 ) ) ;
#17149 = DIRECTION ( 'NONE',  ( 0.000000000000000000, 0.000000000000000000, -1.000000000000000000 ) ) ;
#17150 = AXIS2_PLACEMENT_3D ( 'NONE', #22135, #12642, #933 ) ;
#17151 = CARTESIAN_POINT ( 'NONE',  ( 39.52380524535562500, 7.028748154183637631, -1.499999999999999556 ) ) ;
#17152 = ORIENTED_EDGE ( 'NONE', *, *, #19872, .T. ) ;
#17153 = CARTESIAN_POINT ( 'NONE',  ( -23.84426482588630947, -29.66596207160800347, 34.49999999999999289 ) ) ;
#17154 = CARTESIAN_POINT ( 'NONE',  ( -35.86437274510341666, 3.536632535693895019, 34.72985588596475992 ) ) ;
#17155 = CARTESIAN_POINT ( 'NONE',  ( 49.99999999999998579, 87.00000000000001421, 52.49999999999999289 ) ) ;
#17156 = EDGE_LOOP ( 'NONE', ( #30054, #9172, #16748, #1996 ) ) ;
#17157 = CARTESIAN_POINT ( 'NONE',  ( 15.52282850165806138, 12.63957212366657501, 6.974106381145714018 ) ) ;
#17158 = ORIENTED_EDGE ( 'NONE', *, *, #23783, .F. ) ;
#17159 = CYLINDRICAL_SURFACE ( 'NONE', #9951, 20.00000000000000000 ) ;
#17160 = CARTESIAN_POINT ( 'NONE',  ( 37.99999999999999289, 209.2686044187655909, -34.50000000000000000 ) ) ;
#17161 = DIRECTION ( 'NONE',  ( 0.6548607339452890974, 0.7557495743542548272, 0.000000000000000000 ) ) ;
#17162 = ORIENTED_EDGE ( 'NONE', *, *, #3316, .T. ) ;
#17163 = EDGE_CURVE ( 'NONE', #7591, #8705, #3281, .T. ) ;
#17164 = DIRECTION ( 'NONE',  ( -0.000000000000000000, -0.000000000000000000, -1.000000000000000000 ) ) ;
#17165 = EDGE_CURVE ( 'NONE', #13536, #12805, #3785, .T. ) ;
#17166 = LINE ( 'NONE', #24174, #631 ) ;
#17167 = CYLINDRICAL_SURFACE ( 'NONE', #7848, 6.000000000000005329 ) ;
#17168 = CARTESIAN_POINT ( 'NONE',  ( -2.931009552726339784, -14.22630671667915969, 1.500000000000000000 ) ) ;
#17169 = AXIS2_PLACEMENT_3D ( 'NONE', #17904, #25210, #13072 ) ;
#17170 = FACE_OUTER_BOUND ( 'NONE', #10456, .T. ) ;
#17171 = CARTESIAN_POINT ( 'NONE',  ( 10.50588106577561653, -17.03964880432502937, 20.05479082170252525 ) ) ;
#17172 = EDGE_CURVE ( 'NONE', #26111, #22154, #17708, .T. ) ;
#17173 = CARTESIAN_POINT ( 'NONE',  ( 0.5590800469813631546, 5.620102221249823060, -8.265697409064610923 ) ) ;
#17174 = ORIENTED_EDGE ( 'NONE', *, *, #6716, .T. ) ;
#17175 = EDGE_CURVE ( 'NONE', #15632, #21841, #28738, .T. ) ;
#17176 = CARTESIAN_POINT ( 'NONE',  ( -5.130938270761554065, 7.974144905643839820, 21.50000000000000000 ) ) ;
#17177 = CARTESIAN_POINT ( 'NONE',  ( 19.64114023396309960, -37.13592150529014191, -1.500000000000000000 ) ) ;
#17178 = CARTESIAN_POINT ( 'NONE',  ( -8.884323311075783991, -1.438332125858144295, 21.50000000000000000 ) ) ;
#17179 = EDGE_LOOP ( 'NONE', ( #8052, #7547, #4524, #23211 ) ) ;
#17180 = CARTESIAN_POINT ( 'NONE',  ( 29.18339868661345804, -28.19386397657844867, 9.751140820222291339 ) ) ;
#17182 = EDGE_CURVE ( 'NONE', #11519, #5775, #6908, .T. ) ;
#17181 = CARTESIAN_POINT ( 'NONE',  ( -46.83962922035959053, 69.75107690209843270, 59.80789677786150094 ) ) ;
#17183 = PLANE ( 'NONE',  #17319 ) ;
#17184 = CARTESIAN_POINT ( 'NONE',  ( 4.045242219987652987, 16.55840560649981441, 5.652196082368482699 ) ) ;
#17185 = CARTESIAN_POINT ( 'NONE',  ( 4.336808689942017736E-16, 42.50000000000000000, -1.500000000000000000 ) ) ;
#17186 = EDGE_CURVE ( 'NONE', #19170, #27254, #23729, .T. ) ;
#17187 = CARTESIAN_POINT ( 'NONE',  ( 8.197313248159948884, -3.914781618004724795, 13.22130136205108819 ) ) ;
#17188 = EDGE_CURVE ( 'NONE', #20591, #29733, #6754, .T. ) ;
#17189 = CARTESIAN_POINT ( 'NONE',  ( 26.73499487113253892, 26.30340432104372894, 37.50000000004516210 ) ) ;
#17190 = DIRECTION ( 'NONE',  ( -0.000000000000000000, -0.000000000000000000, 1.000000000000000000 ) ) ;
#17191 = ORIENTED_EDGE ( 'NONE', *, *, #4245, .T. ) ;
#17192 = ORIENTED_EDGE ( 'NONE', *, *, #20131, .T. ) ;
#17193 = DIRECTION ( 'NONE',  ( -0.000000000000000000, 1.000000000000000000, -0.000000000000000000 ) ) ;
#17194 = DIRECTION ( 'NONE',  ( 0.000000000000000000, 0.000000000000000000, 1.000000000000000000 ) ) ;
#17195 = ORIENTED_EDGE ( 'NONE', *, *, #18153, .T. ) ;
#17196 = AXIS2_PLACEMENT_3D ( 'NONE', #2657, #21674, #21989 ) ;
#17197 = VERTEX_POINT ( 'NONE', #181 ) ;
#17198 = DIRECTION ( 'NONE',  ( 0.000000000000000000, 1.000000000000000000, 0.000000000000000000 ) ) ;
#17199 = ORIENTED_EDGE ( 'NONE', *, *, #20814, .F. ) ;
#17200 = ORIENTED_EDGE ( 'NONE', *, *, #9944, .F. ) ;
#17201 = CARTESIAN_POINT ( 'NONE',  ( -32.28307784207223108, -8.475829241206275455, 41.62281023987519291 ) ) ;
#17202 = EDGE_CURVE ( 'NONE', #28757, #29885, #23894, .T. ) ;
#17203 = CARTESIAN_POINT ( 'NONE',  ( -27.20149534458562712, 25.89115957524252210, 34.49999999999998579 ) ) ;
#17204 = EDGE_CURVE ( 'NONE', #13692, #1863, #25353, .T. ) ;
#17205 = DIRECTION ( 'NONE',  ( 0.000000000000000000, 0.000000000000000000, -1.000000000000000000 ) ) ;
#17206 = DIRECTION ( 'NONE',  ( 0.000000000000000000, 0.000000000000000000, 1.000000000000000000 ) ) ;
#17207 = CARTESIAN_POINT ( 'NONE',  ( -11.82521593960875528, 5.400395169024524655, 24.50000000000000000 ) ) ;
#17208 = AXIS2_PLACEMENT_3D ( 'NONE', #25853, #8864, #13698 ) ;
#17209 = EDGE_LOOP ( 'NONE', ( #30392, #23592, #2625, #1480 ) ) ;
#17210 = ADVANCED_FACE ( 'NONE', ( #23575 ), #26553, .F. ) ;
#17211 = CARTESIAN_POINT ( 'NONE',  ( 9.041888939645136958, -0.8750451464062836138, -1.500000000000001776 ) ) ;
#17212 = DIRECTION ( 'NONE',  ( 0.000000000000000000, -1.000000000000000000, 0.000000000000000000 ) ) ;
#17213 = CARTESIAN_POINT ( 'NONE',  ( 0.8978415369256436129, -19.99755156235222486, 5.810767894563978686 ) ) ;
#17214 = FACE_OUTER_BOUND ( 'NONE', #3198, .T. ) ;
#17215 = EDGE_LOOP ( 'NONE', ( #4612, #24754, #6191, #29495, #569, #3399, #2767, #29690, #15007, #26945 ) ) ;
#17216 = EDGE_CURVE ( 'NONE', #19423, #29398, #21230, .T. ) ;
#17217 = CARTESIAN_POINT ( 'NONE',  ( -37.99999999999999289, 70.00000000000000000, -22.50000000000001421 ) ) ;
#17218 = CARTESIAN_POINT ( 'NONE',  ( -14.74412167020460984, -8.612351851578502249, 6.233981582756856987 ) ) ;
#17219 = PLANE ( 'NONE',  #1399 ) ;
#17220 = VECTOR ( 'NONE', #17085, 1000.000000000000000 ) ;
#17221 = CARTESIAN_POINT ( 'NONE',  ( -19.92877566111875254, 1.688993080932622348, 6.037995405461178855 ) ) ;
#17222 = EDGE_CURVE ( 'NONE', #13104, #30552, #21698, .T. ) ;
#17223 = CARTESIAN_POINT ( 'NONE',  ( -15.30652580117162209, -7.480423316612002438, 18.39701043959520987 ) ) ;
#17224 = AXIS2_PLACEMENT_3D ( 'NONE', #28202, #14014, #18857 ) ;
#17225 = DIRECTION ( 'NONE',  ( -0.000000000000000000, -0.000000000000000000, 1.000000000000000000 ) ) ;
#17226 = VERTEX_POINT ( 'NONE', #9550 ) ;
#17227 = ORIENTED_EDGE ( 'NONE', *, *, #24059, .F. ) ;
#17228 = PLANE ( 'NONE',  #8481 ) ;
#17229 = CARTESIAN_POINT ( 'NONE',  ( -5.378544123449399805, 19.26344156360739746, 20.14992337338002315 ) ) ;
#17230 = CYLINDRICAL_SURFACE ( 'NONE', #18421, 0.7500000000000006661 ) ;
#17231 = DIRECTION ( 'NONE',  ( -0.000000000000000000, -0.000000000000000000, -1.000000000000000000 ) ) ;
#17232 = VERTEX_POINT ( 'NONE', #19377 ) ;
#17233 = SHAPE_DEFINITION_REPRESENTATION ( #24374, #20057 ) ;
#17234 = CARTESIAN_POINT ( 'NONE',  ( 15.76815964721466479, -6.465453726329343453, 18.35377592296120497 ) ) ;
#17235 = CIRCLE ( 'NONE', #1301, 10.00000000000000178 ) ;
#17236 = LINE ( 'NONE', #5392, #26143 ) ;
#17237 = ADVANCED_FACE ( 'NONE', ( #339 ), #12051, .F. ) ;
#17238 = ORIENTED_EDGE ( 'NONE', *, *, #23124, .T. ) ;
#17239 = LINE ( 'NONE', #10681, #8327 ) ;
#17240 = CARTESIAN_POINT ( 'NONE',  ( -9.062880100047301823, -0.6210184355499139830, 13.22130136205108819 ) ) ;
#17241 = EDGE_CURVE ( 'NONE', #20990, #10442, #13254, .T. ) ;
#17242 = CARTESIAN_POINT ( 'NONE',  ( -7.786278744154469855, -15.19480685132476161, 19.85459532544248162 ) ) ;
#17243 = CARTESIAN_POINT ( 'NONE',  ( -37.89343041208743301, -10.07310561413692440, 31.90045860481988882 ) ) ;
#17244 = ORIENTED_EDGE ( 'NONE', *, *, #22, .F. ) ;
#17245 = B_SPLINE_CURVE_WITH_KNOTS ( 'NONE', 3,
 ( #2223, #9414, #9099, #8959, #18930, #8790, #20640, #18318, #28436, #27834, #26086, #6463, #4115, #4257, #18618, #6753, #28586, #16889 ),
 .UNSPECIFIED., .F., .F.,
 ( 4, 2, 2, 2, 2, 2, 2, 2, 4 ),
 ( 0.003174295595554302643, 0.003570702171545536274, 0.003967108747536769904, 0.004363515323528003101, 0.004759921899519237165, 0.005156328475510471229, 0.005552735051501704426, 0.005949141627492937623, 0.006345548203484171687 ),
 .UNSPECIFIED. ) ;
#17246 = CARTESIAN_POINT ( 'NONE',  ( 0.000000000000000000, 0.000000000000000000, 1.500000000000000000 ) ) ;
#17247 = VECTOR ( 'NONE', #2834, 1000.000000000000000 ) ;
#17248 = AXIS2_PLACEMENT_3D ( 'NONE', #17251, #24569, #22233 ) ;
#17249 = AXIS2_PLACEMENT_3D ( 'NONE', #2079, #18941, #2234 ) ;
#17250 = CARTESIAN_POINT ( 'NONE',  ( 7.241839955191071709, 43.38385797512582087, -16.49999999999999645 ) ) ;
#17251 = CARTESIAN_POINT ( 'NONE',  ( 0.4269445148198864892, 2.969464325642835689, 24.50000000000000000 ) ) ;
#17252 = ORIENTED_EDGE ( 'NONE', *, *, #28622, .T. ) ;
#17253 = CARTESIAN_POINT ( 'NONE',  ( -15.19605639364643324, -7.717080560943921697, 5.653912893140659257 ) ) ;
#17254 = CARTESIAN_POINT ( 'NONE',  ( 14.18307372309186576, 14.10107868313151691, 6.523620417364438318 ) ) ;
#17255 = CARTESIAN_POINT ( 'NONE',  ( -0.1272161363927056532, -17.02285684280287725, 6.211014596808754007 ) ) ;
#17256 = DIRECTION ( 'NONE',  ( 1.000000000000000000, 0.000000000000000000, 0.000000000000000000 ) ) ;
#17257 = DIRECTION ( 'NONE',  ( 0.9898214418809327952, 0.1423148382732852546, 0.000000000000000000 ) ) ;
#17258 = CYLINDRICAL_SURFACE ( 'NONE', #19981, 20.00000000000000000 ) ;
#17259 = CIRCLE ( 'NONE', #3819, 0.7500000000000006661 ) ;
#17260 = CARTESIAN_POINT ( 'NONE',  ( 0.000000000000000000, 0.000000000000000000, -52.50000000000000000 ) ) ;
#17261 = VERTEX_POINT ( 'NONE', #4714 ) ;
#17262 = DIRECTION ( 'NONE',  ( 0.000000000000000000, 0.000000000000000000, 1.000000000000000000 ) ) ;
#17263 = DIRECTION ( 'NONE',  ( -0.000000000000000000, -0.000000000000000000, -1.000000000000000000 ) ) ;
#17264 = ORIENTED_EDGE ( 'NONE', *, *, #5011, .T. ) ;
#17265 = VERTEX_POINT ( 'NONE', #14685 ) ;
#17266 = AXIS2_PLACEMENT_3D ( 'NONE', #28112, #16104, #23257 ) ;
#17267 = DIRECTION ( 'NONE',  ( -0.000000000000000000, -0.000000000000000000, -1.000000000000000000 ) ) ;
#17268 = DIRECTION ( 'NONE',  ( -0.000000000000000000, -0.000000000000000000, 1.000000000000000000 ) ) ;
#17269 = AXIS2_PLACEMENT_3D ( 'NONE', #3688, #712, #13052 ) ;
#17270 = VERTEX_POINT ( 'NONE', #4871 ) ;
#17271 = AXIS2_PLACEMENT_3D ( 'NONE', #797, #8299, #17340 ) ;
#17272 = CARTESIAN_POINT ( 'NONE',  ( 15.11794152162359595, 13.12142272612526206, 18.39701043959520987 ) ) ;
#17273 = CARTESIAN_POINT ( 'NONE',  ( -8.832446728800205094, -14.56826516372322544, 5.701226463332907279 ) ) ;
#17274 = VERTEX_POINT ( 'NONE', #9244 ) ;
#17275 = CARTESIAN_POINT ( 'NONE',  ( -19.72513283648485327, 3.411576116177899465, 7.080843742048788414 ) ) ;
#17276 = CARTESIAN_POINT ( 'NONE',  ( 64.99999999999998579, -70.00000000000000000, 12.49999999999999112 ) ) ;
#17277 = AXIS2_PLACEMENT_3D ( 'NONE', #18467, #13925, #23271 ) ;
#17278 = DIRECTION ( 'NONE',  ( -0.000000000000000000, -0.000000000000000000, -1.000000000000000000 ) ) ;
#17279 = ORIENTED_EDGE ( 'NONE', *, *, #27114, .F. ) ;
#17280 = EDGE_CURVE ( 'NONE', #27809, #17660, #25186, .T. ) ;
#17281 = CARTESIAN_POINT ( 'NONE',  ( 15.38599937579231636, -7.279790735017073189, 19.41069149716887310 ) ) ;
#17282 = ORIENTED_EDGE ( 'NONE', *, *, #22693, .T. ) ;
#17283 = CARTESIAN_POINT ( 'NONE',  ( 12.09996233686562128, 37.29787398801550324, 27.50000000000001066 ) ) ;
#17284 = ORIENTED_EDGE ( 'NONE', *, *, #24101, .T. ) ;
#17285 = AXIS2_PLACEMENT_3D ( 'NONE', #27854, #29891, #30336 ) ;
#17286 = CARTESIAN_POINT ( 'NONE',  ( 38.79281043785276495, -5.073460407337612388, 32.16650784045132383 ) ) ;
#17287 = CARTESIAN_POINT ( 'NONE',  ( -6.307863225249116468, 15.86248630188382513, 18.73743063545763121 ) ) ;
#17288 = CARTESIAN_POINT ( 'NONE',  ( -15.35487586320816078, 12.84287697592353084, 20.34789198813115263 ) ) ;
#17289 = VECTOR ( 'NONE', #29156, 1000.000000000000114 ) ;
#17290 = CARTESIAN_POINT ( 'NONE',  ( -10.52279982399694092, -17.02885636288122839, 18.34798005862662507 ) ) ;
#17291 = CARTESIAN_POINT ( 'NONE',  ( -37.56589145670645280, -11.49135466129804684, 31.80857576914547380 ) ) ;
#17292 = CARTESIAN_POINT ( 'NONE',  ( 8.413215745754998309, -3.196529495465417980, -1.500000000000002220 ) ) ;
#17293 = CARTESIAN_POINT ( 'NONE',  ( -6.630478080506957639, -6.778663211761441154, 21.50000000000000000 ) ) ;
#17294 = ORIENTED_EDGE ( 'NONE', *, *, #13785, .F. ) ;
#17295 = CARTESIAN_POINT ( 'NONE',  ( 10.30772981839320934, -17.16011447240169474, 6.310736198168394928 ) ) ;
#17296 = B_SPLINE_CURVE_WITH_KNOTS ( 'NONE', 3,
 ( #1373, #1066, #8088, #27263, #3238, #10888, #10575, #6046, #20398, #22263, #1223, #18059, #29755, #22106, #5895, #12761, #10723, #8234, #27576, #17739 ),
 .UNSPECIFIED., .F., .F.,
 ( 4, 2, 2, 2, 2, 2, 2, 2, 2, 4 ),
 ( 0.000000000000000000, 0.06250000000000179023, 0.1250000000000035805, 0.1875000000000053846, 0.2187500000000055234, 0.2500000000000056621, 0.3125000000000042744, 0.3750000000000029421, 0.4375000000000015543, 0.5000000000000001110 ),
 .UNSPECIFIED. ) ;
#17297 = CIRCLE ( 'NONE', #1871, 37.60050224823048381 ) ;
#17298 = DIRECTION ( 'NONE',  ( 0.000000000000000000, 0.000000000000000000, -1.000000000000000000 ) ) ;
#17299 = CARTESIAN_POINT ( 'NONE',  ( 10.47960520055065992, -7.757439966934453146, 24.50000000000000000 ) ) ;
#17300 = VERTEX_POINT ( 'NONE', #24188 ) ;
#17301 = ORIENTED_EDGE ( 'NONE', *, *, #19964, .T. ) ;
#17302 = CARTESIAN_POINT ( 'NONE',  ( 32.60829997825918980, 13.18983524832148646, 35.60092001944725126 ) ) ;
#17303 = CARTESIAN_POINT ( 'NONE',  ( 10.42711161940499309, -17.06705191410859612, 7.267242832833948007 ) ) ;
#17304 = CIRCLE ( 'NONE', #21775, 10.00000000000000178 ) ;
#17305 = DIRECTION ( 'NONE',  ( -0.000000000000000000, -0.000000000000000000, 1.000000000000000000 ) ) ;
#17306 = CARTESIAN_POINT ( 'NONE',  ( -25.64627119138473432, 23.40052582045089480, -6.500000000000000888 ) ) ;
#17307 = CIRCLE ( 'NONE', #29761, 9.084132297865673777 ) ;
#17308 = CYLINDRICAL_SURFACE ( 'NONE', #19139, 20.00000000000000000 ) ;
#17309 = CIRCLE ( 'NONE', #16312, 28.20443790117971261 ) ;
#17310 = LINE ( 'NONE', #19965, #17406 ) ;
#17311 = ORIENTED_EDGE ( 'NONE', *, *, #10589, .T. ) ;
#17312 = VECTOR ( 'NONE', #29383, 1000.000000000000000 ) ;
#17313 = CARTESIAN_POINT ( 'NONE',  ( 0.4831130459764271801, -19.99459506363783490, 7.652108011868850923 ) ) ;
#17314 = CARTESIAN_POINT ( 'NONE',  ( -17.76524000349413157, -9.187221810585024073, 18.54958172136248251 ) ) ;
#17315 = CARTESIAN_POINT ( 'NONE',  ( 16.75466217413942971, 3.123260753354264452, 5.653912893140659257 ) ) ;
#17316 = ORIENTED_EDGE ( 'NONE', *, *, #24437, .T. ) ;
#17317 = CARTESIAN_POINT ( 'NONE',  ( 12.87427757126086547, 11.14157019477621269, 6.018569869498933578 ) ) ;
#17318 = ORIENTED_EDGE ( 'NONE', *, *, #15278, .F. ) ;
#17319 = AXIS2_PLACEMENT_3D ( 'NONE', #7833, #26704, #29194 ) ;
#17320 = CARTESIAN_POINT ( 'NONE',  ( 20.71335220384823117, -27.86167394782616213, -16.50000600000000262 ) ) ;
#17321 = AXIS2_PLACEMENT_3D ( 'NONE', #23490, #1679, #23637 ) ;
#17322 = PLANE ( 'NONE',  #17858 ) ;
#17323 = DIRECTION ( 'NONE',  ( -0.000000000000000000, -0.000000000000000000, 1.000000000000000000 ) ) ;
#17324 = AXIS2_PLACEMENT_3D ( 'NONE', #19917, #17422, #17257 ) ;
#17325 = ORIENTED_EDGE ( 'NONE', *, *, #15877, .T. ) ;
#17326 = CARTESIAN_POINT ( 'NONE',  ( 49.93671616582084738, 70.00028419060272711, 53.79459073512090583 ) ) ;
#17327 = CARTESIAN_POINT ( 'NONE',  ( -7.869584159753960861, 10.39565510934976977, 1.500000000000001332 ) ) ;
#17328 = LINE ( 'NONE', #9849, #3370 ) ;
#17329 = CARTESIAN_POINT ( 'NONE',  ( 32.99222498713436380, 15.81026154464086986, 34.49999999999998579 ) ) ;
#17330 = VECTOR ( 'NONE', #21300, 1000.000000000000000 ) ;
#17331 = AXIS2_PLACEMENT_3D ( 'NONE', #13510, #13662, #1792 ) ;
#17332 = CARTESIAN_POINT ( 'NONE',  ( -16.65122935894506639, -13.93942108199812324, 1.500000000000000000 ) ) ;
#17333 = CARTESIAN_POINT ( 'NONE',  ( 9.579384792474774812, -14.08793303971872390, 20.29090034784956131 ) ) ;
#17334 = CYLINDRICAL_SURFACE ( 'NONE', #19841, 0.7500000000000006661 ) ;
#17335 = VERTEX_POINT ( 'NONE', #12199 ) ;
#17336 = CARTESIAN_POINT ( 'NONE',  ( -34.99999999999933920, 0.000000000000000000, 85.49999999999998579 ) ) ;
#17337 = CARTESIAN_POINT ( 'NONE',  ( -15.63429437150529822, 12.50148542865849244, 20.25542030744407640 ) ) ;
#17338 = DIRECTION ( 'NONE',  ( 1.000000000000000000, 0.000000000000000000, 0.000000000000000000 ) ) ;
#17339 = VERTEX_POINT ( 'NONE', #18924 ) ;
#17340 = DIRECTION ( 'NONE',  ( 1.000000000000000000, 0.000000000000000000, 0.000000000000000000 ) ) ;
#17341 = CIRCLE ( 'NONE', #29804, 15.00000000000000000 ) ;
#17342 = LINE ( 'NONE', #26871, #21682 ) ;
#17343 = B_SPLINE_SURFACE_WITH_KNOTS ( 'NONE', 1, 3, ( 
 ( #30021, #25172, #1170, #27532, #6305, #15819, #20036, #10843, #15350, #20350, #29879, #27215, #27384, #15978, #22522, #29708, #17697, #5851, #18169, #25337, #3979, #6005, #1639, #8801, #22983, #6153, #20646, #27840, #3519, #11150, #18327, #10677, #6468, #23135, #20183, #25499, #4124, #13651, #10999, #8520, #1781, #8192 ),
 ( #15508, #17867, #22671, #8352, #3666, #25024, #13180, #3817, #15659, #13340, #22837, #1488, #20498, #18481, #20940, #9562, #14078, #26244, #13792, #23741, #18626, #11920, #2393, #9258, #6760, #4575, #1932, #11457, #2075, #21411, #25647, #11749, #4884, #21243, #16578, #30319, #23586, #30464, #18937, #16278, #28137, #9108 ) ),
 .UNSPECIFIED., .F., .T., .F.,
 ( 2, 2 ),
 ( 4, 2, 2, 2, 2, 2, 2, 2, 2, 2, 2, 2, 2, 2, 2, 2, 2, 2, 2, 2, 4 ),
 ( 0.000000000000000000, 1.000000000000000000 ),
 ( 0.000000000000000000, 0.1963495408493620697, 0.3926990816987241395, 0.7853981633974482790, 1.178097245096172418, 1.570796326794896558, 1.963495408493620697, 2.356194490192344837, 2.748893571891068976, 2.945243112740430824, 3.141592653589793116, 3.337942194439155408, 3.534291735288517255, 3.926990816987241395, 4.319689898685965090, 4.712388980384689674, 5.105088062083414258, 5.497787143782137953, 5.890486225480861648, 6.086835766330223940, 6.283185307179586232 ),
 .UNSPECIFIED. ) ;
#17344 = LINE ( 'NONE', #10166, #19810 ) ;
#17345 = LINE ( 'NONE', #22790, #21720 ) ;
#17346 = AXIS2_PLACEMENT_3D ( 'NONE', #522, #4901, #21579 ) ;
#17347 = CARTESIAN_POINT ( 'NONE',  ( -5.374868878254082105, 44.10336124695542992, -19.50000000000000355 ) ) ;
#17348 = DIRECTION ( 'NONE',  ( -0.000000000000000000, -0.000000000000000000, -1.000000000000000000 ) ) ;
#17349 = CARTESIAN_POINT ( 'NONE',  ( 16.86471733739763934, 2.322843836264933515, 6.143977687428010093 ) ) ;
#17350 = PRODUCT_RELATED_PRODUCT_CATEGORY ( 'part', '', ( #4943 ) ) ;
#17351 = DIRECTION ( 'NONE',  ( 1.000000000000000000, 1.776356839400250465E-15, 0.000000000000000000 ) ) ;
#17352 = ORIENTED_EDGE ( 'NONE', *, *, #21768, .T. ) ;
#17353 = CARTESIAN_POINT ( 'NONE',  ( 33.46566279634534169, -23.92259740141108537, -11.49999999999999822 ) ) ;
#17354 = AXIS2_PLACEMENT_3D ( 'NONE', #10039, #10499, #3173 ) ;
#17355 = CARTESIAN_POINT ( 'NONE',  ( -23.36057818983818279, -12.54850586925978284, 44.23991181465311229 ) ) ;
#17356 = DIRECTION ( 'NONE',  ( -0.000000000000000000, 0.000000000000000000, 1.000000000000000000 ) ) ;
#17357 = APPLICATION_CONTEXT ( 'automotive_design' ) ;
#17358 = ORIENTED_EDGE ( 'NONE', *, *, #22155, .F. ) ;
#17359 = ORIENTED_EDGE ( 'NONE', *, *, #21962, .T. ) ;
#17360 = CARTESIAN_POINT ( 'NONE',  ( -4.163336342344337027E-14, 1.387778780781445676E-14, 24.50000000000000000 ) ) ;
#17361 = EDGE_CURVE ( 'NONE', #16046, #4862, #21546, .T. ) ;
#17362 = VERTEX_POINT ( 'NONE', #18764 ) ;
#17363 = ORIENTED_EDGE ( 'NONE', *, *, #4081, .F. ) ;
#17364 = CARTESIAN_POINT ( 'NONE',  ( 2.270234684139677217, -8.795879380940574421, 13.22130136205108641 ) ) ;
#17365 = PRODUCT_DEFINITION_FORMATION_WITH_SPECIFIED_SOURCE ( 'ANY', '', #4430, .NOT_KNOWN. ) ;
#17366 = DIRECTION ( 'NONE',  ( -0.000000000000000000, -0.000000000000000000, 1.000000000000000000 ) ) ;
#17367 = DIRECTION ( 'NONE',  ( 0.000000000000000000, 1.000000000000000000, 0.000000000000000000 ) ) ;
#17368 = AXIS2_PLACEMENT_3D ( 'NONE', #2415, #21734, #16600 ) ;
#17369 = CARTESIAN_POINT ( 'NONE',  ( -37.94861706654396727, 9.802039414123830952, 12.35559950699420639 ) ) ;
#17370 = EDGE_CURVE ( 'NONE', #22982, #6819, #5781, .T. ) ;
#17371 = CARTESIAN_POINT ( 'NONE',  ( -20.64946329957944116, 25.40401715649331749, -16.50001200000000523 ) ) ;
#17372 = AXIS2_PLACEMENT_3D ( 'NONE', #15891, #25404, #23644 ) ;
#17373 = ORIENTED_EDGE ( 'NONE', *, *, #4084, .T. ) ;
#17374 = EDGE_CURVE ( 'NONE', #21024, #2038, #16563, .T. ) ;
#17375 = DIRECTION ( 'NONE',  ( -0.000000000000000000, -0.000000000000000000, 1.000000000000000000 ) ) ;
#17376 = CARTESIAN_POINT ( 'NONE',  ( -52.16608720827707657, -36.86186943028246787, 57.49999999999999289 ) ) ;
#17377 = FILL_AREA_STYLE_COLOUR ( '', #23668 ) ;
#17378 = CARTESIAN_POINT ( 'NONE',  ( -5.881244434206279514, -6.812559277181949646, -1.500000000000002665 ) ) ;
#17379 = ORIENTED_EDGE ( 'NONE', *, *, #15262, .T. ) ;
#17380 = AXIS2_PLACEMENT_3D ( 'NONE', #17434, #7606, #9949 ) ;
#17381 = PLANE ( 'NONE',  #28226 ) ;
#17382 = FACE_OUTER_BOUND ( 'NONE', #26679, .T. ) ;
#17383 = CARTESIAN_POINT ( 'NONE',  ( 9.928183626064983613, -13.85837025666176991, 5.652605728828375753 ) ) ;
#17384 = CARTESIAN_POINT ( 'NONE',  ( -15.42813811594281681, -7.209250886987517148, 18.55820869691756769 ) ) ;
#17385 = AXIS2_PLACEMENT_3D ( 'NONE', #5033, #343, #11912 ) ;
#17386 = FACE_OUTER_BOUND ( 'NONE', #4876, .T. ) ;
#17387 = VERTEX_POINT ( 'NONE', #28581 ) ;
#17388 = ORIENTED_EDGE ( 'NONE', *, *, #3298, .T. ) ;
#17389 = CARTESIAN_POINT ( 'NONE',  ( 9.248129367672067502, 2.094186647214772101, 1.500000000000001332 ) ) ;
#17390 = CARTESIAN_POINT ( 'NONE',  ( 39.83602371822922095, -11.57901747687539640, -19.50000000000000355 ) ) ;
#17391 = EDGE_CURVE ( 'NONE', #3254, #26855, #9251, .T. ) ;
#17392 = CARTESIAN_POINT ( 'NONE',  ( -3.668093106282626081, -42.33811009507338952, 34.60879219164162635 ) ) ;
#17393 = EDGE_CURVE ( 'NONE', #10427, #28059, #26185, .T. ) ;
#17394 = DIRECTION ( 'NONE',  ( -1.000000000000000000, 0.000000000000000000, 0.000000000000000000 ) ) ;
#17395 = ORIENTED_EDGE ( 'NONE', *, *, #26562, .F. ) ;
#17396 = SHAPE_DEFINITION_REPRESENTATION ( #28862, #7129 ) ;
#17397 = EDGE_CURVE ( 'NONE', #19418, #27728, #16038, .T. ) ;
#17398 = PLANE ( 'NONE',  #19395 ) ;
#17399 = VECTOR ( 'NONE', #16756, 1000.000000000000000 ) ;
#17400 = EDGE_CURVE ( 'NONE', #8016, #27429, #26703, .T. ) ;
#17401 = DIRECTION ( 'NONE',  ( 0.000000000000000000, -1.132880637372608986E-16, 1.000000000000000000 ) ) ;
#17402 = VERTEX_POINT ( 'NONE', #17817 ) ;
#17403 = CARTESIAN_POINT ( 'NONE',  ( 5.908622583341373691, 19.12614776545568418, 18.55820869691756769 ) ) ;
#17404 = EDGE_CURVE ( 'NONE', #8240, #23407, #14995, .T. ) ;
#17405 = DIRECTION ( 'NONE',  ( 1.000000000000000000, 0.000000000000000000, 0.000000000000000000 ) ) ;
#17406 = VECTOR ( 'NONE', #29483, 1000.000000000000000 ) ;
#17407 = CARTESIAN_POINT ( 'NONE',  ( -7.852931495992875988, -15.15760027748588179, 19.96568007040468373 ) ) ;
#17408 = CARTESIAN_POINT ( 'NONE',  ( -24.41908749150431035, -33.17108856314850840, 34.50932754554303017 ) ) ;
#17409 = ORIENTED_EDGE ( 'NONE', *, *, #7863, .F. ) ;
#17410 = ADVANCED_FACE ( 'NONE', ( #20145 ), #15146, .F. ) ;
#17411 = CARTESIAN_POINT ( 'NONE',  ( -9.056208293496290196, 2.810445847081948667, 13.00000000000000178 ) ) ;
#17412 = ADVANCED_FACE ( 'NONE', ( #12521 ), #22170, .F. ) ;
#17413 = DIRECTION ( 'NONE',  ( -1.000000000000000000, 0.000000000000000000, 0.000000000000000000 ) ) ;
#17414 = CARTESIAN_POINT ( 'NONE',  ( -57.50000000000001421, -50.00000000000000000, -87.50000000000000000 ) ) ;
#17415 = CARTESIAN_POINT ( 'NONE',  ( -4.163336342344337027E-14, 1.387778780781445676E-14, 1.500000000000000000 ) ) ;
#17416 = ORIENTED_EDGE ( 'NONE', *, *, #5172, .T. ) ;
#17417 = LINE ( 'NONE', #12900, #8833 ) ;
#17418 = CARTESIAN_POINT ( 'NONE',  ( 30.38302862529102200, 15.53680216053818874, 36.63232123326682199 ) ) ;
#17419 = B_SPLINE_SURFACE_WITH_KNOTS ( 'NONE', 3, 1, ( 
 ( #5217, #12400 ),
 ( #19559, #29079 ),
 ( #27515, #5835 ),
 ( #8337, #1305 ),
 ( #15335, #24865 ),
 ( #3648, #3502 ),
 ( #24692, #22203 ),
 ( #1148, #8505 ),
 ( #26902, #17851 ),
 ( #25010, #3187 ),
 ( #5522, #19875 ),
 ( #22366, #12868 ),
 ( #29392, #27050 ),
 ( #15173, #10661 ),
 ( #27369, #15492 ),
 ( #20019, #15025 ),
 ( #29539, #24539 ),
 ( #15644, #17531 ),
 ( #3336, #1003 ),
 ( #13163, #22656 ),
 ( #10825, #29863 ),
 ( #17682, #18007 ),
 ( #6135, #25156 ),
 ( #3800, #13324 ),
 ( #18519, #13077 ),
 ( #30210, #25220 ),
 ( #1672, #15702 ),
 ( #1370, #13228 ),
 ( #15393, #29916 ),
 ( #8554, #3555 ),
 ( #16016, #8698 ) ),
 .UNSPECIFIED., .F., .F., .F.,
 ( 4, 3, 3, 3, 3, 3, 3, 3, 3, 3, 4 ),
 ( 2, 2 ),
 ( 0.000000000000000000, 0.05425176834609614362, 0.1085332949128348518, 0.1623767749169379715, 0.2157504826133058717, 0.2688657508888169789, 0.3218907763505471364, 0.3749548578363334772, 0.4282048033836237666, 0.4818374082110496448, 0.4999999999131651274 ),
 ( 0.000000000000000000, 1.000000000000000000 ),
 .UNSPECIFIED. ) ;
#17420 = CARTESIAN_POINT ( 'NONE',  ( -4.163336342344337027E-14, 1.387778780781445676E-14, 1.500000000000000000 ) ) ;
#17421 = CARTESIAN_POINT ( 'NONE',  ( 28.37932450449293853, 10.51822134874671022, -1.500000000000000000 ) ) ;
#17422 = DIRECTION ( 'NONE',  ( 0.1423148382732852546, -0.9898214418809327952, 0.000000000000000000 ) ) ;
#17423 = DIRECTION ( 'NONE',  ( -1.000000000000000000, 0.000000000000000000, 0.000000000000000000 ) ) ;
#17424 = DIRECTION ( 'NONE',  ( -0.000000000000000000, -1.000000000000000000, -0.000000000000000000 ) ) ;
#17425 = VERTEX_POINT ( 'NONE', #29192 ) ;
#17426 = EDGE_CURVE ( 'NONE', #30256, #549, #275, .T. ) ;
#17427 = DIRECTION ( 'NONE',  ( -0.000000000000000000, -1.000000000000000000, -0.000000000000000000 ) ) ;
#17428 = AXIS2_PLACEMENT_3D ( 'NONE', #21092, #4125, #6922 ) ;
#17429 = DIRECTION ( 'NONE',  ( -0.000000000000000000, 0.000000000000000000, -1.000000000000000000 ) ) ;
#17430 = ORIENTED_EDGE ( 'NONE', *, *, #8311, .F. ) ;
#17431 = VERTEX_POINT ( 'NONE', #648 ) ;
#17432 = CARTESIAN_POINT ( 'NONE',  ( -50.00000000000000000, -70.00000000000000000, 12.49999999999999112 ) ) ;
#17433 = EDGE_CURVE ( 'NONE', #20557, #26276, #17342, .T. ) ;
#17434 = CARTESIAN_POINT ( 'NONE',  ( -2.081668171172168513E-14, 90.00000000000001421, 37.49999999999999289 ) ) ;
#17435 = EDGE_CURVE ( 'NONE', #3576, #3847, #8259, .T. ) ;
#17436 = EDGE_LOOP ( 'NONE', ( #460, #22643 ) ) ;
#17437 = AXIS2_PLACEMENT_3D ( 'NONE', #4294, #7104, #11629 ) ;
#17438 = CARTESIAN_POINT ( 'NONE',  ( -27.98100949438103413, -24.85668482956322123, 27.50000000000001066 ) ) ;
#17439 = CARTESIAN_POINT ( 'NONE',  ( -9.248129367672079937, -2.094186647214709485, 1.500000000000001332 ) ) ;
#17440 = ORIENTED_EDGE ( 'NONE', *, *, #12471, .F. ) ;
#17441 = CARTESIAN_POINT ( 'NONE',  ( -19.71348387055304130, 3.477795851889708523, 6.864725433338323413 ) ) ;
#17442 = CARTESIAN_POINT ( 'NONE',  ( 17.90972305382299368, -8.901787470106556910, 6.781503518395063601 ) ) ;
#17443 = DIRECTION ( 'NONE',  ( 0.000000000000000000, 0.000000000000000000, -1.000000000000000000 ) ) ;
#17444 = ORIENTED_EDGE ( 'NONE', *, *, #26840, .F. ) ;
#17445 = CARTESIAN_POINT ( 'NONE',  ( 12.24063095261064404, 4.490763173670002217, 1.500000000000001332 ) ) ;
#17446 = ORIENTED_EDGE ( 'NONE', *, *, #4806, .F. ) ;
#17447 = CIRCLE ( 'NONE', #12469, 6.600000000000001421 ) ;
#17448 = CARTESIAN_POINT ( 'NONE',  ( 7.730328572437743517, -4.608906612435629491, -1.500000000000002220 ) ) ;
#17449 = ORIENTED_EDGE ( 'NONE', *, *, #2683, .T. ) ;
#17450 = CARTESIAN_POINT ( 'NONE',  ( -5.971396161871752817, 19.08775596758252036, 20.34789198813115263 ) ) ;
#17451 = DIRECTION ( 'NONE',  ( -0.9895723101232632990, 0.1430086711943935607, 0.01718030851067640571 ) ) ;
#17452 = CARTESIAN_POINT ( 'NONE',  ( 19.63374410927882607, 3.902325345048613947, 7.366751648393900176 ) ) ;
#17453 = DIRECTION ( 'NONE',  ( -1.000000000000000000, 0.000000000000000000, 0.000000000000000000 ) ) ;
#17454 = VECTOR ( 'NONE', #22018, 1000.000000000000114 ) ;
#17455 = CARTESIAN_POINT ( 'NONE',  ( -17.28117534813046774, 38.12494209667251255, 29.23509795125549005 ) ) ;
#17456 = DIRECTION ( 'NONE',  ( 0.5503133621338236470, -0.8349582046168341209, 0.000000000000000000 ) ) ;
#17457 = CARTESIAN_POINT ( 'NONE',  ( 17.26937953831880534, -14.36006998371588317, -1.500000000000000000 ) ) ;
#17458 = B_SPLINE_CURVE_WITH_KNOTS ( 'NONE', 3,
 ( #10146, #19651, #29172, #24492, #3136, #12659, #22153, #27007, #6656, #16173, #27730, #1984, #30512, #28028 ),
 .UNSPECIFIED., .F., .F.,
 ( 4, 2, 2, 2, 2, 2, 4 ),
 ( 2.108610145883729832E-07, 0.0004867403503157766501, 0.0009732698396169649517, 0.001459799328918153253, 0.001946328818219341663, 0.002919387796821711761, 0.003892446775424082510 ),
 .UNSPECIFIED. ) ;
#17459 = EDGE_CURVE ( 'NONE', #12805, #12720, #12236, .T. ) ;
#17460 = CARTESIAN_POINT ( 'NONE',  ( 10.27954044202352968, -17.17695407163359889, 6.420335371522007506 ) ) ;
#17461 = EDGE_CURVE ( 'NONE', #26638, #7128, #7999, .T. ) ;
#17462 = CARTESIAN_POINT ( 'NONE',  ( 39.99999999999998579, 80.00000000000001421, 22.49999999999999289 ) ) ;
#17463 = DIRECTION ( 'NONE',  ( -0.4495526574063634095, -0.8932538319083086487, 0.000000000000000000 ) ) ;
#17464 = FACE_BOUND ( 'NONE', #21499, .T. ) ;
#17465 = EDGE_LOOP ( 'NONE', ( #13422, #14431, #23140, #17284 ) ) ;
#17466 = ORIENTED_EDGE ( 'NONE', *, *, #26931, .T. ) ;
#17467 = CARTESIAN_POINT ( 'NONE',  ( 17.90987090234840906, -8.901490003858832267, 19.21471108562413832 ) ) ;
#17468 = CARTESIAN_POINT ( 'NONE',  ( 43.34097750826428097, 11.89502811014149763, -1.500000000000000444 ) ) ;
#17469 = CARTESIAN_POINT ( 'NONE',  ( 12.72536390617885438, -2.839914339433650348, 24.50000000000000000 ) ) ;
#17470 = VERTEX_POINT ( 'NONE', #3614 ) ;
#17471 = CARTESIAN_POINT ( 'NONE',  ( -4.163336342344337027E-14, 1.387778780781445676E-14, 1.500000000000000000 ) ) ;
#17472 = CIRCLE ( 'NONE', #24945, 9.084132297865673777 ) ;
#17473 = CARTESIAN_POINT ( 'NONE',  ( -15.16120755655624741, 17.22181377296911720, 1.500000000000000000 ) ) ;
#17474 = CARTESIAN_POINT ( 'NONE',  ( 5.780652116621846304, 19.14677724775280154, 5.775318986477950389 ) ) ;
#17475 = ORIENTED_EDGE ( 'NONE', *, *, #7671, .F. ) ;
#17476 = CARTESIAN_POINT ( 'NONE',  ( -10.40347366321433142, -17.08171436691437606, 20.34789198813115263 ) ) ;
#17477 = CARTESIAN_POINT ( 'NONE',  ( 14.23411040819766882, 14.07463391211592096, 6.341840715582230281 ) ) ;
#17478 = CARTESIAN_POINT ( 'NONE',  ( 16.74328840634222715, 3.194145055459935101, 7.652108011868850035 ) ) ;
#17479 = ORIENTED_EDGE ( 'NONE', *, *, #25619, .T. ) ;
#17480 = CARTESIAN_POINT ( 'NONE',  ( 49.99999999999998579, -67.00000000000000000, 62.49999999999999289 ) ) ;
#17481 = VERTEX_POINT ( 'NONE', #970 ) ;
#17482 = CARTESIAN_POINT ( 'NONE',  ( 3.395021109945009385, -30.50000000000000711, 1.500000000000001332 ) ) ;
#17483 = CARTESIAN_POINT ( 'NONE',  ( 6.974883619896790954, 5.687793815610376669, -3.621320343559650379 ) ) ;
#17484 = DIRECTION ( 'NONE',  ( 0.000000000000000000, 0.000000000000000000, 1.000000000000000000 ) ) ;
#17485 = ORIENTED_EDGE ( 'NONE', *, *, #823, .F. ) ;
#17486 = DIRECTION ( 'NONE',  ( 0.000000000000000000, 1.000000000000000000, 0.000000000000000000 ) ) ;
#17487 = VECTOR ( 'NONE', #30590, 1000.000000000000000 ) ;
#17488 = CARTESIAN_POINT ( 'NONE',  ( 24.03448224033878944, 8.660042335149841009, 49.47829057475697567 ) ) ;
#17489 = CARTESIAN_POINT ( 'NONE',  ( 0.000000000000000000, 0.000000000000000000, 1.500000000000001332 ) ) ;
#17490 = CARTESIAN_POINT ( 'NONE',  ( 25.91119823319791848, 27.43797854297901750, 34.50000000000000000 ) ) ;
#17491 = CIRCLE ( 'NONE', #19999, 9.084132297865673777 ) ;
#17492 = CARTESIAN_POINT ( 'NONE',  ( -11.52197458429825083, 37.50933785548062360, 27.50000000000001066 ) ) ;
#17493 = CARTESIAN_POINT ( 'NONE',  ( 9.048061653868892051, -14.41834352799975427, 19.66989035740801839 ) ) ;
#17494 = CARTESIAN_POINT ( 'NONE',  ( 10.25423333689187544, -17.17121715837755147, 19.21471108562414898 ) ) ;
#17495 = ORIENTED_EDGE ( 'NONE', *, *, #15496, .F. ) ;
#17496 = CARTESIAN_POINT ( 'NONE',  ( -24.58208797071834795, -7.298293523701643082, 49.35779847067230719 ) ) ;
#17497 = EDGE_CURVE ( 'NONE', #19042, #7607, #4790, .T. ) ;
#17498 = CARTESIAN_POINT ( 'NONE',  ( -15.64089046717304399, 12.49323067438739621, 18.44527579819791185 ) ) ;
#17499 = CARTESIAN_POINT ( 'NONE',  ( 33.42925964089140933, 11.06161099612213405, 35.54550565580007060 ) ) ;
#17500 = ORIENTED_EDGE ( 'NONE', *, *, #11301, .F. ) ;
#17501 = CARTESIAN_POINT ( 'NONE',  ( 32.76094438725117186, -23.06299619967057168, 8.000000000000007105 ) ) ;
#17502 = CARTESIAN_POINT ( 'NONE',  ( -45.88720696345781391, 69.36824176953101073, 60.58574796622433212 ) ) ;
#17503 = CARTESIAN_POINT ( 'NONE',  ( -5.352643706120520761, -7.827050521741861999, 21.50000000000000000 ) ) ;
#17504 = CARTESIAN_POINT ( 'NONE',  ( 0.000000000000000000, 0.000000000000000000, 92.49999999999998579 ) ) ;
#17505 = CARTESIAN_POINT ( 'NONE',  ( -31.18700685316100163, -26.11823559932341610, -1.500000000000000000 ) ) ;
#17506 = CARTESIAN_POINT ( 'NONE',  ( 0.000000000000000000, 42.50000000000000000, 27.50000000000000355 ) ) ;
#17507 = CARTESIAN_POINT ( 'NONE',  ( 17.79450790306045604, 37.82695112826932160, 34.52540950801754605 ) ) ;
#17508 = CARTESIAN_POINT ( 'NONE',  ( 19.55517958221000185, 4.194633687229720742, 6.523620417364448976 ) ) ;
#17509 = ORIENTED_EDGE ( 'NONE', *, *, #8836, .F. ) ;
#17510 = VECTOR ( 'NONE', #27862, 1000.000000000000000 ) ;
#17511 = CARTESIAN_POINT ( 'NONE',  ( -8.499586724479453181, -2.959227181723774525, 21.50000000000000000 ) ) ;
#17512 = PLANE ( 'NONE',  #26646 ) ;
#17513 = DIRECTION ( 'NONE',  ( 1.000000000000000000, 0.000000000000000000, 0.000000000000000000 ) ) ;
#17514 = ORIENTED_EDGE ( 'NONE', *, *, #8094, .T. ) ;
#17515 = EDGE_LOOP ( 'NONE', ( #28906, #26803, #29060, #30711 ) ) ;
#17516 = CARTESIAN_POINT ( 'NONE',  ( -10.08096377525214926, -17.27393813307045178, 7.528076282304592581 ) ) ;
#17517 = ORIENTED_EDGE ( 'NONE', *, *, #29772, .F. ) ;
#17518 = DIRECTION ( 'NONE',  ( 0.000000000000000000, 1.000000000000000000, 0.000000000000000000 ) ) ;
#17519 = CARTESIAN_POINT ( 'NONE',  ( -19.49586959400445707, 33.20761599285713572, 34.49999999999998579 ) ) ;
#17520 = VECTOR ( 'NONE', #15889, 1000.000000000000000 ) ;
#17521 = DIRECTION ( 'NONE',  ( 0.000000000000000000, 0.000000000000000000, 1.000000000000000000 ) ) ;
#17522 = CARTESIAN_POINT ( 'NONE',  ( -34.49515668447323691, 19.83906540583472022, 8.223984938597787675 ) ) ;
#17523 = CARTESIAN_POINT ( 'NONE',  ( -23.91679456219655364, 22.99653376284463135, -16.50001200000000523 ) ) ;
#17524 = ADVANCED_FACE ( 'NONE', ( #500 ), #10020, .F. ) ;
#17525 = CARTESIAN_POINT ( 'NONE',  ( -6.587096388939656322, -18.88412458026101604, 24.50000000000000000 ) ) ;
#17526 = CARTESIAN_POINT ( 'NONE',  ( 3.896869771148438577, -16.82098518409776489, 1.500000000000000000 ) ) ;
#17527 = CARTESIAN_POINT ( 'NONE',  ( 0.8597189258598705308, -17.02598424914432940, 5.652605728828374865 ) ) ;
#17528 = CARTESIAN_POINT ( 'NONE',  ( 0.1262659238204208167, 8.999114229549594057, -3.621320343559650379 ) ) ;
#17529 = ORIENTED_EDGE ( 'NONE', *, *, #23142, .T. ) ;
#17530 = AXIS2_PLACEMENT_3D ( 'NONE', #26531, #10003, #7359 ) ;
#17531 = CARTESIAN_POINT ( 'NONE',  ( -9.351023488831160080, -14.22394595406099427, 19.00652017443069752 ) ) ;
#17532 = DIRECTION ( 'NONE',  ( 0.1411672138529631859, 0.9899857664294936521, 0.000000000000000000 ) ) ;
#17533 = CARTESIAN_POINT ( 'NONE',  ( -6.460166075217649961, 15.80732207284230029, 6.341840715582230281 ) ) ;
#17534 = EDGE_CURVE ( 'NONE', #27429, #584, #14744, .T. ) ;
#17535 = CARTESIAN_POINT ( 'NONE',  ( 10.56600709331201671, -13.41035981659392462, 7.196036389296800451 ) ) ;
#17536 = EDGE_CURVE ( 'NONE', #509, #977, #7525, .T. ) ;
#17537 = CARTESIAN_POINT ( 'NONE',  ( 20.65888525914375862, -38.75220717792901581, -19.50000000000000355 ) ) ;
#17538 = CARTESIAN_POINT ( 'NONE',  ( -33.42925964089141644, -11.06161099612212695, 35.54550565580013455 ) ) ;
#17539 = ORIENTED_EDGE ( 'NONE', *, *, #11841, .T. ) ;
#17540 = ORIENTED_EDGE ( 'NONE', *, *, #27469, .T. ) ;
#17541 = CARTESIAN_POINT ( 'NONE',  ( -3.221450758838616757, -1.621276839356792454, 1.500000000000000000 ) ) ;
#17542 = DIRECTION ( 'NONE',  ( -1.000000000000000000, 0.000000000000000000, 0.000000000000000000 ) ) ;
#17543 = CARTESIAN_POINT ( 'NONE',  ( 0.4876298400482597661, -42.50362390527760681, 28.83943401234160930 ) ) ;
#17545 = VECTOR ( 'NONE', #3253, 1000.000000000000000 ) ;
#17544 = CARTESIAN_POINT ( 'NONE',  ( -0.2239719228550731966, -17.01994463034866101, 6.782064869129511564 ) ) ;
#17546 = EDGE_LOOP ( 'NONE', ( #10458, #30163, #5177, #17199 ) ) ;
#17547 = CARTESIAN_POINT ( 'NONE',  ( 16.01802636628489296, -5.877265577766301874, 18.45571264222804331 ) ) ;
#17548 = DIRECTION ( 'NONE',  ( -1.000000000000000000, 0.000000000000000000, 0.000000000000000000 ) ) ;
#17549 = EDGE_CURVE ( 'NONE', #11497, #20113, #7780, .T. ) ;
#17550 = EDGE_LOOP ( 'NONE', ( #18420, #25924 ) ) ;
#17551 = CARTESIAN_POINT ( 'NONE',  ( 4.045241160018713700, 16.55840174602106529, 18.34798005862930026 ) ) ;
#17552 = CIRCLE ( 'NONE', #27024, 22.49999999999996447 ) ;
#17553 = DIRECTION ( 'NONE',  ( -1.000000000000000000, -5.125319360840571077E-16, 0.000000000000000000 ) ) ;
#17554 = CARTESIAN_POINT ( 'NONE',  ( -27.23683592356784544, -25.89410312378974410, 37.49999999984879651 ) ) ;
#17555 = ORIENTED_EDGE ( 'NONE', *, *, #24844, .F. ) ;
#17556 = CARTESIAN_POINT ( 'NONE',  ( 8.860628911697515875, 8.184276679720483116, 1.500000000000000000 ) ) ;
#17557 = EDGE_CURVE ( 'NONE', #11562, #5756, #14837, .T. ) ;
#17558 = CARTESIAN_POINT ( 'NONE',  ( 0.000000000000000000, 0.000000000000000000, 62.49999999999999289 ) ) ;
#17559 = CARTESIAN_POINT ( 'NONE',  ( -19.80980381183504235, 2.754394816484158515, 18.37250658438899009 ) ) ;
#17560 = VERTEX_POINT ( 'NONE', #29968 ) ;
#17561 = CARTESIAN_POINT ( 'NONE',  ( -15.25992540518562635, -7.581593484474010047, 5.670038381137163519 ) ) ;
#17562 = VECTOR ( 'NONE', #24243, 1000.000000000000000 ) ;
#17563 = CARTESIAN_POINT ( 'NONE',  ( 12.93287820104972141, 11.07039438042774293, 19.85270094495842130 ) ) ;
#17564 = EDGE_CURVE ( 'NONE', #22385, #20718, #20223, .T. ) ;
#17565 = CARTESIAN_POINT ( 'NONE',  ( 16.17629920997981330, -5.470921186997150798, 6.329955581934032516 ) ) ;
#17566 = EDGE_CURVE ( 'NONE', #4103, #26490, #18112, .T. ) ;
#17567 = CARTESIAN_POINT ( 'NONE',  ( -7.483314773547907528, 75.00000000000001421, 50.49999999999998579 ) ) ;
#17568 = CARTESIAN_POINT ( 'NONE',  ( -17.06430796154857887, 0.6673913134784715817, 6.917457548096561659 ) ) ;
#17569 = DIRECTION ( 'NONE',  ( -0.7557495743542581579, -0.6548607339452852116, 0.000000000000000000 ) ) ;
#17570 = CARTESIAN_POINT ( 'NONE',  ( 36.43862201448670390, -15.16126941994617283, 16.62946957978847351 ) ) ;
#17571 = DIRECTION ( 'NONE',  ( 0.000000000000000000, 1.000000000000000000, 0.000000000000000000 ) ) ;
#17572 = EDGE_LOOP ( 'NONE', ( #13040, #516, #22120, #9133 ) ) ;
#17573 = ADVANCED_FACE ( 'NONE', ( #6413 ), #7896, .T. ) ;
#17574 = CARTESIAN_POINT ( 'NONE',  ( 33.21329855679435639, -9.207353758468070026, 40.53414655261587995 ) ) ;
#17575 = CARTESIAN_POINT ( 'NONE',  ( -4.163336342344337027E-14, 1.387778780781445676E-14, -1.500000000000000000 ) ) ;
#17576 = VERTEX_POINT ( 'NONE', #7331 ) ;
#17577 = ORIENTED_EDGE ( 'NONE', *, *, #23411, .F. ) ;
#17578 = CARTESIAN_POINT ( 'NONE',  ( -13.88429941593315853, -16.69721919944146649, -1.500000000000000000 ) ) ;
#17579 = CARTESIAN_POINT ( 'NONE',  ( 37.99999999999999289, 80.00000000000000000, 0.000000000000000000 ) ) ;
#17580 = EDGE_CURVE ( 'NONE', #2431, #15951, #9056, .T. ) ;
#17581 = DIRECTION ( 'NONE',  ( 1.000000000000000000, 0.000000000000000000, 0.000000000000000000 ) ) ;
#17582 = CARTESIAN_POINT ( 'NONE',  ( -35.15416861624421330, -8.598791122201292936, 27.50000000000000355 ) ) ;
#17583 = EDGE_CURVE ( 'NONE', #18859, #21029, #26041, .T. ) ;
#17584 = CARTESIAN_POINT ( 'NONE',  ( 12.99901289864994958, 10.98932263627886385, 19.56050940960062690 ) ) ;
#17585 = EDGE_CURVE ( 'NONE', #17335, #16359, #16682, .T. ) ;
#17586 = AXIS2_PLACEMENT_3D ( 'NONE', #678, #10046, #19555 ) ;
#17587 = VERTEX_POINT ( 'NONE', #4520 ) ;
#17588 = ORIENTED_EDGE ( 'NONE', *, *, #6123, .F. ) ;
#17589 = CIRCLE ( 'NONE', #4137, 0.7441270634457319844 ) ;
#17590 = CARTESIAN_POINT ( 'NONE',  ( 5.881244434206234217, 6.812559277181991391, 1.500000000000001332 ) ) ;
#17591 = CARTESIAN_POINT ( 'NONE',  ( 19.68627777834516479, 3.628879393376897244, 20.25542030744407640 ) ) ;
#17592 = CARTESIAN_POINT ( 'NONE',  ( 40.57341518701483096, 0.5662347448574781561, -16.50000000000000000 ) ) ;
#17593 = ORIENTED_EDGE ( 'NONE', *, *, #6776, .T. ) ;
#17594 = CYLINDRICAL_SURFACE ( 'NONE', #23797, 0.7500000000000011102 ) ;
#17595 = CARTESIAN_POINT ( 'NONE',  ( 39.87350638640253919, -4.706224724400470016, -11.49999999999999645 ) ) ;
#17596 = ORIENTED_EDGE ( 'NONE', *, *, #17370, .T. ) ;
#17597 = EDGE_CURVE ( 'NONE', #17807, #22741, #30205, .T. ) ;
#17598 = SURFACE_SIDE_STYLE ('',( #24761 ) ) ;
#17599 = EDGE_CURVE ( 'NONE', #8468, #8832, #12772, .T. ) ;
#17600 = CARTESIAN_POINT ( 'NONE',  ( 20.71335220384823117, -27.86167394782616213, -16.50001200000000168 ) ) ;
#17601 = B_SPLINE_SURFACE_WITH_KNOTS ( 'NONE', 3, 1, ( 
 ( #10454, #22755 ),
 ( #20430, #19968 ),
 ( #17628, #15587 ),
 ( #27300, #5930 ),
 ( #6077, #29799 ),
 ( #29487, #13111 ),
 ( #26999, #12956 ),
 ( #3747, #29950 ),
 ( #8587, #6233 ),
 ( #24950, #1977 ),
 ( #1097, #11499 ),
 ( #29332, #7974 ),
 ( #17477, #17947 ),
 ( #29637, #1253 ),
 ( #10760, #27457 ),
 ( #16629, #16476 ),
 ( #18663, #28169 ),
 ( #12110, #95 ),
 ( #6800, #14121 ),
 ( #5084, #30815 ),
 ( #19272, #23789 ),
 ( #9756, #9613 ),
 ( #18822, #7263 ),
 ( #25992, #6965 ),
 ( #16324, #28790 ),
 ( #2592, #11961 ),
 ( #23946, #13984 ),
 ( #14595, #24100 ),
 ( #23625, #9296 ),
 ( #28638, #2748 ),
 ( #18978, #21609 ) ),
 .UNSPECIFIED., .F., .F., .F.,
 ( 4, 3, 3, 3, 3, 3, 3, 3, 3, 3, 4 ),
 ( 2, 2 ),
 ( 0.4999999998345681651, 0.5360336730431942698, 0.5907651151589017324, 0.6456034593241839481, 0.6998270958050443191, 0.7529536536315944995, 0.8052385063053264513, 0.8575343587103996246, 0.9106564858195047574, 0.9648414833209688624, 1.000000006602610014 ),
 ( 0.000000000000000000, 1.000000000000000000 ),
 .UNSPECIFIED. ) ;
#17602 = DIRECTION ( 'NONE',  ( -0.000000000000000000, -0.000000000000000000, -1.000000000000000000 ) ) ;
#17603 = CARTESIAN_POINT ( 'NONE',  ( -33.13218612630368654, 7.028748154183637631, -1.942616967526160643 ) ) ;
#17604 = ADVANCED_FACE ( 'NONE', ( #4673 ), #18714, .F. ) ;
#17605 = CARTESIAN_POINT ( 'NONE',  ( 1.665992581745963985, -16.99218467486907258, 6.147510495896842286 ) ) ;
#17606 = CARTESIAN_POINT ( 'NONE',  ( -4.506343322667617279, 42.22116422339769315, 28.86378313756725333 ) ) ;
#17607 = VECTOR ( 'NONE', #4648, 1000.000000000000000 ) ;
#17608 = FACE_OUTER_BOUND ( 'NONE', #22799, .T. ) ;
#17609 = DIRECTION ( 'NONE',  ( 1.000000000000000000, 0.000000000000000000, 0.000000000000000000 ) ) ;
#17610 = ORIENTED_EDGE ( 'NONE', *, *, #24838, .F. ) ;
#17611 = AXIS2_PLACEMENT_3D ( 'NONE', #24002, #28703, #2651 ) ;
#17612 = CARTESIAN_POINT ( 'NONE',  ( -19.86132161767506332, 2.497832813224998727, 5.652196082364320695 ) ) ;
#17613 = EDGE_CURVE ( 'NONE', #11152, #14718, #25212, .T. ) ;
#17614 = CARTESIAN_POINT ( 'NONE',  ( -29.55668231273981661, 27.73034433992416936, 9.346428711510588627 ) ) ;
#17615 = CARTESIAN_POINT ( 'NONE',  ( -8.884323311075783991, -1.438332125858144295, 21.50000000000000000 ) ) ;
#17616 = ORIENTED_EDGE ( 'NONE', *, *, #8241, .T. ) ;
#17617 = ORIENTED_EDGE ( 'NONE', *, *, #5134, .F. ) ;
#17618 = CARTESIAN_POINT ( 'NONE',  ( 17.96625477203412657, -8.787278772463423593, 19.85261563089510517 ) ) ;
#17619 = CARTESIAN_POINT ( 'NONE',  ( -5.971396161871752817, 19.08775596758251680, 7.652108011868850035 ) ) ;
#17620 = EDGE_CURVE ( 'NONE', #27015, #25122, #28693, .T. ) ;
#17621 = CARTESIAN_POINT ( 'NONE',  ( -5.435829780283180312, 16.15227280059888315, 7.652108011868850035 ) ) ;
#17622 = ORIENTED_EDGE ( 'NONE', *, *, #24195, .F. ) ;
#17623 = CARTESIAN_POINT ( 'NONE',  ( -40.00000000000000000, 90.00000000000001421, 52.49999999999999289 ) ) ;
#17624 = CARTESIAN_POINT ( 'NONE',  ( 5.422617586916723020, 19.25129646183500398, 7.652108011868850035 ) ) ;
#17625 = EDGE_LOOP ( 'NONE', ( #30404, #5429 ) ) ;
#17626 = AXIS2_PLACEMENT_3D ( 'NONE', #29537, #5831, #29074 ) ;
#17627 = CARTESIAN_POINT ( 'NONE',  ( -10.51513057463694523, -17.01270198993485394, 20.34789198813115263 ) ) ;
#17628 = CARTESIAN_POINT ( 'NONE',  ( 14.79201625507351636, 13.48748956535167487, 5.661398277488801867 ) ) ;
#17629 = CARTESIAN_POINT ( 'NONE',  ( 19.89739966441223018, 2.193321724558644714, 6.755862304746362845 ) ) ;
#17630 = ORIENTED_EDGE ( 'NONE', *, *, #17006, .F. ) ;
#17631 = CARTESIAN_POINT ( 'NONE',  ( 6.812559277181973627, -5.881244434206257310, 1.500000000000001332 ) ) ;
#17632 = ORIENTED_EDGE ( 'NONE', *, *, #19082, .F. ) ;
#17633 = EDGE_CURVE ( 'NONE', #9483, #15816, #25319, .T. ) ;
#17634 = CARTESIAN_POINT ( 'NONE',  ( -13.55077504527628562, 10.35587614683493918, 18.34938820207544552 ) ) ;
#17635 = AXIS2_PLACEMENT_3D ( 'NONE', #8188, #26916, #17694 ) ;
#17636 = PRODUCT_DEFINITION_CONTEXT ( 'detailed design', #2417, 'design' ) ;
#17637 = ADVANCED_FACE ( 'NONE', ( #28080 ), #20893, .F. ) ;
#17638 = CARTESIAN_POINT ( 'NONE',  ( 31.46108752401734066, -15.19043599309334169, 35.82118098715091747 ) ) ;
#17639 = ORIENTED_EDGE ( 'NONE', *, *, #22496, .T. ) ;
#17640 = CARTESIAN_POINT ( 'NONE',  ( 5.231931633751616850, 19.32210152104737233, 7.652108011868850035 ) ) ;
#17641 = DIRECTION ( 'NONE',  ( 1.000000000000000000, 0.000000000000000000, 0.000000000000000000 ) ) ;
#17642 = DIRECTION ( 'NONE',  ( 0.000000000000000000, 0.000000000000000000, -1.000000000000000000 ) ) ;
#17643 = CARTESIAN_POINT ( 'NONE',  ( 34.45950848030155100, 11.47319617667155711, 34.50000000000000000 ) ) ;
#17644 = LINE ( 'NONE', #15136, #30324 ) ;
#17645 = CARTESIAN_POINT ( 'NONE',  ( 9.002475149809907151, -14.44561766934883273, 19.33715507985239412 ) ) ;
#17646 = CARTESIAN_POINT ( 'NONE',  ( 30.38302862529101489, 15.53680216053818519, 40.87496192038609877 ) ) ;
#17647 = VERTEX_POINT ( 'NONE', #11695 ) ;
#17648 = CARTESIAN_POINT ( 'NONE',  ( 25.88640477275122009, 6.345529225273955909, 48.34755156421744005 ) ) ;
#17649 = B_SPLINE_CURVE_WITH_KNOTS ( 'NONE', 3,
 ( #2252, #9447, #6488, #18803, #28323, #27864, #16150, #18503, #16604, #30636, #21115, #6636, #11624, #18962, #16305, #28472, #7098, #4143 ),
 .UNSPECIFIED., .F., .F.,
 ( 4, 2, 2, 2, 2, 2, 2, 2, 4 ),
 ( 0.003174295595554298306, 0.003570702171545536707, 0.003967108747536774241, 0.004363515323528012642, 0.004759921899519251043, 0.005156328475510488576, 0.005552735051501727845, 0.005949141627492967113, 0.006345548203484206382 ),
 .UNSPECIFIED. ) ;
#17650 = CARTESIAN_POINT ( 'NONE',  ( -31.18700685316050780, 26.11823559932051353, -1.500000000000000000 ) ) ;
#17651 = CARTESIAN_POINT ( 'NONE',  ( -23.09047454507859243, 11.74540567832115912, 44.85144129262233292 ) ) ;
#17652 = ORIENTED_EDGE ( 'NONE', *, *, #16413, .F. ) ;
#17653 = VECTOR ( 'NONE', #27452, 1000.000000000000000 ) ;
#17654 = CARTESIAN_POINT ( 'NONE',  ( 31.80160417541173956, -24.60589111005866059, 17.86404149739671965 ) ) ;
#17655 = CARTESIAN_POINT ( 'NONE',  ( 0.000000000000000000, -2.322405306613848348E-14, 117.5000000000000000 ) ) ;
#17656 = CARTESIAN_POINT ( 'NONE',  ( -15.26094448139682846, 12.92753815214665636, 18.34726407865098707 ) ) ;
#17657 = FACE_OUTER_BOUND ( 'NONE', #17725, .T. ) ;
#17658 = DIRECTION ( 'NONE',  ( -0.000000000000000000, -0.000000000000000000, 1.000000000000000000 ) ) ;
#17659 = CARTESIAN_POINT ( 'NONE',  ( 16.81826667484149240, 2.692788315428430224, 7.526951045817047437 ) ) ;
#17660 = VERTEX_POINT ( 'NONE', #6702 ) ;
#17661 = CARTESIAN_POINT ( 'NONE',  ( -33.03705654931147251, -8.970011997839668183, 36.52435908506018336 ) ) ;
#17662 = CARTESIAN_POINT ( 'NONE',  ( -4.163336342344337027E-14, 1.387778780781445676E-14, 1.500000000000000000 ) ) ;
#17663 = CYLINDRICAL_SURFACE ( 'NONE', #23912, 0.7500000000000006661 ) ;
#17664 = VERTEX_POINT ( 'NONE', #144 ) ;
#17665 = ORIENTED_EDGE ( 'NONE', *, *, #11878, .F. ) ;
#17666 = CARTESIAN_POINT ( 'NONE',  ( -9.033033306777449312, 0.9621688436940326605, 13.22130136205108819 ) ) ;
#17667 = B_SPLINE_CURVE_WITH_KNOTS ( 'NONE', 3,
 ( #12041, #4402, #16873, #14528 ),
 .UNSPECIFIED., .F., .F.,
 ( 4, 4 ),
 ( 0.002976194933398901288, 0.003711256114093793891 ),
 .UNSPECIFIED. ) ;
#17668 = EDGE_CURVE ( 'NONE', #14218, #27309, #26708, .T. ) ;
#17669 = EDGE_LOOP ( 'NONE', ( #573, #5042, #27244, #25796 ) ) ;
#17670 = CARTESIAN_POINT ( 'NONE',  ( 24.03057240117690441, -26.57182937991349903, -1.500000000000001332 ) ) ;
#17671 = EDGE_CURVE ( 'NONE', #1048, #22947, #11180, .T. ) ;
#17672 = DIRECTION ( 'NONE',  ( 0.1423148382732746797, -0.9898214418809342385, 0.000000000000000000 ) ) ;
#17673 = DIRECTION ( 'NONE',  ( -0.000000000000000000, 0.000000000000000000, 1.000000000000000000 ) ) ;
#17674 = DIRECTION ( 'NONE',  ( 0.000000000000000000, 0.000000000000000000, -1.000000000000000000 ) ) ;
#17675 = CARTESIAN_POINT ( 'NONE',  ( 28.37932450449293853, 10.51822134874671022, 1.500000000000000000 ) ) ;
#17676 = CARTESIAN_POINT ( 'NONE',  ( -11.03614041005515567, -16.67970391259860108, 7.454139397117727661 ) ) ;
#17677 = PLANE ( 'NONE',  #138 ) ;
#17679 = CARTESIAN_POINT ( 'NONE',  ( 0.5800982118606525795, -20.00934090639729135, 5.678370764302467677 ) ) ;
#17678 = AXIS2_PLACEMENT_3D ( 'NONE', #5041, #15004, #21556 ) ;
#17680 = CYLINDRICAL_SURFACE ( 'NONE', #22086, 1.447898107987198646 ) ;
#17681 = ORIENTED_EDGE ( 'NONE', *, *, #30016, .F. ) ;
#17682 = CARTESIAN_POINT ( 'NONE',  ( -11.12409513110480574, -16.64241105543193200, 18.63641924841378028 ) ) ;
#17683 = CARTESIAN_POINT ( 'NONE',  ( -70.00000000000000000, -70.00000000000000000, 12.49999999999999112 ) ) ;
#17684 = DIRECTION ( 'NONE',  ( 0.000000000000000000, -1.000000000000000000, 0.000000000000000000 ) ) ;
#17685 = DIRECTION ( 'NONE',  ( -1.000000000000000000, 0.000000000000000000, 0.000000000000000000 ) ) ;
#17686 = DIRECTION ( 'NONE',  ( 1.000000000000000000, 0.000000000000000000, 0.000000000000000000 ) ) ;
#17687 = CARTESIAN_POINT ( 'NONE',  ( -23.00100564131931691, 35.20929533517665533, -8.166629612147223938 ) ) ;
#17688 = EDGE_LOOP ( 'NONE', ( #22391, #13382, #7421, #10411 ) ) ;
#17689 = ORIENTED_EDGE ( 'NONE', *, *, #16033, .T. ) ;
#17690 =( BOUNDED_SURFACE ( )  B_SPLINE_SURFACE ( 3, 1, ( 
 ( #20111, #7640 ),
 ( #12487, #5760 ),
 ( #10279, #17468 ),
 ( #12325, #5296 ) ),
 .UNSPECIFIED., .F., .F., .T. ) 
 B_SPLINE_SURFACE_WITH_KNOTS ( ( 4, 4 ),
 ( 2, 2 ),
 ( 0.000000000000000000, 1.000000000000000000 ),
 ( 0.000000000000000000, 1.000000000000000000 ),
 .UNSPECIFIED. ) 
 GEOMETRIC_REPRESENTATION_ITEM ( )  RATIONAL_B_SPLINE_SURFACE ( (
 ( 1.000000000000000000, 1.000000000000000000),
 ( 0.8179194830933627092, 0.8179194830933627092),
 ( 0.8179194830933627092, 0.8179194830933627092),
 ( 1.000000000000000000, 1.000000000000000000) ) ) 
 REPRESENTATION_ITEM ( '' )  SURFACE ( )  );
#17691 = LINE ( 'NONE', #15502, #8937 ) ;
#17692 = AXIS2_PLACEMENT_3D ( 'NONE', #3947, #22950, #11113 ) ;
#17693 = CARTESIAN_POINT ( 'NONE',  ( -13.23566211985188623, 10.73140863935235068, 5.670038381137163519 ) ) ;
#17694 = DIRECTION ( 'NONE',  ( 0.2817325568414296710, -0.9594929736144973687, 0.000000000000000000 ) ) ;
#17695 = ORIENTED_EDGE ( 'NONE', *, *, #19859, .F. ) ;
#17696 = CARTESIAN_POINT ( 'NONE',  ( -23.07950435457407679, -11.50806656539752737, 44.96784366550136980 ) ) ;
#17697 = CARTESIAN_POINT ( 'NONE',  ( 20.65888525914375862, -38.75220717792901581, -19.50000000000000355 ) ) ;
#17698 = EDGE_LOOP ( 'NONE', ( #28882, #19147, #24057, #18065 ) ) ;
#17699 = DIRECTION ( 'NONE',  ( 0.6707505147970024284, 0.7416830501633134842, 0.000000000000000000 ) ) ;
#17700 = CARTESIAN_POINT ( 'NONE',  ( -2.209227181723746103, 8.499586724479465616, 21.50000000000000000 ) ) ;
#17701 = CARTESIAN_POINT ( 'NONE',  ( -37.14285906899156231, -13.21667505289354061, 31.69282016062263807 ) ) ;
#17702 = ORIENTED_EDGE ( 'NONE', *, *, #22687, .T. ) ;
#17703 = LINE ( 'NONE', #25033, #5892 ) ;
#17704 = FACE_OUTER_BOUND ( 'NONE', #14835, .T. ) ;
#17705 = DIRECTION ( 'NONE',  ( 0.000000000000000000, 0.000000000000000000, 1.000000000000000000 ) ) ;
#17706 = ORIENTED_EDGE ( 'NONE', *, *, #30525, .F. ) ;
#17707 = CARTESIAN_POINT ( 'NONE',  ( -15.17962487735951527, -7.751670534285734604, 5.651989602109218858 ) ) ;
#17708 = CIRCLE ( 'NONE', #15218, 27.70876437800068359 ) ;
#17709 = LINE ( 'NONE', #27399, #2404 ) ;
#17710 = CYLINDRICAL_SURFACE ( 'NONE', #3839, 7.500000000000013323 ) ;
#17711 = DIRECTION ( 'NONE',  ( 0.000000000000000000, 0.000000000000000000, 1.000000000000000000 ) ) ;
#17712 = CARTESIAN_POINT ( 'NONE',  ( -40.53232212831233028, -2.361325892396209714, -16.49999999999999645 ) ) ;
#17713 = LINE ( 'NONE', #29896, #27283 ) ;
#17714 = CARTESIAN_POINT ( 'NONE',  ( 11.40980092660686118, 6.310027164379057751, 1.500000000000001332 ) ) ;
#17715 = DIRECTION ( 'NONE',  ( -0.000000000000000000, -0.000000000000000000, 1.000000000000000000 ) ) ;
#17716 = ORIENTED_EDGE ( 'NONE', *, *, #18492, .T. ) ;
#17717 = DIRECTION ( 'NONE',  ( -1.000000000000000000, 0.000000000000000000, 0.000000000000000000 ) ) ;
#17718 = LINE ( 'NONE', #12283, #1135 ) ;
#17719=STYLED_ITEM('',(#30879),#3175);
#17720 = ORIENTED_EDGE ( 'NONE', *, *, #25240, .T. ) ;
#17721 = EDGE_LOOP ( 'NONE', ( #21009, #14189, #21632, #23378 ) ) ;
#17722 = CARTESIAN_POINT ( 'NONE',  ( -8.419710366748644148, 7.777014463793872956, 1.500000000000000000 ) ) ;
#17723 = CARTESIAN_POINT ( 'NONE',  ( -2.270234684139619041, 8.795879380940583303, 13.22130136205108997 ) ) ;
#17724 = DIRECTION ( 'NONE',  ( -1.000000000000000000, 0.000000000000000000, 0.000000000000000000 ) ) ;
#17725 = EDGE_LOOP ( 'NONE', ( #22952, #18753 ) ) ;
#17726 =( NAMED_UNIT ( * ) SI_UNIT ( $, .STERADIAN. ) SOLID_ANGLE_UNIT ( ) );
#17727 = DIRECTION ( 'NONE',  ( -0.7557495743542581579, -0.6548607339452852116, 0.000000000000000000 ) ) ;
#17728 = CARTESIAN_POINT ( 'NONE',  ( 12.40635649856745815, 11.68570839673119188, 18.34969686940296185 ) ) ;
#17729 = AXIS2_PLACEMENT_3D ( 'NONE', #16954, #24579, #719 ) ;
#17730 = EDGE_CURVE ( 'NONE', #11851, #11816, #2792, .T. ) ;
#17731 = EDGE_LOOP ( 'NONE', ( #18638, #22772, #8525 ) ) ;
#17732 = ORIENTED_EDGE ( 'NONE', *, *, #25909, .F. ) ;
#17733 = ADVANCED_FACE ( 'NONE', ( #10272 ), #19627, .F. ) ;
#17734 = LINE ( 'NONE', #6040, #19264 ) ;
#17735 = CARTESIAN_POINT ( 'NONE',  ( 6.631244434206235105, 6.812559277181991391, 1.500000000000001332 ) ) ;
#17736 = CIRCLE ( 'NONE', #2783, 7.500000000000000000 ) ;
#17737 = CARTESIAN_POINT ( 'NONE',  ( 40.35742903647388147, -4.708108710862773272, -16.50000000000000000 ) ) ;
#17738 = VERTEX_POINT ( 'NONE', #21974 ) ;
#17739 = CARTESIAN_POINT ( 'NONE',  ( -5.549075634136965363, 16.11684027513961226, 18.34798005863078885 ) ) ;
#17740 = EDGE_CURVE ( 'NONE', #20169, #7139, #19238, .T. ) ;
#17741 = CIRCLE ( 'NONE', #10254, 9.084132297865673777 ) ;
#17742 = VERTEX_POINT ( 'NONE', #5753 ) ;
#17743 = EDGE_CURVE ( 'NONE', #281, #10722, #20722, .T. ) ;
#17744 = CARTESIAN_POINT ( 'NONE',  ( -16.94861615806142296, 1.782241101945937212, 20.34789198813115618 ) ) ;
#17745 = AXIS2_PLACEMENT_3D ( 'NONE', #13997, #11806, #21000 ) ;
#17746 = ORIENTED_EDGE ( 'NONE', *, *, #5907, .T. ) ;
#17747 = B_SPLINE_CURVE_WITH_KNOTS ( 'NONE', 3,
 ( #828, #10351, #29684, #17053, #5671, #17371, #26585, #8021, #5209, #14710, #24217, #26895, #2867, #17523, #27044, #1300, #11126, #1908 ),
 .UNSPECIFIED., .F., .F.,
 ( 4, 2, 2, 2, 2, 2, 2, 2, 4 ),
 ( 0.000000000000000000, 0.1250000000000000000, 0.2500000000000000000, 0.3750000000000000000, 0.5000000000000000000, 0.6250000000000000000, 0.7500000000000000000, 0.8750000000000000000, 1.000000000000000000 ),
 .UNSPECIFIED. ) ;
#17748 = AXIS2_PLACEMENT_3D ( 'NONE', #22475, #10635, #13459 ) ;
#17749 = ADVANCED_FACE ( 'NONE', ( #7956 ), #19484, .T. ) ;
#17750 = CARTESIAN_POINT ( 'NONE',  ( 11.97149782862661027, -40.45422486509310289, 29.01997631939856959 ) ) ;
#17751 = CARTESIAN_POINT ( 'NONE',  ( 16.55532831589958320, 4.193940174973930013, 6.672349528511551497 ) ) ;
#17752 = FACE_OUTER_BOUND ( 'NONE', #25127, .T. ) ;
#17753 = EDGE_CURVE ( 'NONE', #26694, #8742, #15279, .T. ) ;
#17754 = CARTESIAN_POINT ( 'NONE',  ( -7.673856334772117371, -15.25703464229374084, 19.47783254395485031 ) ) ;
#17756 = EDGE_CURVE ( 'NONE', #12360, #18098, #28712, .T. ) ;
#17755 = CIRCLE ( 'NONE', #12286, 10.00000000000000000 ) ;
#17757 = CARTESIAN_POINT ( 'NONE',  ( -6.419316938171813369, 41.92620935963721962, 28.88939473975622718 ) ) ;
#17758 = CARTESIAN_POINT ( 'NONE',  ( -16.96555893289282935, 1.647560171710575228, 18.34798005862662507 ) ) ;
#17759 = LINE ( 'NONE', #27439, #7379 ) ;
#17761 = CARTESIAN_POINT ( 'NONE',  ( 11.29413195299407491, 40.68967926612123875, 21.21776214944138772 ) ) ;
#17760 = CIRCLE ( 'NONE', #4304, 9.084132297865673777 ) ;
#17762 = CARTESIAN_POINT ( 'NONE',  ( 11.71757112412214141, -16.22992597261981018, 18.64703902303423178 ) ) ;
#17763 = AXIS2_PLACEMENT_3D ( 'NONE', #666, #7850, #21565 ) ;
#17764 = CARTESIAN_POINT ( 'NONE',  ( -25.64627119138473788, 23.40052582045089480, -6.500000000000000888 ) ) ;
#17765 = ORIENTED_EDGE ( 'NONE', *, *, #26117, .F. ) ;
#17766 = ORIENTED_EDGE ( 'NONE', *, *, #10561, .T. ) ;
#17767 = CARTESIAN_POINT ( 'NONE',  ( 18.00031268893096481, -8.717656915646676552, 18.72886616302734097 ) ) ;
#17768 = CARTESIAN_POINT ( 'NONE',  ( 10.99809977392671279, -16.70505906359366932, 7.652108011868849147 ) ) ;
#17769 = FACE_OUTER_BOUND ( 'NONE', #9822, .T. ) ;
#17770 = ORIENTED_EDGE ( 'NONE', *, *, #20619, .T. ) ;
#17771 = B_SPLINE_CURVE_WITH_KNOTS ( 'NONE', 3,
 ( #29574, #20053, #10228, #17418, #3532, #27230, #27547, #24572, #5555, #13049, #13356, #29892, #6173, #26937, #15676, #5705 ),
 .UNSPECIFIED., .F., .F.,
 ( 4, 2, 2, 2, 2, 2, 2, 4 ),
 ( 2.980374332640320740E-07, 0.0009280375596593695665, 0.001391907320772415311, 0.001855777081885461163, 0.002319646842998507232, 0.002783516604111560457, 0.003247386365224614116, 0.003711256126337667341 ),
 .UNSPECIFIED. ) ;
#17772 = CARTESIAN_POINT ( 'NONE',  ( 0.000000000000000000, 0.000000000000000000, 21.50000000000000000 ) ) ;
#17773 = AXIS2_PLACEMENT_3D ( 'NONE', #3503, #22204, #17532 ) ;
#17774 = CARTESIAN_POINT ( 'NONE',  ( -70.00000000000000000, 70.00000000000000000, -92.50000000000000000 ) ) ;
#17775 = AXIS2_PLACEMENT_3D ( 'NONE', #30068, #4320, #13849 ) ;
#17776 = EDGE_CURVE ( 'NONE', #23138, #13113, #11205, .T. ) ;
#17777 = LINE ( 'NONE', #19800, #15405 ) ;
#17778 = B_SPLINE_CURVE_WITH_KNOTS ( 'NONE', 3,
 ( #16457, #18648, #13672, #20253, #23156, #9128, #25971, #16149, #30344, #4456, #21114, #20962, #1805, #30486, #4287, #14099 ),
 .UNSPECIFIED., .F., .F.,
 ( 4, 2, 2, 2, 2, 2, 2, 4 ),
 ( 0.5000000000000000000, 0.6250000000000008882, 0.6875000000000015543, 0.7187500000000019984, 0.7500000000000023315, 0.8125000000000014433, 0.8750000000000006661, 1.000000000000000000 ),
 .UNSPECIFIED. ) ;
#17779 = ORIENTED_EDGE ( 'NONE', *, *, #20077, .F. ) ;
#17780 = ADVANCED_FACE ( 'NONE', ( #6528 ), #3734, .F. ) ;
#17781 = EDGE_CURVE ( 'NONE', #8016, #14669, #19733, .T. ) ;
#17782 = CARTESIAN_POINT ( 'NONE',  ( 7.827050521741877098, -5.352643706120495004, 21.50000000000000000 ) ) ;
#17783 = VECTOR ( 'NONE', #11715, 1000.000000000000000 ) ;
#17784 = DIRECTION ( 'NONE',  ( 0.000000000000000000, -1.000000000000000000, 0.000000000000000000 ) ) ;
#17785 = EDGE_CURVE ( 'NONE', #6787, #2517, #1821, .T. ) ;
#17786 = CARTESIAN_POINT ( 'NONE',  ( 19.87213478643044340, 2.412525337365569733, 6.018569869498933578 ) ) ;
#17787 = ORIENTED_EDGE ( 'NONE', *, *, #10890, .F. ) ;
#17788 = CIRCLE ( 'NONE', #28240, 6.000000000000005329 ) ;
#17789 = CARTESIAN_POINT ( 'NONE',  ( -11.40980092660686829, 6.310027164379044429, 1.500000000000001332 ) ) ;
#17790 = EDGE_LOOP ( 'NONE', ( #27464, #25950 ) ) ;
#17791 = CARTESIAN_POINT ( 'NONE',  ( 19.18576292979354747, 22.55620591602726677, 24.50000000000000000 ) ) ;
#17792 = AXIS2_PLACEMENT_3D ( 'NONE', #14208, #11896, #31 ) ;
#17793 = ADVANCED_FACE ( 'NONE', ( #1239 ), #27334, .T. ) ;
#17794 = CARTESIAN_POINT ( 'NONE',  ( -40.00000000000002842, 80.00000000000001421, 52.50000000000014921 ) ) ;
#17795 = AXIS2_PLACEMENT_3D ( 'NONE', #2685, #7054, #16562 ) ;
#17796 = ORIENTED_EDGE ( 'NONE', *, *, #18426, .F. ) ;
#17797 = ORIENTED_EDGE ( 'NONE', *, *, #15441, .T. ) ;
#17798 = ADVANCED_FACE ( 'NONE', ( #2145 ), #30672, .F. ) ;
#17799 = ADVANCED_FACE ( 'NONE', ( #25702 ), #11978, .T. ) ;
#17800 = CARTESIAN_POINT ( 'NONE',  ( 4.469338653509386639, 19.51245501789046344, 7.196036389296800451 ) ) ;
#17801 = CARTESIAN_POINT ( 'NONE',  ( 0.000000000000000000, -2.775557561562891351E-14, 157.4999999999999716 ) ) ;
#17802 = CARTESIAN_POINT ( 'NONE',  ( -3.668292057955944596, 8.743977807160110416, 21.50000000000000000 ) ) ;
#17803 = AXIS2_PLACEMENT_3D ( 'NONE', #21393, #10017, #12047 ) ;
#17804 = CARTESIAN_POINT ( 'NONE',  ( -17.94248964168179938, 34.33858135081683827, 27.49999999999999645 ) ) ;
#17805 = CARTESIAN_POINT ( 'NONE',  ( 10.58525311124732049, -16.99040216561238026, 18.55820869691756769 ) ) ;
#17806 = CARTESIAN_POINT ( 'NONE',  ( 19.89475757678375345, 2.217009531549523960, 19.56050940960062690 ) ) ;
#17807 = VERTEX_POINT ( 'NONE', #28507 ) ;
#17808 = CARTESIAN_POINT ( 'NONE',  ( -5.815855718377446415, -16.25752007041490188, 1.500000000000000000 ) ) ;
#17809 = CARTESIAN_POINT ( 'NONE',  ( 18.26182835180409825, -8.199456719779957936, 5.670038381137163519 ) ) ;
#17810 = VECTOR ( 'NONE', #20880, 1000.000000000000114 ) ;
#17811 = CARTESIAN_POINT ( 'NONE',  ( -15.85879827683069010, 12.21494667905098019, 18.73743063545763121 ) ) ;
#17812 = CARTESIAN_POINT ( 'NONE',  ( 9.169883732660084164, -9.268939115642975679, 1.500000000000001332 ) ) ;
#17813 = CARTESIAN_POINT ( 'NONE',  ( 0.000000000000000000, 7.500000000000000000, -16.50000000000000000 ) ) ;
#17814 = VERTEX_POINT ( 'NONE', #4179 ) ;
#17815 = VECTOR ( 'NONE', #4589, 1000.000000000000114 ) ;
#17816 = CARTESIAN_POINT ( 'NONE',  ( 29.07478158690974013, -28.32671550006340055, 16.11782540859593382 ) ) ;
#17817 = CARTESIAN_POINT ( 'NONE',  ( 23.21352257770656990, 10.78826658734920230, 49.40206402021032517 ) ) ;
#17818 = EDGE_CURVE ( 'NONE', #28109, #22736, #21471, .T. ) ;
#17819 = CARTESIAN_POINT ( 'NONE',  ( -4.935065328765587012, 16.29835470421560828, 20.12545155307891065 ) ) ;
#17820 = CARTESIAN_POINT ( 'NONE',  ( 3.914781618004695041, 8.197313248159959542, 13.22130136205108997 ) ) ;
#17821 = EDGE_CURVE ( 'NONE', #15390, #8511, #2633, .T. ) ;
#17822 = DIRECTION ( 'NONE',  ( 0.000000000000000000, 0.000000000000000000, 1.000000000000000000 ) ) ;
#17823 = CYLINDRICAL_SURFACE ( 'NONE', #25342, 10.00000000000000000 ) ;
#17824 = CARTESIAN_POINT ( 'NONE',  ( 6.563702251502810725, 36.99658191090264125, 37.50000000022351543 ) ) ;
#17825 = AXIS2_PLACEMENT_3D ( 'NONE', #14596, #19431, #26927 ) ;
#17826 = ORIENTED_EDGE ( 'NONE', *, *, #22358, .T. ) ;
#17827 = LINE ( 'NONE', #24985, #13182 ) ;
#17828 = CIRCLE ( 'NONE', #13353, 6.000000000000001776 ) ;
#17829 = CARTESIAN_POINT ( 'NONE',  ( -33.37677408195396112, 9.488883682882484294, 40.30072466173501056 ) ) ;
#17830 = EDGE_CURVE ( 'NONE', #16844, #9112, #27202, .T. ) ;
#17831 = DIRECTION ( 'NONE',  ( 0.000000000000000000, 1.000000000000000000, 0.000000000000000000 ) ) ;
#17832 = VERTEX_POINT ( 'NONE', #15065 ) ;
#17833 = ORIENTED_EDGE ( 'NONE', *, *, #9993, .T. ) ;
#17834 = CARTESIAN_POINT ( 'NONE',  ( -19.75697076387333695, 3.109827004491390934, 7.454139397117727661 ) ) ;
#17835 = AXIS2_PLACEMENT_3D ( 'NONE', #25848, #4480, #25223 ) ;
#17836 = CARTESIAN_POINT ( 'NONE',  ( 2.168404344971008868E-16, 30.50000000000000000, 24.50000000000000000 ) ) ;
#17837 = ORIENTED_EDGE ( 'NONE', *, *, #2110, .F. ) ;
#17838 = CARTESIAN_POINT ( 'NONE',  ( 0.3541519782205858613, -20.01464289576667710, 18.34798005862930381 ) ) ;
#17839 = VECTOR ( 'NONE', #29719, 1000.000000000000000 ) ;
#17840 = FACE_OUTER_BOUND ( 'NONE', #11281, .T. ) ;
#17841 = FACE_OUTER_BOUND ( 'NONE', #22524, .T. ) ;
#17842 = DIRECTION ( 'NONE',  ( 1.000000000000000000, 0.000000000000000000, 0.000000000000000000 ) ) ;
#17843 = CARTESIAN_POINT ( 'NONE',  ( 19.91398265452213323, -1.852915226174633778, 24.50000000000000000 ) ) ;
#17844 = DIRECTION ( 'NONE',  ( 0.000000000000000000, 0.000000000000000000, -1.000000000000000000 ) ) ;
#17845 = CARTESIAN_POINT ( 'NONE',  ( 15.57266529552203416, -38.96488032230103471, 1.500000000000000000 ) ) ;
#17846 = CARTESIAN_POINT ( 'NONE',  ( 0.8008512464130215225, -20.00192252186466746, 5.749491821935610147 ) ) ;
#17847 = DIRECTION ( 'NONE',  ( 0.000000000000000000, 0.000000000000000000, 1.000000000000000000 ) ) ;
#17848 = AXIS2_PLACEMENT_3D ( 'NONE', #5297, #27136, #29158 ) ;
#17849 = ORIENTED_EDGE ( 'NONE', *, *, #25426, .F. ) ;
#17850 = VECTOR ( 'NONE', #2528, 1000.000000000000000 ) ;
#17851 = CARTESIAN_POINT ( 'NONE',  ( -9.223046300750477045, -14.31106556781055339, 19.96783386855779341 ) ) ;
#17852 = CARTESIAN_POINT ( 'NONE',  ( -15.13309390500917573, -7.848982836665745921, 7.652108011868850035 ) ) ;
#17853 = CARTESIAN_POINT ( 'NONE',  ( -5.549075634136967139, 16.11684027513961226, 5.652196082368482699 ) ) ;
#17854 = CARTESIAN_POINT ( 'NONE',  ( 11.94600218753717513, -16.06231219995581583, 6.672349528511551497 ) ) ;
#17855 = EDGE_CURVE ( 'NONE', #20591, #15313, #13752, .T. ) ;
#17856 = CARTESIAN_POINT ( 'NONE',  ( -20.65888525914099105, 38.75220717792564784, -19.50000000000000355 ) ) ;
#17857 = CARTESIAN_POINT ( 'NONE',  ( -32.68301789103641397, 8.668739453992939659, 36.94438844897151597 ) ) ;
#17858 = AXIS2_PLACEMENT_3D ( 'NONE', #26852, #5778, #12808 ) ;
#17859 = ORIENTED_EDGE ( 'NONE', *, *, #23506, .F. ) ;
#17860 = VERTEX_POINT ( 'NONE', #19599 ) ;
#17861 = DIRECTION ( 'NONE',  ( -1.000000000000000000, 0.000000000000000000, 0.000000000000000000 ) ) ;
#17862 = CARTESIAN_POINT ( 'NONE',  ( 0.000000000000000000, 44.39187623478217404, -19.50000000000000355 ) ) ;
#17863 = CARTESIAN_POINT ( 'NONE',  ( -14.88989150774294146, 13.37932992012220446, 5.940635272151477686 ) ) ;
#17864 = CARTESIAN_POINT ( 'NONE',  ( 0.000000000000000000, -2.435693370351110282E-15, 21.50000000000000355 ) ) ;
#17865 = ORIENTED_EDGE ( 'NONE', *, *, #1172, .T. ) ;
#17866 = PLANE ( 'NONE',  #2647 ) ;
#17867 = CARTESIAN_POINT ( 'NONE',  ( 2.552544031601107211, 42.49999999998228617, -1.500000000000000000 ) ) ;
#17868 = CARTESIAN_POINT ( 'NONE',  ( -11.05774036494469925, -16.68675304545164195, 5.862424720655265098 ) ) ;
#17869 = AXIS2_PLACEMENT_3D ( 'NONE', #28163, #20974, #11339 ) ;
#17870 = ORIENTED_EDGE ( 'NONE', *, *, #22020, .F. ) ;
#17871 = B_SPLINE_SURFACE_WITH_KNOTS ( 'NONE', 3, 1, ( 
 ( #10202, #13166 ),
 ( #29866, #17383 ),
 ( #22207, #25014 ),
 ( #20022, #27203 ),
 ( #685, #15028 ),
 ( #3652, #29234 ),
 ( #8508, #24869 ),
 ( #3036, #8180 ),
 ( #22507, #8030 ),
 ( #5525, #843 ),
 ( #3339, #13018 ),
 ( #22659, #27519 ),
 ( #10828, #1007 ),
 ( #1152, #24543 ),
 ( #8340, #20337 ),
 ( #17854, #10513 ),
 ( #3190, #26905 ),
 ( #12710, #22369 ),
 ( #18010, #14881 ),
 ( #10665, #27372 ),
 ( #10364, #17535 ),
 ( #5838, #15338 ),
 ( #5680, #5993 ),
 ( #15176, #24696 ),
 ( #12871, #29544 ),
 ( #20172, #1476 ),
 ( #15967, #13327 ),
 ( #2063, #8647 ),
 ( #3804, #30009 ),
 ( #20930, #9095 ),
 ( #11586, #18158 ) ),
 .UNSPECIFIED., .F., .F., .F.,
 ( 4, 3, 3, 3, 3, 3, 3, 3, 3, 3, 4 ),
 ( 2, 2 ),
 ( 0.4999999998345684982, 0.5360336730431942698, 0.5907651151589017324, 0.6456034593241839481, 0.6998270958050443191, 0.7529536536315944995, 0.8052385063053264513, 0.8575343587103996246, 0.9106564858195047574, 0.9648414833209688624, 1.000000006602610236 ),
 ( 0.000000000000000000, 1.000000000000000000 ),
 .UNSPECIFIED. ) ;
#17872 = VECTOR ( 'NONE', #8171, 1000.000000000000114 ) ;
#17873 = AXIS2_PLACEMENT_3D ( 'NONE', #23188, #18535, #28040 ) ;
#17874 = CARTESIAN_POINT ( 'NONE',  ( -50.00000000000000000, -70.00000000000000000, 59.49999999999999289 ) ) ;
#17875 = CARTESIAN_POINT ( 'NONE',  ( 19.58271949849003946, 4.064458250759533264, 19.85730954408918336 ) ) ;
#17876 = VERTEX_POINT ( 'NONE', #5259 ) ;
#17877 = CARTESIAN_POINT ( 'NONE',  ( 11.83211694375102496, -16.12463123479446381, 7.161525567826885208 ) ) ;
#17878 = DIRECTION ( 'NONE',  ( -0.000000000000000000, -1.000000000000000000, -0.000000000000000000 ) ) ;
#17879 = CARTESIAN_POINT ( 'NONE',  ( 32.14097302481091845, -14.40131566728160628, 39.78047203870804083 ) ) ;
#17880 = AXIS2_PLACEMENT_3D ( 'NONE', #390, #19421, #28940 ) ;
#17881 = CARTESIAN_POINT ( 'NONE',  ( -3.196529495465446402, -8.413215745754985875, 21.50000000000000000 ) ) ;
#17882 = ORIENTED_EDGE ( 'NONE', *, *, #8221, .T. ) ;
#17883 = CARTESIAN_POINT ( 'NONE',  ( 9.349584168494304848, 12.69858007495367680, -0.6213203435596476032 ) ) ;
#17884 = DIRECTION ( 'NONE',  ( 1.000000000000000000, 0.000000000000000000, 0.000000000000000000 ) ) ;
#17885 = PRESENTATION_STYLE_ASSIGNMENT (( #18034 ) ) ;
#17886 = DIRECTION ( 'NONE',  ( -0.000000000000000000, -0.000000000000000000, 1.000000000000000000 ) ) ;
#17887 = CARTESIAN_POINT ( 'NONE',  ( -17.06238204535203096, 0.6919203014629479176, 6.329955581934033404 ) ) ;
#17888 =( BOUNDED_CURVE ( )  B_SPLINE_CURVE ( 3, ( #2567, #18791, #213, #9726 ),
 .UNSPECIFIED., .F., .T. ) 
 B_SPLINE_CURVE_WITH_KNOTS ( ( 4, 4 ),
 ( 2.399144907686414196, 2.730840413552699353 ),
 .UNSPECIFIED. ) 
 CURVE ( )  GEOMETRIC_REPRESENTATION_ITEM ( )  RATIONAL_B_SPLINE_CURVE ( ( 1.000000000000000000, 0.9908525036704132205, 0.9908525036704132205, 1.000000000000000000 ) ) 
 REPRESENTATION_ITEM ( '' )  );
#17889 = DIRECTION ( 'NONE',  ( -0.5503133621338236470, -0.8349582046168341209, 0.000000000000000000 ) ) ;
#17890 = DIRECTION ( 'NONE',  ( 0.000000000000000000, 1.132880637372608986E-16, -1.000000000000000000 ) ) ;
#17891 = DIRECTION ( 'NONE',  ( -0.000000000000000000, 1.132880637372608986E-16, -1.000000000000000000 ) ) ;
#17892 = ORIENTED_EDGE ( 'NONE', *, *, #9763, .F. ) ;
#17893 = PRODUCT_DEFINITION_FORMATION_WITH_SPECIFIED_SOURCE ( 'ANY', '', #14916, .NOT_KNOWN. ) ;
#17894 = CARTESIAN_POINT ( 'NONE',  ( 0.8762659238204211221, 8.999114229549594057, 21.50000000000000000 ) ) ;
#17895 = CARTESIAN_POINT ( 'NONE',  ( 0.000000000000000000, 7.794228634059944483, -4.500000000000004441 ) ) ;
#17896 = ORIENTED_EDGE ( 'NONE', *, *, #5222, .T. ) ;
#17897 = AXIS2_PLACEMENT_3D ( 'NONE', #8547, #30203, #4006 ) ;
#17898 = ORIENTED_EDGE ( 'NONE', *, *, #28250, .T. ) ;
#17899 = DIRECTION ( 'NONE',  ( 0.000000000000000000, -0.000000000000000000, -1.000000000000000000 ) ) ;
#17900 = CARTESIAN_POINT ( 'NONE',  ( 35.76344986165623396, 22.29344514668041199, -19.50000000000000355 ) ) ;
#17901 = CARTESIAN_POINT ( 'NONE',  ( -7.856594496258223259, -4.390207617113929039, 21.50000000000000000 ) ) ;
#17902 = ORIENTED_EDGE ( 'NONE', *, *, #26350, .T. ) ;
#17903 = CARTESIAN_POINT ( 'NONE',  ( -40.00000000000002842, 90.00000000000001421, 22.49999999999983302 ) ) ;
#17904 = CARTESIAN_POINT ( 'NONE',  ( -8.072557715923444732, 14.41080185948837311, 24.50000000000000000 ) ) ;
#17905 = ORIENTED_EDGE ( 'NONE', *, *, #20232, .F. ) ;
#17906 = EDGE_LOOP ( 'NONE', ( #25562, #26599, #19153, #6833, #9966, #25437 ) ) ;
#17907 = CARTESIAN_POINT ( 'NONE',  ( -19.86072707285307359, 2.502642989097794590, 7.652108011868850035 ) ) ;
#17908 = EDGE_CURVE ( 'NONE', #27870, #16473, #8283, .T. ) ;
#17909 = AXIS2_PLACEMENT_3D ( 'NONE', #2691, #12201, #21701 ) ;
#17910 = CARTESIAN_POINT ( 'NONE',  ( 18.08053511453367790, -8.550039048713399481, 7.454139397117720556 ) ) ;
#17911 = CARTESIAN_POINT ( 'NONE',  ( 15.05429537369195359, 13.16750578773770464, 5.676722608126683944 ) ) ;
#17912 = DIRECTION ( 'NONE',  ( 1.000000000000000000, 0.000000000000000000, 0.000000000000000000 ) ) ;
#17913 = ORIENTED_EDGE ( 'NONE', *, *, #18066, .T. ) ;
#17914 = DIRECTION ( 'NONE',  ( -0.000000000000000000, -0.000000000000000000, 1.000000000000000000 ) ) ;
#17915 = ORIENTED_EDGE ( 'NONE', *, *, #15859, .F. ) ;
#17916 = CARTESIAN_POINT ( 'NONE',  ( -16.87834697510463045, 2.265528671608726619, 20.14907003336613300 ) ) ;
#17917 = ORIENTED_EDGE ( 'NONE', *, *, #15654, .F. ) ;
#17918 = LINE ( 'NONE', #15561, #4318 ) ;
#17919 = CARTESIAN_POINT ( 'NONE',  ( 37.27204780043465604, -12.57768201427415988, 31.72981289407691108 ) ) ;
#17920 = CARTESIAN_POINT ( 'NONE',  ( 19.72311808385369858, 3.421819763545496773, 5.678370764302467677 ) ) ;
#17921 = DIRECTION ( 'NONE',  ( -1.000000000000000000, 0.000000000000000000, -0.000000000000000000 ) ) ;
#17922 = AXIS2_PLACEMENT_3D ( 'NONE', #28519, #23822, #16963 ) ;
#17923 = CARTESIAN_POINT ( 'NONE',  ( -8.361245565923715262, -14.86101098545372956, 20.32367522806703874 ) ) ;
#17924 = EDGE_CURVE ( 'NONE', #11277, #26276, #29278, .T. ) ;
#17925 = CARTESIAN_POINT ( 'NONE',  ( 25.47847050916410439, -26.57182937991349903, 1.500000000000001332 ) ) ;
#17926 = CARTESIAN_POINT ( 'NONE',  ( -9.353104432029162751, -14.22246372587116348, 6.973843882838226094 ) ) ;
#17927 = FACE_BOUND ( 'NONE', #12378, .T. ) ;
#17928 = ORIENTED_EDGE ( 'NONE', *, *, #22726, .T. ) ;
#17929 = CARTESIAN_POINT ( 'NONE',  ( 2.703030265324084080, -12.75514121382991384, 24.50000000000000000 ) ) ;
#17930 = AXIS2_PLACEMENT_3D ( 'NONE', #11426, #25620, #30288 ) ;
#17931 = CARTESIAN_POINT ( 'NONE',  ( 10.46384303394385817, -13.48464439008897209, 18.64703902303423178 ) ) ;
#17932 = CARTESIAN_POINT ( 'NONE',  ( 27.03943647958860552, 26.20092231554394857, 27.49999999999999645 ) ) ;
#17933 = EDGE_CURVE ( 'NONE', #526, #6797, #21630, .T. ) ;
#17934 = VERTEX_POINT ( 'NONE', #4950 ) ;
#17935 = EDGE_LOOP ( 'NONE', ( #26077, #21056, #1743, #7789, #9236, #23814 ) ) ;
#17936 = DIRECTION ( 'NONE',  ( 1.000000000000000000, 0.000000000000000000, 0.000000000000000000 ) ) ;
#17937 = DIRECTION ( 'NONE',  ( -0.000000000000000000, -0.000000000000000000, 1.000000000000000000 ) ) ;
#17938 = EDGE_CURVE ( 'NONE', #194, #2397, #9781, .T. ) ;
#17939 = CARTESIAN_POINT ( 'NONE',  ( -5.023839636758347105, 19.37724795171757464, 6.420335371522007506 ) ) ;
#17940 = EDGE_LOOP ( 'NONE', ( #10133, #17358, #6359, #22718 ) ) ;
#17941 = CARTESIAN_POINT ( 'NONE',  ( 8.884323311075775109, 1.438332125858202692, 21.50000000000000000 ) ) ;
#17942 = CARTESIAN_POINT ( 'NONE',  ( -3.196529495465446402, -8.413215745754985875, -1.500000000000002665 ) ) ;
#17943 = CARTESIAN_POINT ( 'NONE',  ( 23.07601128794333434, 11.40611796340042261, 49.25937209212059997 ) ) ;
#17944 = EDGE_LOOP ( 'NONE', ( #19960, #9386, #19975, #25202, #13525, #12748, #6320, #9116 ) ) ;
#17945 = CARTESIAN_POINT ( 'NONE',  ( 52.16608720827707657, -36.86186943028246787, 97.07879600563551037 ) ) ;
#17946 = CIRCLE ( 'NONE', #26919, 1.447898107987198646 ) ;
#17947 = CARTESIAN_POINT ( 'NONE',  ( 11.69519594420021313, 12.44297266173655458, 6.341840715582230281 ) ) ;
#17948 = CARTESIAN_POINT ( 'NONE',  ( 16.79398274391852652, 2.865066961627992903, 5.701226463332907279 ) ) ;
#17949 = EDGE_LOOP ( 'NONE', ( #26480, #13535, #2494, #18783 ) ) ;
#17950 = ADVANCED_FACE ( 'NONE', ( #12595 ), #5419, .F. ) ;
#17951 = CARTESIAN_POINT ( 'NONE',  ( 12.35522127274689730, 11.74279147932066181, 5.652196082367002106 ) ) ;
#17952 = ORIENTED_EDGE ( 'NONE', *, *, #29989, .F. ) ;
#17953 = CARTESIAN_POINT ( 'NONE',  ( -14.01107592578418881, 9.765138712360661444, 19.47952243369110192 ) ) ;
#17954 = VERTEX_POINT ( 'NONE', #7451 ) ;
#17955 = ORIENTED_EDGE ( 'NONE', *, *, #19143, .T. ) ;
#17956 = LINE ( 'NONE', #13441, #3629 ) ;
#17957 = DIRECTION ( 'NONE',  ( -0.9898214418809326842, 0.1423148382732851158, -0.000000000000000000 ) ) ;
#17958 = ORIENTED_EDGE ( 'NONE', *, *, #19493, .T. ) ;
#17959 = CARTESIAN_POINT ( 'NONE',  ( -17.94248964168179938, -34.33858135081683827, 34.80090346875805096 ) ) ;
#17960 = CARTESIAN_POINT ( 'NONE',  ( -40.00000000000002842, 80.00000000000001421, 52.50000000000014921 ) ) ;
#17961 = DIRECTION ( 'NONE',  ( 0.000000000000000000, 0.000000000000000000, 1.000000000000000000 ) ) ;
#17962 = ADVANCED_FACE ( 'NONE', ( #12745 ), #24281, .F. ) ;
#17963 = VERTEX_POINT ( 'NONE', #2611 ) ;
#17964 = ADVANCED_FACE ( 'NONE', ( #14924 ), #9270, .T. ) ;
#17965 = CARTESIAN_POINT ( 'NONE',  ( -19.72513283648485682, 3.411576116177901241, 19.77662771831109367 ) ) ;
#17966 = CARTESIAN_POINT ( 'NONE',  ( 18.30707599941031916, -8.097116190180054573, 5.657991946698900598 ) ) ;
#17967 = VECTOR ( 'NONE', #25715, 1000.000000000000000 ) ;
#17968 = CARTESIAN_POINT ( 'NONE',  ( -14.00200865723717314, 9.777219707070196719, 19.14333282897057842 ) ) ;
#17969 = CARTESIAN_POINT ( 'NONE',  ( 4.782940318440150662, 19.43789448792816543, 20.19593175699879595 ) ) ;
#17970 = ORIENTED_EDGE ( 'NONE', *, *, #5564, .F. ) ;
#17971 = EDGE_LOOP ( 'NONE', ( #8276, #11916, #29489, #1811 ) ) ;
#17972 = DIRECTION ( 'NONE',  ( 1.000000000000000000, 0.000000000000000000, 0.000000000000000000 ) ) ;
#17973 = EDGE_CURVE ( 'NONE', #19924, #11902, #28211, .T. ) ;
#17974 = CARTESIAN_POINT ( 'NONE',  ( -5.976020107417634009, 19.08630880174946043, 5.652196082369965069 ) ) ;
#17975 = ADVANCED_FACE ( 'NONE', ( #10406, #7600, #21786 ), #5569, .T. ) ;
#17976 = CARTESIAN_POINT ( 'NONE',  ( -5.754904482333549787, 19.17304367822655209, 20.32842677360128292 ) ) ;
#17977 = DIRECTION ( 'NONE',  ( -0.000000000000000000, -0.000000000000000000, -1.000000000000000000 ) ) ;
#17978 = CARTESIAN_POINT ( 'NONE',  ( 25.10445388623454477, 25.60065097860747585, 1.500000000000000000 ) ) ;
#17979 = EDGE_CURVE ( 'NONE', #20736, #11391, #13298, .T. ) ;
#17980 = DIRECTION ( 'NONE',  ( 0.000000000000000000, 0.000000000000000000, 1.000000000000000000 ) ) ;
#17981 = CARTESIAN_POINT ( 'NONE',  ( 16.85582347139597914, 2.398957759888394214, 6.031926333436654630 ) ) ;
#17982 = ADVANCED_FACE ( 'NONE', ( #16801 ), #23964, .F. ) ;
#17983 = ORIENTED_EDGE ( 'NONE', *, *, #17361, .F. ) ;
#17984 = FACE_OUTER_BOUND ( 'NONE', #23179, .T. ) ;
#17985 = DIRECTION ( 'NONE',  ( -0.000000000000000000, 0.000000000000000000, 1.000000000000000000 ) ) ;
#17986 = CARTESIAN_POINT ( 'NONE',  ( 33.78553873773097393, 24.40792641592722134, -16.50000000000000000 ) ) ;
#17987 = ORIENTED_EDGE ( 'NONE', *, *, #18187, .T. ) ;
#17988 = EDGE_CURVE ( 'NONE', #17047, #15766, #1330, .T. ) ;
#17989 = ORIENTED_EDGE ( 'NONE', *, *, #21561, .F. ) ;
#17990 = CARTESIAN_POINT ( 'NONE',  ( -19.77456323383487913, 2.996942905618070530, 5.775318986477955718 ) ) ;
#17991 = UNCERTAINTY_MEASURE_WITH_UNIT (LENGTH_MEASURE( 1.000000000000000082E-05 ), #21477, 'distance_accuracy_value', 'NONE');
#17992 = VECTOR ( 'NONE', #26979, 1000.000000000000000 ) ;
#17993 = DIRECTION ( 'NONE',  ( 1.000000000000000000, 0.000000000000000000, 0.000000000000000000 ) ) ;
#17994 = ORIENTED_EDGE ( 'NONE', *, *, #19172, .F. ) ;
#17995 = CARTESIAN_POINT ( 'NONE',  ( -0.5282983270408738719, -19.99308596983832231, 6.144783687052519205 ) ) ;
#17996 = CARTESIAN_POINT ( 'NONE',  ( 14.61451073016445967, 47.81658942982300431, -51.58549908343919554 ) ) ;
#17997 = CARTESIAN_POINT ( 'NONE',  ( -18.23283297759883581, -37.58012701748170059, 23.78652270266532653 ) ) ;
#17998 = CARTESIAN_POINT ( 'NONE',  ( -20.64946329957944116, -25.40401715649331749, -16.50001200000000168 ) ) ;
#17999 = CARTESIAN_POINT ( 'NONE',  ( -6.123826420728668118, 19.05819691457235976, 18.35718225375110180 ) ) ;
#18000 = CARTESIAN_POINT ( 'NONE',  ( -40.00000000000002842, 90.00000000000001421, 52.50000000000014921 ) ) ;
#18001 = FACE_OUTER_BOUND ( 'NONE', #29871, .T. ) ;
#18002 = LINE ( 'NONE', #30145, #29685 ) ;
#18003 = DIRECTION ( 'NONE',  ( 0.000000000000000000, 1.000000000000000000, 0.000000000000000000 ) ) ;
#18004 = ADVANCED_FACE ( 'NONE', ( #5105 ), #5875, .T. ) ;
#18005 = ORIENTED_EDGE ( 'NONE', *, *, #11521, .T. ) ;
#18006 = EDGE_CURVE ( 'NONE', #22947, #18116, #19382, .T. ) ;
#18007 = CARTESIAN_POINT ( 'NONE',  ( -9.147715168420964105, -14.36154699054606887, 18.63641924841378028 ) ) ;
#18008 = CARTESIAN_POINT ( 'NONE',  ( -15.06839649859471564, -7.981447355247934361, 7.627891251804737927 ) ) ;
#18009 = CARTESIAN_POINT ( 'NONE',  ( -5.861334694664001255, 16.01657976118488236, 7.603368798681074736 ) ) ;
#18010 = CARTESIAN_POINT ( 'NONE',  ( 11.89619695863782312, -16.09924856797056592, 6.995624166085161910 ) ) ;
#18011 = CARTESIAN_POINT ( 'NONE',  ( 49.99999999999997868, 90.00000000000001421, -34.50000000000000000 ) ) ;
#18012 = VECTOR ( 'NONE', #15099, 1000.000000000000000 ) ;
#18013 = CARTESIAN_POINT ( 'NONE',  ( -33.25379661643704310, 9.265521131796548460, 36.23697955560132300 ) ) ;
#18014 = ORIENTED_EDGE ( 'NONE', *, *, #4558, .T. ) ;
#18015 = VERTEX_POINT ( 'NONE', #20064 ) ;
#18016 = CARTESIAN_POINT ( 'NONE',  ( -4.163336342344337027E-14, -1.387778780781445676E-14, -1.500000000000000000 ) ) ;
#18017 = CARTESIAN_POINT ( 'NONE',  ( -13.38159811102998198, 10.55828946469181417, 5.652196082367002106 ) ) ;
#18018 = DIRECTION ( 'NONE',  ( 0.000000000000000000, -1.000000000000000000, -1.132880637372608986E-16 ) ) ;
#18019 = ORIENTED_EDGE ( 'NONE', *, *, #5567, .F. ) ;
#18020 = CARTESIAN_POINT ( 'NONE',  ( 0.000000000000000000, 0.000000000000000000, 1.500000000000001332 ) ) ;
#18021 = DIRECTION ( 'NONE',  ( 1.000000000000000000, 0.000000000000000000, 0.000000000000000000 ) ) ;
#18022 = CARTESIAN_POINT ( 'NONE',  ( -9.213835811784830909, -14.31736145455815645, 6.018569869498933578 ) ) ;
#18023 = ORIENTED_EDGE ( 'NONE', *, *, #8754, .T. ) ;
#18024 = DIRECTION ( 'NONE',  ( -1.000000000000000000, -0.000000000000000000, 0.000000000000000000 ) ) ;
#18025 = CARTESIAN_POINT ( 'NONE',  ( -20.23374174526511027, -31.57860962931301785, 37.50000000001161027 ) ) ;
#18026 = EDGE_LOOP ( 'NONE', ( #8839, #14059, #28527, #13233 ) ) ;
#18027 = CARTESIAN_POINT ( 'NONE',  ( -32.24119420145671455, 26.76047160551536663, -16.50000600000000262 ) ) ;
#18028 = ADVANCED_FACE ( 'NONE', ( #3843 ), #24736, .F. ) ;
#18029 = EDGE_CURVE ( 'NONE', #4388, #8400, #8071, .T. ) ;
#18030 = CIRCLE ( 'NONE', #21479, 0.7500000000000002220 ) ;
#18031 = CARTESIAN_POINT ( 'NONE',  ( 33.56327786402390245, 10.34181101807379299, 35.63689980405264635 ) ) ;
#18032 = EDGE_LOOP ( 'NONE', ( #22975, #6196, #23744, #27995 ) ) ;
#18033 = CARTESIAN_POINT ( 'NONE',  ( 15.57266529552203416, 38.96488032230103471, 1.500000000000000000 ) ) ;
#18034 = SURFACE_STYLE_USAGE ( .BOTH. , #29724 ) ;
#18035 = CARTESIAN_POINT ( 'NONE',  ( -43.01137460125430323, 68.74210893030173963, 12.95891939259967529 ) ) ;
#18036 = DIRECTION ( 'NONE',  ( -0.000000000000000000, 0.000000000000000000, 1.000000000000000000 ) ) ;
#18037 = CARTESIAN_POINT ( 'NONE',  ( -4.163336342344337027E-14, 1.387778780781445676E-14, 67.49999999999997158 ) ) ;
#18038 = DIRECTION ( 'NONE',  ( -0.000000000000000000, -0.000000000000000000, 1.000000000000000000 ) ) ;
#18039 = CARTESIAN_POINT ( 'NONE',  ( -37.99999999999999289, 70.00000000000000000, -87.50000000000000000 ) ) ;
#18040 = CARTESIAN_POINT ( 'NONE',  ( 25.64627119138473432, 23.40052582045089480, -6.500000000000000888 ) ) ;
#18041 = CARTESIAN_POINT ( 'NONE',  ( 33.48316501811950019, -9.771059948263134842, 40.12037505765862733 ) ) ;
#18042 = CARTESIAN_POINT ( 'NONE',  ( -7.075845757273814415E-16, 80.00000000000000000, 15.49999999999998757 ) ) ;
#18043 = ORIENTED_EDGE ( 'NONE', *, *, #2031, .T. ) ;
#18044 = VERTEX_POINT ( 'NONE', #25199 ) ;
#18045 = LINE ( 'NONE', #15688, #14445 ) ;
#18046 = CARTESIAN_POINT ( 'NONE',  ( 2.687479362164894248, -44.39187623478217404, -19.50000000000000355 ) ) ;
#18047 = DIRECTION ( 'NONE',  ( 0.000000000000000000, 0.000000000000000000, 1.000000000000000000 ) ) ;
#18048 = ORIENTED_EDGE ( 'NONE', *, *, #590, .F. ) ;
#18049 = VECTOR ( 'NONE', #16482, 1000.000000000000000 ) ;
#18050 = CARTESIAN_POINT ( 'NONE',  ( -6.385759811041538114, 15.83451745216639672, 18.84329447212442687 ) ) ;
#18051 = DIRECTION ( 'NONE',  ( -0.000000000000000000, -0.000000000000000000, -1.000000000000000000 ) ) ;
#18052 = EDGE_LOOP ( 'NONE', ( #21171, #30710, #2939 ) ) ;
#18053 = ORIENTED_EDGE ( 'NONE', *, *, #29078, .F. ) ;
#18054 = CARTESIAN_POINT ( 'NONE',  ( -16.86382086101523825, 2.355052171780695147, 5.940635272151477686 ) ) ;
#18055 = CARTESIAN_POINT ( 'NONE',  ( 8.795879380940565540, 2.270234684139708303, 21.50000000000000000 ) ) ;
#18056 = CARTESIAN_POINT ( 'NONE',  ( 7.856594496258195726, 4.390207617113981442, 1.500000000000001332 ) ) ;
#18057 = CARTESIAN_POINT ( 'NONE',  ( 4.216636297896264374, 37.26217892624189432, 37.50000000000000000 ) ) ;
#18058 = ORIENTED_EDGE ( 'NONE', *, *, #28805, .F. ) ;
#18059 = CARTESIAN_POINT ( 'NONE',  ( -4.574230723432976653, 16.39514892286269188, 19.21496526180054332 ) ) ;
#18060 = ORIENTED_EDGE ( 'NONE', *, *, #29510, .F. ) ;
#18061 = VECTOR ( 'NONE', #10556, 1000.000000000000000 ) ;
#18062 = CARTESIAN_POINT ( 'NONE',  ( 8.817355867515813017, 2.185336383880231992, 21.50000000000000000 ) ) ;
#18063 = FACE_OUTER_BOUND ( 'NONE', #9221, .T. ) ;
#18064 = EDGE_CURVE ( 'NONE', #15359, #5466, #10293, .T. ) ;
#18065 = ORIENTED_EDGE ( 'NONE', *, *, #10385, .T. ) ;
#18066 = EDGE_CURVE ( 'NONE', #11919, #15501, #29225, .T. ) ;
#18067 =( LENGTH_UNIT ( ) NAMED_UNIT ( * ) SI_UNIT ( .MILLI., .METRE. ) );
#18068 = CARTESIAN_POINT ( 'NONE',  ( -9.406652940105978189, 1.195154792889487227, 13.00000000000000178 ) ) ;
#18069 = CARTESIAN_POINT ( 'NONE',  ( 19.74834695364560133, 3.274018421667482137, 5.652605728828373977 ) ) ;
#18070 = DIRECTION ( 'NONE',  ( 0.000000000000000000, 0.000000000000000000, 1.000000000000000000 ) ) ;
#18071 = CARTESIAN_POINT ( 'NONE',  ( 1.664698296075797890, -16.99226504953965389, 7.158811349119584833 ) ) ;
#18072 = LINE ( 'NONE', #3883, #28480 ) ;
#18073 = CARTESIAN_POINT ( 'NONE',  ( -8.770223337696748445, -14.60814232176959671, 5.676815824193227833 ) ) ;
#18074 = PLANE ( 'NONE',  #13860 ) ;
#18075 = EDGE_LOOP ( 'NONE', ( #3366, #16102, #9719, #3018 ) ) ;
#18076 = CARTESIAN_POINT ( 'NONE',  ( 9.864935476092961508, -13.90063640548120460, 18.34798005862662507 ) ) ;
#18077 = CARTESIAN_POINT ( 'NONE',  ( 21.86019681245147339, 31.48592878035296749, 34.80090346875810070 ) ) ;
#18078 = ORIENTED_EDGE ( 'NONE', *, *, #20998, .T. ) ;
#18079 = ORIENTED_EDGE ( 'NONE', *, *, #39, .F. ) ;
#18080 = DIRECTION ( 'NONE',  ( 0.000000000000000000, -0.000000000000000000, -1.000000000000000000 ) ) ;
#18081 = VECTOR ( 'NONE', #9254, 1000.000000000000000 ) ;
#18082 = CIRCLE ( 'NONE', #30508, 0.7500000000000006661 ) ;
#18083 = CARTESIAN_POINT ( 'NONE',  ( 11.11118388262826251, -16.62953976291647962, 5.652196082369964181 ) ) ;
#18084 = CIRCLE ( 'NONE', #27055, 12.50000000000000000 ) ;
#18085 = CARTESIAN_POINT ( 'NONE',  ( -5.332709978455699051, 16.18357461815305243, 5.670038381137163519 ) ) ;
#18086 = VERTEX_POINT ( 'NONE', #8216 ) ;
#18087 = DIRECTION ( 'NONE',  ( 1.000000000000000000, 0.000000000000000000, 0.000000000000000000 ) ) ;
#18088 = CARTESIAN_POINT ( 'NONE',  ( -27.86235613436986114, 14.72519157938688750, 43.48653168448687012 ) ) ;
#18089 = CARTESIAN_POINT ( 'NONE',  ( 23.11610519334012537, 11.09643357455199464, 49.35895363836304028 ) ) ;
#18090 = VERTEX_POINT ( 'NONE', #22697 ) ;
#18091 = CARTESIAN_POINT ( 'NONE',  ( -1.687027447297492211, -8.840471615930066918, 21.50000000000000000 ) ) ;
#18092 = PLANE ( 'NONE',  #2249 ) ;
#18093 = CARTESIAN_POINT ( 'NONE',  ( -33.52437897089259877, -10.76376600292166863, 39.79035104387400423 ) ) ;
#18094 = ORIENTED_EDGE ( 'NONE', *, *, #1521, .F. ) ;
#18095 = DIRECTION ( 'NONE',  ( 0.000000000000000000, -1.132880637372608986E-16, 1.000000000000000000 ) ) ;
#18096 = ORIENTED_EDGE ( 'NONE', *, *, #23178, .F. ) ;
#18097 = ORIENTED_EDGE ( 'NONE', *, *, #14003, .F. ) ;
#18098 = VERTEX_POINT ( 'NONE', #8683 ) ;
#18099 = AXIS2_PLACEMENT_3D ( 'NONE', #3329, #12859, #22360 ) ;
#18100 = CARTESIAN_POINT ( 'NONE',  ( 3.060137030613569120, 16.80197902060525195, 6.560937769032974209 ) ) ;
#18101 = EDGE_CURVE ( 'NONE', #7391, #23685, #1349, .T. ) ;
#18102 = CIRCLE ( 'NONE', #28561, 9.482273699623480212 ) ;
#18103 = DIRECTION ( 'NONE',  ( 0.000000000000000000, 0.000000000000000000, 1.000000000000000000 ) ) ;
#18104 = CARTESIAN_POINT ( 'NONE',  ( 6.067212148875117173, 19.05774739413747909, 18.72886616302736229 ) ) ;
#18105 = ORIENTED_EDGE ( 'NONE', *, *, #26149, .T. ) ;
#18106 = B_SPLINE_CURVE_WITH_KNOTS ( 'NONE', 3,
 ( #21764, #2749, #12576, #10533, #27070, #15191, #22224, #12259 ),
 .UNSPECIFIED., .F., .F.,
 ( 4, 2, 2, 4 ),
 ( 0.005257893453559912313, 0.006567392922673243386, 0.007876892391786575326, 0.01049589133001323574 ),
 .UNSPECIFIED. ) ;
#18107 = CARTESIAN_POINT ( 'NONE',  ( -9.268856789657290207, -38.25380398711768493, 27.50000000000000355 ) ) ;
#18108 = CARTESIAN_POINT ( 'NONE',  ( 9.769531821641352920, -13.96399651007160081, 18.35377592296120497 ) ) ;
#18109 = CARTESIAN_POINT ( 'NONE',  ( 16.87995935610570442, 2.188012981718272076, 19.33715507985239412 ) ) ;
#18110 = ORIENTED_EDGE ( 'NONE', *, *, #13569, .F. ) ;
#18111 = CARTESIAN_POINT ( 'NONE',  ( -16.95074943597165174, 1.765291926024246116, 20.34789198813115263 ) ) ;
#18112 = LINE ( 'NONE', #13450, #3803 ) ;
#18113 = CARTESIAN_POINT ( 'NONE',  ( -15.81542570303654749, 12.27127866024200920, 5.951255046771932733 ) ) ;
#18114 = CARTESIAN_POINT ( 'NONE',  ( 4.877030535751917029, 19.41475911700131363, 20.25542030744407640 ) ) ;
#18115 = VERTEX_POINT ( 'NONE', #17894 ) ;
#18116 = VERTEX_POINT ( 'NONE', #27408 ) ;
#18117 = DIRECTION ( 'NONE',  ( 1.000000000000000000, 0.000000000000000000, 0.000000000000000000 ) ) ;
#18118 = DIRECTION ( 'NONE',  ( -0.000000000000000000, -0.000000000000000000, 1.000000000000000000 ) ) ;
#18119 = CARTESIAN_POINT ( 'NONE',  ( 15.52007383991469069, 12.61466978257045035, 19.08232364404839387 ) ) ;
#18120 = B_SPLINE_SURFACE_WITH_KNOTS ( 'NONE', 3, 1, ( 
 ( #27476, #22009 ),
 ( #8294, #3293 ),
 ( #20139, #12823 ),
 ( #19831, #22165 ),
 ( #24352, #7995 ),
 ( #17498, #644 ),
 ( #3609, #27167 ),
 ( #22324, #964 ),
 ( #29355, #2999 ),
 ( #17811, #13130 ),
 ( #15141, #6097 ),
 ( #29657, #22624 ),
 ( #10159, #27325 ),
 ( #12671, #17968 ),
 ( #8465, #27018 ),
 ( #10474, #19987 ),
 ( #5646, #5954 ),
 ( #19666, #26867 ),
 ( #29506, #1274 ),
 ( #3460, #10782 ),
 ( #8143, #5793 ),
 ( #15291, #24821 ),
 ( #12976, #15453 ),
 ( #29823, #7826 ),
 ( #22467, #20297 ),
 ( #17337, #5490 ),
 ( #14991, #15932 ),
 ( #21042, #11238 ),
 ( #28081, #13286 ),
 ( #16218, #6703 ),
 ( #11095, #30564 ) ),
 .UNSPECIFIED., .F., .F., .F.,
 ( 4, 3, 3, 3, 3, 3, 3, 3, 3, 3, 4 ),
 ( 2, 2 ),
 ( 0.4999999998345683316, 0.5360336730431939367, 0.5907651151589012883, 0.6456034593241830599, 0.6998270958050434309, 0.7529536536315937223, 0.8052385063053260073, 0.8575343587103997356, 0.9106564858195042023, 0.9648414833209685293, 1.000000006602610014 ),
 ( 0.000000000000000000, 1.000000000000000000 ),
 .UNSPECIFIED. ) ;
#18121 = CARTESIAN_POINT ( 'NONE',  ( -5.119216485953539397, 16.24645747311529931, 20.25336174263950184 ) ) ;
#18122 = CARTESIAN_POINT ( 'NONE',  ( 32.50000000000000000, 3.980102097228898626E-15, -52.50000000000000000 ) ) ;
#18123 = CIRCLE ( 'NONE', #26074, 20.00000000000000000 ) ;
#18124 = DIRECTION ( 'NONE',  ( -0.000000000000000000, -0.000000000000000000, 1.000000000000000000 ) ) ;
#18125 = CARTESIAN_POINT ( 'NONE',  ( -10.33689618797787446, 37.84157881464940942, 27.50000000000000355 ) ) ;
#18126 = VECTOR ( 'NONE', #15252, 1000.000000000000000 ) ;
#18127 = CARTESIAN_POINT ( 'NONE',  ( -24.44496207165490276, -7.595930209050158588, -16.55003854064094426 ) ) ;
#18128 = CIRCLE ( 'NONE', #25537, 4.999999999999997335 ) ;
#18129 = ORIENTED_EDGE ( 'NONE', *, *, #16972, .F. ) ;
#18130 = EDGE_CURVE ( 'NONE', #165, #28122, #24960, .T. ) ;
#18131 = CYLINDRICAL_SURFACE ( 'NONE', #12674, 0.7441270634457337607 ) ;
#18132 = CARTESIAN_POINT ( 'NONE',  ( -32.28307784207223108, 8.475829241206282560, 41.62281023987520001 ) ) ;
#18133 = DIRECTION ( 'NONE',  ( -0.4154150130018840481, 0.9096319953545194403, 0.000000000000000000 ) ) ;
#18134 = VERTEX_POINT ( 'NONE', #20521 ) ;
#18135 = EDGE_CURVE ( 'NONE', #30732, #5139, #5715, .T. ) ;
#18136 = ORIENTED_EDGE ( 'NONE', *, *, #30147, .F. ) ;
#18137 = FACE_OUTER_BOUND ( 'NONE', #15506, .T. ) ;
#18138 = FACE_OUTER_BOUND ( 'NONE', #14657, .T. ) ;
#18139 = VERTEX_POINT ( 'NONE', #26726 ) ;
#18140 = DIRECTION ( 'NONE',  ( -1.000000000000000000, -0.000000000000000000, -0.000000000000000000 ) ) ;
#18141 = EDGE_CURVE ( 'NONE', #3185, #7581, #30533, .T. ) ;
#18142 = CARTESIAN_POINT ( 'NONE',  ( -70.00000000000000000, -65.00000000000000000, 12.49999999999999112 ) ) ;
#18143 = EDGE_CURVE ( 'NONE', #15984, #22640, #24213, .T. ) ;
#18144 = CARTESIAN_POINT ( 'NONE',  ( -1.246245039005656974, 2.728895986063601509, 24.50000000000000000 ) ) ;
#18145 = CARTESIAN_POINT ( 'NONE',  ( -20.78475560873934569, -25.06838084537526612, -16.50001200000000523 ) ) ;
#18146 = FACE_OUTER_BOUND ( 'NONE', #3721, .T. ) ;
#18147 = CIRCLE ( 'NONE', #28092, 7.500000000000000000 ) ;
#18148 = CARTESIAN_POINT ( 'NONE',  ( 22.95669091611928181, 27.54300778121952575, 1.500000000000000000 ) ) ;
#18149 = CARTESIAN_POINT ( 'NONE',  ( 0.7788148826605760799, -17.02744010918315709, 7.652108011868850035 ) ) ;
#18150 = DIRECTION ( 'NONE',  ( -0.000000000000000000, -0.000000000000000000, 1.000000000000000000 ) ) ;
#18151 = EDGE_CURVE ( 'NONE', #13747, #16188, #9293, .T. ) ;
#18152 = ORIENTED_EDGE ( 'NONE', *, *, #18538, .F. ) ;
#18153 = EDGE_CURVE ( 'NONE', #315, #23230, #5667, .T. ) ;
#18154 = CARTESIAN_POINT ( 'NONE',  ( 9.824744466605370263, -8.513189541288715745, 24.50000000000000000 ) ) ;
#18155 = DIRECTION ( 'NONE',  ( -0.3598999890241659783, 0.9329908884337537733, 0.000000000000000000 ) ) ;
#18156 = CARTESIAN_POINT ( 'NONE',  ( 1.000000000000008438, 13.00000000000001421, 1.500000000000001332 ) ) ;
#18157 = EDGE_CURVE ( 'NONE', #4887, #2392, #3174, .T. ) ;
#18158 = CARTESIAN_POINT ( 'NONE',  ( 9.860909911264741368, -13.90333503211347477, 7.652108011868850035 ) ) ;
#18159 = CARTESIAN_POINT ( 'NONE',  ( 0.000000000000000000, 44.39187623478217404, -19.50000000000000355 ) ) ;
#18160 = CARTESIAN_POINT ( 'NONE',  ( 0.000000000000000000, -5.590849009245238754, -1.500000000000000000 ) ) ;
#18161 = ORIENTED_EDGE ( 'NONE', *, *, #251, .T. ) ;
#18162 = CARTESIAN_POINT ( 'NONE',  ( -50.00000000000000000, 90.00000000000001421, 52.49999999999999289 ) ) ;
#18163 = CARTESIAN_POINT ( 'NONE',  ( -20.65888525914099105, 38.75220717792564784, -19.50000000000000355 ) ) ;
#18164 = CARTESIAN_POINT ( 'NONE',  ( 35.03831055084558699, -13.42466405557608944, 37.50000000000372324 ) ) ;
#18165 = LINE ( 'NONE', #15974, #6607 ) ;
#18166 = EDGE_LOOP ( 'NONE', ( #21165, #16640, #5258, #14406 ) ) ;
#18167 = B_SPLINE_CURVE_WITH_KNOTS ( 'NONE', 3,
 ( #30826, #20852, #27735, #1987, #6366, #18528, #28031, #6809, #9158, #18672, #18834, #28179, #16337, #4484, #26003, #13994, #21141, #30660, #9308, #28351 ),
 .UNSPECIFIED., .F., .F.,
 ( 4, 2, 2, 2, 2, 2, 2, 2, 2, 4 ),
 ( 0.000000000000000000, 0.06250000000000183187, 0.1250000000000036637, 0.1875000000000054956, 0.2187500000000056344, 0.2500000000000057732, 0.3125000000000043299, 0.3750000000000028866, 0.4375000000000014433, 0.5000000000000000000 ),
 .UNSPECIFIED. ) ;
#18168 = CYLINDRICAL_SURFACE ( 'NONE', #10426, 9.482273699623480212 ) ;
#18169 = CARTESIAN_POINT ( 'NONE',  ( 10.64374042650304020, -42.96126232887725394, -19.50000000000000355 ) ) ;
#18170 = CARTESIAN_POINT ( 'NONE',  ( -9.376411575904491258, -14.20642299464377345, 6.864725433338323413 ) ) ;
#18171 = VECTOR ( 'NONE', #13425, 1000.000000000000114 ) ;
#18172 = ADVANCED_FACE ( 'NONE', ( #12543 ), #14266, .F. ) ;
#18173 = ORIENTED_EDGE ( 'NONE', *, *, #16447, .T. ) ;
#18174 = EDGE_CURVE ( 'NONE', #24299, #8908, #22250, .T. ) ;
#18175 = CARTESIAN_POINT ( 'NONE',  ( -23.12263228470262888, -11.97179573940914921, 48.96234658225964864 ) ) ;
#18176 = EDGE_CURVE ( 'NONE', #2982, #11117, #24691, .T. ) ;
#18177 = CARTESIAN_POINT ( 'NONE',  ( 0.000000000000000000, 1.699320956058915452E-16, -1.500000000000001776 ) ) ;
#18178 = VERTEX_POINT ( 'NONE', #5205 ) ;
#18179 = CARTESIAN_POINT ( 'NONE',  ( -31.61046531718546149, 26.43913157134711156, -9.833326303388901124 ) ) ;
#18180 = EDGE_CURVE ( 'NONE', #13938, #24446, #14706, .T. ) ;
#18181 = CARTESIAN_POINT ( 'NONE',  ( 3.763133143576435913, -8.268028093133381162, -1.500000000000002665 ) ) ;
#18182 = CARTESIAN_POINT ( 'NONE',  ( 7.488956955540398752, 5.141690706682901180, 13.22130136205108819 ) ) ;
#18183 = ORIENTED_EDGE ( 'NONE', *, *, #12059, .T. ) ;
#18184 = DIRECTION ( 'NONE',  ( -1.000000000000000000, -0.000000000000000000, -0.000000000000000000 ) ) ;
#18185 = CARTESIAN_POINT ( 'NONE',  ( 0.000000000000000000, 0.000000000000000000, -87.50000000000000000 ) ) ;
#18186 = DIRECTION ( 'NONE',  ( 1.000000000000000000, 0.000000000000000000, -0.000000000000000000 ) ) ;
#18187 = EDGE_CURVE ( 'NONE', #23990, #8702, #27191, .T. ) ;
#18188 = CARTESIAN_POINT ( 'NONE',  ( 26.41394434536444535, -32.09691347256665495, -6.500000000000000000 ) ) ;
#18189 = DIRECTION ( 'NONE',  ( 1.000000000000000000, 0.000000000000000000, 0.000000000000000000 ) ) ;
#18190 = CIRCLE ( 'NONE', #10699, 1.447898107987198646 ) ;
#18191 = DIRECTION ( 'NONE',  ( 1.000000000000000000, 0.000000000000000000, 0.000000000000000000 ) ) ;
#18192 = PLANE ( 'NONE',  #24834 ) ;
#18193 = CARTESIAN_POINT ( 'NONE',  ( 9.181265710901294952, -14.33790826719505773, 7.267659094423557065 ) ) ;
#18194 = CARTESIAN_POINT ( 'NONE',  ( 0.07661102881318006264, 8.673996836102553232, -2.976196775178694853 ) ) ;
#18195 = ORIENTED_EDGE ( 'NONE', *, *, #3500, .T. ) ;
#18196 = ORIENTED_EDGE ( 'NONE', *, *, #8031, .T. ) ;
#18197 = DIRECTION ( 'NONE',  ( 1.000000000000000000, 0.000000000000000000, 0.000000000000000000 ) ) ;
#18198 = CARTESIAN_POINT ( 'NONE',  ( 25.19442432474404470, 35.44676296256560022, -19.50000000000000355 ) ) ;
#18199 = ADVANCED_FACE ( 'NONE', ( #22959 ), #8492, .F. ) ;
#18200 = LINE ( 'NONE', #4465, #26853 ) ;
#18201 = ORIENTED_EDGE ( 'NONE', *, *, #28308, .T. ) ;
#18202 = EDGE_CURVE ( 'NONE', #228, #25790, #29995, .T. ) ;
#18203 = CARTESIAN_POINT ( 'NONE',  ( 23.22298176981586337, -35.92225146852586448, -14.83329738391580221 ) ) ;
#18204 = DIRECTION ( 'NONE',  ( 0.000000000000000000, 0.000000000000000000, -1.000000000000000000 ) ) ;
#18205 = EDGE_LOOP ( 'NONE', ( #22835, #7418 ) ) ;
#18206 = ORIENTED_EDGE ( 'NONE', *, *, #21784, .T. ) ;
#18207 = CARTESIAN_POINT ( 'NONE',  ( -19.75958569938476117, 3.205325445645398563, 5.940635272151477686 ) ) ;
#18208 = CARTESIAN_POINT ( 'NONE',  ( -30.50204315964898427, -15.53056155674291183, 36.52918211141458471 ) ) ;
#18209 = CARTESIAN_POINT ( 'NONE',  ( 14.88222593340885958, 13.36111339922579155, 7.652108011868850035 ) ) ;
#18210 = FACE_OUTER_BOUND ( 'NONE', #21486, .T. ) ;
#18211 = ORIENTED_EDGE ( 'NONE', *, *, #21582, .T. ) ;
#18212 = LINE ( 'NONE', #8854, #2391 ) ;
#18213 = CIRCLE ( 'NONE', #30159, 0.7500000000000006661 ) ;
#18214 = ORIENTED_EDGE ( 'NONE', *, *, #5526, .F. ) ;
#18215 = CARTESIAN_POINT ( 'NONE',  ( 5.881244434206234217, 6.812559277181991391, 1.500000000000001332 ) ) ;
#18216 = DIRECTION ( 'NONE',  ( 0.000000000000000000, 0.000000000000000000, 1.000000000000000000 ) ) ;
#18217 = ORIENTED_EDGE ( 'NONE', *, *, #8221, .F. ) ;
#18218 = CARTESIAN_POINT ( 'NONE',  ( -3.912171961292012057, -8.637616862297827325, 13.00000000000000178 ) ) ;
#18219 = CARTESIAN_POINT ( 'NONE',  ( 17.26937953831880534, -14.36006998371588317, 1.500000000000000000 ) ) ;
#18220 = DIRECTION ( 'NONE',  ( 0.9547931052914336858, 0.2972711322815274615, -0.000000000000000000 ) ) ;
#18221 = CARTESIAN_POINT ( 'NONE',  ( -6.224883619896829146, -5.687793815610328707, 21.50000000000000000 ) ) ;
#18222 = AXIS2_PLACEMENT_3D ( 'NONE', #24536, #15328, #3183 ) ;
#18223 = CARTESIAN_POINT ( 'NONE',  ( 0.7836604620899301210, -17.02735026737548552, 5.652196082368483587 ) ) ;
#18224 = CARTESIAN_POINT ( 'NONE',  ( 0.000000000000000000, 0.000000000000000000, 21.50000000000000000 ) ) ;
#18225 = DIRECTION ( 'NONE',  ( -0.7557495743542581579, -0.6548607339452852116, 0.000000000000000000 ) ) ;
#18226 = CYLINDRICAL_SURFACE ( 'NONE', #17372, 20.00000000000000000 ) ;
#18227 = ORIENTED_EDGE ( 'NONE', *, *, #19668, .T. ) ;
#18228 = CARTESIAN_POINT ( 'NONE',  ( -29.54217267045739348, 27.74668781839406506, 16.62675390102625528 ) ) ;
#18229 = CARTESIAN_POINT ( 'NONE',  ( -4.375757216953428294E-15, -39.50000000000000000, 27.50000000000000355 ) ) ;
#18230 = ORIENTED_EDGE ( 'NONE', *, *, #22307, .F. ) ;
#18231 = ORIENTED_EDGE ( 'NONE', *, *, #2926, .F. ) ;
#18232 = AXIS2_PLACEMENT_3D ( 'NONE', #14386, #5960, #27022 ) ;
#18233 = CARTESIAN_POINT ( 'NONE',  ( 48.60441976126723773, 69.95499445371133618, 17.35986660046888019 ) ) ;
#18234 = CARTESIAN_POINT ( 'NONE',  ( -0.1262659238204836554, -8.999114229549588728, -3.621320343559650379 ) ) ;
#18235 = CARTESIAN_POINT ( 'NONE',  ( 33.01877980957530667, -12.12572312222180670, 35.60092001944722995 ) ) ;
#18236 = ORIENTED_EDGE ( 'NONE', *, *, #11504, .T. ) ;
#18237 = CARTESIAN_POINT ( 'NONE',  ( -4.163336342344337027E-14, 1.387778780781445676E-14, 24.50000000000000000 ) ) ;
#18238 = VECTOR ( 'NONE', #25421, 1000.000000000000000 ) ;
#18239 = DIRECTION ( 'NONE',  ( 1.000000000000000000, 0.000000000000000000, 0.000000000000000000 ) ) ;
#18240 = EDGE_CURVE ( 'NONE', #24029, #6719, #26733, .T. ) ;
#18241 = CARTESIAN_POINT ( 'NONE',  ( 31.56327786402390245, -10.34181101807379655, -16.55003854064094426 ) ) ;
#18242 = EDGE_LOOP ( 'NONE', ( #21712, #6429, #6620, #1810 ) ) ;
#18243 = DIRECTION ( 'NONE',  ( 0.000000000000000000, -1.132880637372608986E-16, 1.000000000000000000 ) ) ;
#18244 = CARTESIAN_POINT ( 'NONE',  ( 0.000000000000000000, -7.028748154183644736, -16.50000000000000000 ) ) ;
#18245 = ORIENTED_EDGE ( 'NONE', *, *, #16472, .T. ) ;
#18246 = DIRECTION ( 'NONE',  ( 1.000000000000000000, 0.000000000000000000, 0.000000000000000000 ) ) ;
#18247 = ORIENTED_EDGE ( 'NONE', *, *, #20232, .T. ) ;
#18248 = DIRECTION ( 'NONE',  ( -0.000000000000000000, 0.000000000000000000, 1.000000000000000000 ) ) ;
#18249 = PRODUCT_DEFINITION_CONTEXT ( 'detailed design', #10394, 'design' ) ;
#18250 = ORIENTED_EDGE ( 'NONE', *, *, #18947, .T. ) ;
#18251 = ORIENTED_EDGE ( 'NONE', *, *, #15844, .T. ) ;
#18252 = VECTOR ( 'NONE', #25282, 1000.000000000000000 ) ;
#18253 = CARTESIAN_POINT ( 'NONE',  ( 4.877030535751920581, 19.41475911700131363, 7.559636331181775581 ) ) ;
#18254 = CIRCLE ( 'NONE', #11286, 9.482273699623480212 ) ;
#18255 = DIRECTION ( 'NONE',  ( 1.000000000000000000, 0.000000000000000000, 0.000000000000000000 ) ) ;
#18256 = LINE ( 'NONE', #20288, #28260 ) ;
#18257 = ORIENTED_EDGE ( 'NONE', *, *, #24597, .T. ) ;
#18258 = VECTOR ( 'NONE', #582, 1000.000000000000000 ) ;
#18259 = CARTESIAN_POINT ( 'NONE',  ( -32.31576317091163730, 17.59561277345963504, 27.50000000000000355 ) ) ;
#18260 = DIRECTION ( 'NONE',  ( 0.000000000000000000, 1.000000000000000000, 0.000000000000000000 ) ) ;
#18261 = FACE_OUTER_BOUND ( 'NONE', #2888, .T. ) ;
#18262 = ORIENTED_EDGE ( 'NONE', *, *, #9947, .F. ) ;
#18263 = CARTESIAN_POINT ( 'NONE',  ( 0.000000000000000000, 12.18947652193946851, 27.94260272410217638 ) ) ;
#18264 = CARTESIAN_POINT ( 'NONE',  ( 15.72291199960845454, -6.567794255929247704, 5.670038381137163519 ) ) ;
#18265 = DIRECTION ( 'NONE',  ( 0.000000000000000000, 0.000000000000000000, 1.000000000000000000 ) ) ;
#18266 = CARTESIAN_POINT ( 'NONE',  ( 4.772488686130579083, 19.44046140540703504, 18.50655187082627862 ) ) ;
#18267 = ORIENTED_EDGE ( 'NONE', *, *, #17580, .F. ) ;
#18268 = EDGE_LOOP ( 'NONE', ( #14697, #26018, #9704, #30787 ) ) ;
#18269 = CARTESIAN_POINT ( 'NONE',  ( 4.510281037539698445E-13, -4.926614671774132148E-13, 77.49999999999998579 ) ) ;
#18270 = VECTOR ( 'NONE', #19211, 1000.000000000000000 ) ;
#18271 = DIRECTION ( 'NONE',  ( -0.000000000000000000, -0.000000000000000000, 1.000000000000000000 ) ) ;
#18272 = CARTESIAN_POINT ( 'NONE',  ( 19.64177907938615064, -36.71644397333972876, 24.50000000000000000 ) ) ;
#18273 = CARTESIAN_POINT ( 'NONE',  ( -32.28307784207223108, -8.475829241206275455, 41.62281023987519291 ) ) ;
#18274 = DIRECTION ( 'NONE',  ( 0.000000000000000000, 1.000000000000000000, 0.000000000000000000 ) ) ;
#18275 = CARTESIAN_POINT ( 'NONE',  ( -6.974883619896829146, -5.687793815610328707, 21.50000000000000000 ) ) ;
#18276 = VECTOR ( 'NONE', #24853, 1000.000000000000000 ) ;
#18277 = CARTESIAN_POINT ( 'NONE',  ( -18.65094025732183525, 33.78913767902538012, 27.50000000000000355 ) ) ;
#18278 = AXIS2_PLACEMENT_3D ( 'NONE', #11020, #10555, #29584 ) ;
#18279 = CONTEXT_DEPENDENT_SHAPE_REPRESENTATION ( #16171, #3215 ) ;
#18280 = CARTESIAN_POINT ( 'NONE',  ( 2.878478920843542177, 0.8451976705242683074, 24.50000000000000000 ) ) ;
#18281 = VERTEX_POINT ( 'NONE', #11123 ) ;
#18282 = CIRCLE ( 'NONE', #12807, 21.71568325578193637 ) ;
#18283 = CARTESIAN_POINT ( 'NONE',  ( 0.3567147238643512130, -19.99681861211370659, 5.652196082369963293 ) ) ;
#18284 = FACE_OUTER_BOUND ( 'NONE', #9805, .T. ) ;
#18285 = CARTESIAN_POINT ( 'NONE',  ( 22.58267429318970443, -26.57182937991349903, 1.500000000000001332 ) ) ;
#18286 = ORIENTED_EDGE ( 'NONE', *, *, #9245, .F. ) ;
#18287 = CARTESIAN_POINT ( 'NONE',  ( 4.119120293826439294, 16.53802619141619346, 18.34969686940295830 ) ) ;
#18288 = ORIENTED_EDGE ( 'NONE', *, *, #1029, .T. ) ;
#18289 = CARTESIAN_POINT ( 'NONE',  ( -19.71415773217920986, 3.369653345580889692, 7.156831654632820339 ) ) ;
#18290 = CARTESIAN_POINT ( 'NONE',  ( -30.53339558441486190, -7.800891647352838909, 39.24389099736757913 ) ) ;
#18291 = AXIS2_PLACEMENT_3D ( 'NONE', #9092, #8643, #27827 ) ;
#18292 = ORIENTED_EDGE ( 'NONE', *, *, #16452, .F. ) ;
#18293 = CARTESIAN_POINT ( 'NONE',  ( 9.041888939645136958, -0.8750451464062836138, 21.50000000000000000 ) ) ;
#18294 = DIRECTION ( 'NONE',  ( 0.8349582046168341209, 0.5503133621338236470, 0.000000000000000000 ) ) ;
#18295 = CARTESIAN_POINT ( 'NONE',  ( -22.94541271838176755, -35.03073867844241818, -6.500000000000000888 ) ) ;
#18296 = CARTESIAN_POINT ( 'NONE',  ( -8.499586724479453181, -2.959227181723774525, -3.621320343559650379 ) ) ;
#18297 = AXIS2_PLACEMENT_3D ( 'NONE', #782, #24811, #29499 ) ;
#18298 = DIRECTION ( 'NONE',  ( -0.000000000000000000, 0.000000000000000000, 1.000000000000000000 ) ) ;
#18299 = CIRCLE ( 'NONE', #17285, 0.7499999999999997780 ) ;
#18300 = CARTESIAN_POINT ( 'NONE',  ( 52.16608720827707657, 36.86186943028246787, 97.07879600563551037 ) ) ;
#18301 = CARTESIAN_POINT ( 'NONE',  ( 1.653546806191835250, -16.99301016096993422, 6.131018562779544823 ) ) ;
#18302 = CARTESIAN_POINT ( 'NONE',  ( -16.94912694330537306, 1.778434104809240912, 5.651492010659113774 ) ) ;
#18303 = ORIENTED_EDGE ( 'NONE', *, *, #11135, .T. ) ;
#18304 = AXIS2_PLACEMENT_3D ( 'NONE', #10392, #15363, #1187 ) ;
#18305 = DIRECTION ( 'NONE',  ( 0.9594929736144952592, -0.2817325568414371095, 0.000000000000000000 ) ) ;
#18306 = FACE_OUTER_BOUND ( 'NONE', #26621, .T. ) ;
#18307 = ADVANCED_FACE ( 'NONE', ( #17840 ), #8630, .F. ) ;
#18308 = CARTESIAN_POINT ( 'NONE',  ( -4.773373620198770872, 16.34284820692472451, 6.031926333436658183 ) ) ;
#18309 = CARTESIAN_POINT ( 'NONE',  ( 6.511989298491061007E-15, -8.236864015571844888, 3.733333029993807006 ) ) ;
#18310 = CIRCLE ( 'NONE', #7837, 1.447898107987198646 ) ;
#18311 = PRODUCT_DEFINITION ( 'UNKNOWN', '', #28330, #12344 ) ;
#18312 = CARTESIAN_POINT ( 'NONE',  ( 0.000000000000000000, 7.794228634059939154, 4.500000000000010658 ) ) ;
#18313 = VECTOR ( 'NONE', #4205, 1000.000000000000000 ) ;
#18314 = DIRECTION ( 'NONE',  ( 1.000000000000000000, 0.000000000000000000, 0.000000000000000000 ) ) ;
#18315 = CIRCLE ( 'NONE', #15284, 22.49999999999996447 ) ;
#18316 = EDGE_CURVE ( 'NONE', #13370, #2118, #831, .T. ) ;
#18317 = EDGE_LOOP ( 'NONE', ( #300, #19299, #8282, #24901 ) ) ;
#18318 = CARTESIAN_POINT ( 'NONE',  ( -0.6312581325461337212, -19.99009984789270433, 19.60917204426171168 ) ) ;
#18319 = CARTESIAN_POINT ( 'NONE',  ( 2.552544030762014415, -42.50000000000000000, -1.500000000000000000 ) ) ;
#18320 = CARTESIAN_POINT ( 'NONE',  ( 36.92711665837346402, -13.73927826681822317, 34.88776314540329082 ) ) ;
#18321 = CLOSED_SHELL ( 'NONE', ( #1340, #26700, #18866, #7476, #22175, #9189, #11060, #14137, #8633, #17733, #17060, #9026, #22352, #27536, #19355, #13407, #16418, #16961, #29764, #7679, #9193, #15153, #6533, #20769, #9219, #16336, #3134, #30111, #3124, #9349, #1154, #480, #4395, #28489, #9163, #3841, #2100, #26804, #15439, #21173, #2745, #17799, #29752, #19929, #5391, #19122, #62, #2275, #14515, #27517, #13944, #15482, #11940, #10353, #12107, #1766, #15491, #5028, #1091, #28272 ) ) ;
#18322 = ADVANCED_FACE ( 'NONE', ( #4096 ), #15634, .F. ) ;
#18323 = DIRECTION ( 'NONE',  ( 0.000000000000000000, 0.000000000000000000, 1.000000000000000000 ) ) ;
#18324 = EDGE_LOOP ( 'NONE', ( #12420, #21618, #26887 ) ) ;
#18325 = DIRECTION ( 'NONE',  ( 0.2972711322815266843, -0.9547931052914337968, -0.000000000000000000 ) ) ;
#18326 = AXIS2_PLACEMENT_3D ( 'NONE', #7032, #25465, #4090 ) ;
#18327 = CARTESIAN_POINT ( 'NONE',  ( -40.89187623478217404, -5.790488632116337797, -19.50000000000000355 ) ) ;
#18328 = DIRECTION ( 'NONE',  ( 0.000000000000000000, 0.000000000000000000, -1.000000000000000000 ) ) ;
#18329 = CIRCLE ( 'NONE', #12331, 0.7500000000000015543 ) ;
#18330 = ORIENTED_EDGE ( 'NONE', *, *, #3242, .F. ) ;
#18331 = AXIS2_PLACEMENT_3D ( 'NONE', #20013, #675, #10504 ) ;
#18332 = EDGE_CURVE ( 'NONE', #10292, #21897, #15412, .T. ) ;
#18333 = DIRECTION ( 'NONE',  ( -0.000000000000000000, 0.000000000000000000, 1.000000000000000000 ) ) ;
#18334 = EDGE_LOOP ( 'NONE', ( #17632, #28995, #10932, #12178 ) ) ;
#18335 = DIRECTION ( 'NONE',  ( 0.000000000000000000, 1.000000000000000000, 0.000000000000000000 ) ) ;
#18336 = EDGE_CURVE ( 'NONE', #8546, #9249, #20246, .T. ) ;
#18337 = AXIS2_PLACEMENT_3D ( 'NONE', #15664, #25029, #6007 ) ;
#18338 = CARTESIAN_POINT ( 'NONE',  ( 0.000000000000000000, 0.000000000000000000, 1.500000000000001332 ) ) ;
#18339 = AXIS2_PLACEMENT_3D ( 'NONE', #1914, #23569, #1625 ) ;
#18340 = CARTESIAN_POINT ( 'NONE',  ( -14.83584055149731817, -17.84153987719691514, 1.500000000000000000 ) ) ;
#18341 = AXIS2_PLACEMENT_3D ( 'NONE', #5710, #26788, #12904 ) ;
#18342 = ORIENTED_EDGE ( 'NONE', *, *, #5764, .F. ) ;
#18343 = CARTESIAN_POINT ( 'NONE',  ( 23.11610519334012537, 11.09643357455199464, 45.11631295124375640 ) ) ;
#18344 = CARTESIAN_POINT ( 'NONE',  ( 16.55667234708964486, 4.187688857956195498, 6.521906765011494578 ) ) ;
#18345 = DIRECTION ( 'NONE',  ( -0.8412535328311804284, 0.5406408174555987767, 0.000000000000000000 ) ) ;
#18346 = CARTESIAN_POINT ( 'NONE',  ( 27.75715622479469147, -6.315477654728063328E-15, 24.50000000000000000 ) ) ;
#18347 = AXIS2_PLACEMENT_3D ( 'NONE', #7228, #28607, #16908 ) ;
#18348 = DIRECTION ( 'NONE',  ( 0.000000000000000000, 0.000000000000000000, 1.000000000000000000 ) ) ;
#18349 = CARTESIAN_POINT ( 'NONE',  ( 0.000000000000000000, 0.000000000000000000, -87.50000000000000000 ) ) ;
#18350 = CARTESIAN_POINT ( 'NONE',  ( 1.750000000000008660, 16.48749217771910125, 1.500000000000000000 ) ) ;
#18351 = ADVANCED_FACE ( 'NONE', ( #18907, #28261 ), #3759, .F. ) ;
#18352 = EDGE_CURVE ( 'NONE', #10409, #20585, #7040, .T. ) ;
#18353 = DIRECTION ( 'NONE',  ( 0.8412535328311810945, 0.5406408174555976665, 0.000000000000000000 ) ) ;
#18354 = CARTESIAN_POINT ( 'NONE',  ( 0.8038475772933696417, 10.39230484541327471, -1.336447385876663028E-16 ) ) ;
#18355 = EDGE_LOOP ( 'NONE', ( #18780, #9484, #11009, #2555 ) ) ;
#18356 = EDGE_CURVE ( 'NONE', #13536, #24159, #1905, .T. ) ;
#18357 = EDGE_LOOP ( 'NONE', ( #24723, #8083, #16528, #15126 ) ) ;
#18358 = CARTESIAN_POINT ( 'NONE',  ( -14.44122519041009234, -13.83658248990211348, 24.50000000000000000 ) ) ;
#18359 = DIRECTION ( 'NONE',  ( 1.000000000000000000, 0.000000000000000000, 0.000000000000000000 ) ) ;
#18360 = VECTOR ( 'NONE', #5761, 1000.000000000000000 ) ;
#18361 = LINE ( 'NONE', #16467, #28340 ) ;
#18362 = EDGE_CURVE ( 'NONE', #20591, #27348, #20919, .T. ) ;
#18363 = VERTEX_POINT ( 'NONE', #9083 ) ;
#18364 = DIRECTION ( 'NONE',  ( 0.000000000000000000, 0.000000000000000000, -1.000000000000000000 ) ) ;
#18365 = AXIS2_PLACEMENT_3D ( 'NONE', #26261, #23921, #21260 ) ;
#18366 = DIRECTION ( 'NONE',  ( 0.000000000000000000, 0.000000000000000000, -1.000000000000000000 ) ) ;
#18367 = VECTOR ( 'NONE', #14954, 1000.000000000000000 ) ;
#18368 = DIRECTION ( 'NONE',  ( 0.000000000000000000, 0.000000000000000000, 1.000000000000000000 ) ) ;
#18369 = EDGE_CURVE ( 'NONE', #6009, #3753, #20606, .T. ) ;
#18370 = EDGE_CURVE ( 'NONE', #1375, #28044, #23237, .T. ) ;
#18371 = VERTEX_POINT ( 'NONE', #4396 ) ;
#18372 = CARTESIAN_POINT ( 'NONE',  ( -19.86132377132435778, 2.497833445081380166, 5.652196082367002106 ) ) ;
#18373 = AXIS2_PLACEMENT_3D ( 'NONE', #1138, #27353, #5510 ) ;
#18374 = CARTESIAN_POINT ( 'NONE',  ( 15.21452331804151115, 12.98203751624682667, 5.775318986477954830 ) ) ;
#18375 = PLANE ( 'NONE',  #7519 ) ;
#18376 = ORIENTED_EDGE ( 'NONE', *, *, #17461, .T. ) ;
#18377 =( REPRESENTATION_RELATIONSHIP ('NONE','NONE', #19885, #23229 ) REPRESENTATION_RELATIONSHIP_WITH_TRANSFORMATION ( #23238 )SHAPE_REPRESENTATION_RELATIONSHIP( ) );
#18378 = LINE ( 'NONE', #27727, #27811 ) ;
#18379 = ORIENTED_EDGE ( 'NONE', *, *, #7257, .T. ) ;
#18380 = B_SPLINE_CURVE_WITH_KNOTS ( 'NONE', 3,
 ( #25188, #3834, #22853, #1504, #11012, #20513, #8676, #18955, #21429, #25964, #19406, #21580, #26109, #2244, #14571, #19096, #12230, #28924 ),
 .UNSPECIFIED., .F., .F.,
 ( 4, 2, 2, 2, 2, 2, 2, 2, 4 ),
 ( 0.000000000000000000, 0.0003967869494442878304, 0.0007935738988885756608, 0.001190360848332863491, 0.001587147797777151322, 0.001983934747221438935, 0.002380721696665726982, 0.002777508646110015030, 0.003174295595554302643 ),
 .UNSPECIFIED. ) ;
#18381 = DIRECTION ( 'NONE',  ( 1.000000000000000000, 0.000000000000000000, 0.000000000000000000 ) ) ;
#18382 = CARTESIAN_POINT ( 'NONE',  ( -15.34618562042307310, 12.82554431217321245, 5.652196082369965069 ) ) ;
#18383 = ORIENTED_EDGE ( 'NONE', *, *, #24612, .F. ) ;
#18384 = CARTESIAN_POINT ( 'NONE',  ( -0.1262659238204836554, -8.999114229549588728, -3.621320343559650379 ) ) ;
#18385 = CARTESIAN_POINT ( 'NONE',  ( 26.12047388987419083, -6.311255530320352136, 43.88527982295130414 ) ) ;
#18386 = AXIS2_PLACEMENT_3D ( 'NONE', #14112, #6959, #27876 ) ;
#18387 = EDGE_CURVE ( 'NONE', #4045, #27870, #30589, .T. ) ;
#18388 = LINE ( 'NONE', #15020, #29542 ) ;
#18389 = B_SPLINE_SURFACE_WITH_KNOTS ( 'NONE', 3, 1, ( 
 ( #6291, #27829 ),
 ( #15803, #6602 ),
 ( #16116, #11444 ),
 ( #30307, #25325 ),
 ( #11137, #6458 ),
 ( #4109, #30601 ),
 ( #4252, #28124 ),
 ( #3968, #13642 ),
 ( #23122, #1768 ),
 ( #18762, #6140 ),
 ( #23275, #16262 ),
 ( #18470, #13776 ),
 ( #1918, #4413 ),
 ( #11285, #15647 ),
 ( #20779, #25159 ),
 ( #2839, #7373 ),
 ( #19061, #23574 ),
 ( #7207, #4561 ),
 ( #24187, #30759 ),
 ( #25930, #14064 ),
 ( #14539, #24036 ),
 ( #5025, #26080 ),
 ( #26232, #37 ),
 ( #2218, #10019 ),
 ( #11736, #11904 ),
 ( #21697, #21229 ),
 ( #18923, #9549 ),
 ( #12361, #14684 ),
 ( #14214, #4713 ),
 ( #21865, #499 ),
 ( #16419, #2537 ) ),
 .UNSPECIFIED., .F., .F., .F.,
 ( 4, 3, 3, 3, 3, 3, 3, 3, 3, 3, 4 ),
 ( 2, 2 ),
 ( 0.4999999998345689423, 0.5360336730431939367, 0.5907651151589012883, 0.6456034593241830599, 0.6998270958050434309, 0.7529536536315937223, 0.8052385063053260073, 0.8575343587103997356, 0.9106564858195042023, 0.9648414833209685293, 1.000000006602610014 ),
 ( 0.000000000000000000, 1.000000000000000000 ),
 .UNSPECIFIED. ) ;
#18390 = FACE_OUTER_BOUND ( 'NONE', #8584, .T. ) ;
#18391 = VECTOR ( 'NONE', #5673, 1000.000000000000000 ) ;
#18392 = AXIS2_PLACEMENT_3D ( 'NONE', #20206, #17891, #13522 ) ;
#18393 = CARTESIAN_POINT ( 'NONE',  ( 10.16054539467770113, 13.96046037420044961, 24.50000000000000000 ) ) ;
#18394 = CARTESIAN_POINT ( 'NONE',  ( -20.71335220384823117, 27.86167394782616213, -6.500000000000000888 ) ) ;
#18395 = CARTESIAN_POINT ( 'NONE',  ( -16.99246856547861739, 1.423159825038152082, 18.37415474056476938 ) ) ;
#18396 = CARTESIAN_POINT ( 'NONE',  ( -4.390207617113899730, 7.856594496258241023, -3.621320343559650379 ) ) ;
#18397 = ORIENTED_EDGE ( 'NONE', *, *, #11138, .F. ) ;
#18398 = EDGE_CURVE ( 'NONE', #15560, #21169, #6887, .T. ) ;
#18399 = EDGE_CURVE ( 'NONE', #29153, #11604, #12456, .T. ) ;
#18400 = CARTESIAN_POINT ( 'NONE',  ( -31.05590141235049018, 25.71202138535109327, 17.62027412222990819 ) ) ;
#18401 = CIRCLE ( 'NONE', #3946, 0.7499999999999991118 ) ;
#18402 = CARTESIAN_POINT ( 'NONE',  ( 27.03943647958860197, -26.20092231554396633, 34.80090346875810070 ) ) ;
#18403 = ORIENTED_EDGE ( 'NONE', *, *, #3258, .F. ) ;
#18404 = ORIENTED_EDGE ( 'NONE', *, *, #13774, .F. ) ;
#18405 = LINE ( 'NONE', #6223, #24565 ) ;
#18406 = CARTESIAN_POINT ( 'NONE',  ( -4.596254364928610059, 16.38944764646978314, 6.864725433338323413 ) ) ;
#18407 = ORIENTED_EDGE ( 'NONE', *, *, #942, .T. ) ;
#18408 = CIRCLE ( 'NONE', #22372, 1.000000000000007772 ) ;
#18409 = DIRECTION ( 'NONE',  ( -0.000000000000000000, -0.000000000000000000, 1.000000000000000000 ) ) ;
#18410 = CARTESIAN_POINT ( 'NONE',  ( -12.71614549213497014, 11.31496011770333077, 6.782064869129508899 ) ) ;
#18411 = DIRECTION ( 'NONE',  ( 0.000000000000000000, 0.000000000000000000, 1.000000000000000000 ) ) ;
#18412 = ORIENTED_EDGE ( 'NONE', *, *, #6085, .T. ) ;
#18413 = DIRECTION ( 'NONE',  ( 0.000000000000000000, 1.132880637372608986E-16, -1.000000000000000000 ) ) ;
#18414 = AXIS2_PLACEMENT_3D ( 'NONE', #23319, #1960, #9129 ) ;
#18415 = CARTESIAN_POINT ( 'NONE',  ( -32.28307784207223108, -8.475829241206275455, 41.62281023987519291 ) ) ;
#18416 = VERTEX_POINT ( 'NONE', #14371 ) ;
#18417 = CARTESIAN_POINT ( 'NONE',  ( 25.64627119138473432, -23.40052582045089480, -6.500000000000000888 ) ) ;
#18418 = ORIENTED_EDGE ( 'NONE', *, *, #3520, .T. ) ;
#18419 = PLANE ( 'NONE',  #21898 ) ;
#18420 = ORIENTED_EDGE ( 'NONE', *, *, #24240, .F. ) ;
#18421 = AXIS2_PLACEMENT_3D ( 'NONE', #23939, #233, #11953 ) ;
#18422 = ORIENTED_EDGE ( 'NONE', *, *, #25781, .F. ) ;
#18423 = EDGE_CURVE ( 'NONE', #28337, #18904, #12802, .T. ) ;
#18424 = CARTESIAN_POINT ( 'NONE',  ( -2.931009552726342449, 14.22630671667915792, 1.500000000000000000 ) ) ;
#18425 = CARTESIAN_POINT ( 'NONE',  ( -17.58129253318380947, -9.534052292972809539, 6.523620417364448976 ) ) ;
#18426 = EDGE_CURVE ( 'NONE', #16566, #20079, #20981, .T. ) ;
#18427 = EDGE_LOOP ( 'NONE', ( #12409, #28475, #28912, #2735 ) ) ;
#18428 = AXIS2_PLACEMENT_3D ( 'NONE', #24992, #10805, #3317 ) ;
#18429 = CARTESIAN_POINT ( 'NONE',  ( -11.52197458429825261, -37.50933785548060229, 34.80090346875804386 ) ) ;
#18430 = CARTESIAN_POINT ( 'NONE',  ( 9.582629137048305878, -14.08615220418400860, 18.39701043959520987 ) ) ;
#18431 = CARTESIAN_POINT ( 'NONE',  ( 26.41394434536411140, 32.09691347256533334, -6.500000000000000888 ) ) ;
#18432 = ORIENTED_EDGE ( 'NONE', *, *, #12611, .F. ) ;
#18433 = CARTESIAN_POINT ( 'NONE',  ( -19.73500371898430217, 3.353449004226455088, 19.87181966307587544 ) ) ;
#18434 = CARTESIAN_POINT ( 'NONE',  ( 15.81223571690235730, -6.365019318618788446, 7.652108011868850035 ) ) ;
#18435 = CARTESIAN_POINT ( 'NONE',  ( -13.97362136398187182, 9.814707526993062814, 6.995624166085161910 ) ) ;
#18436 = CARTESIAN_POINT ( 'NONE',  ( 3.283642163210877207, 16.75135354181591296, 19.97651184436794125 ) ) ;
#18437 = VERTEX_POINT ( 'NONE', #22308 ) ;
#18438 = ORIENTED_EDGE ( 'NONE', *, *, #13211, .F. ) ;
#18439 = DIRECTION ( 'NONE',  ( 0.000000000000000000, 0.000000000000000000, -1.000000000000000000 ) ) ;
#18440 = CARTESIAN_POINT ( 'NONE',  ( 49.99999999999998579, 50.00000000000000000, -87.50000000000000000 ) ) ;
#18441 = CARTESIAN_POINT ( 'NONE',  ( 15.40940123050674693, 12.74987339073082637, 19.96302680909623817 ) ) ;
#18442 = CARTESIAN_POINT ( 'NONE',  ( -5.216068956281039171, 19.32652695433950285, 18.71435384576123440 ) ) ;
#18443 = CARTESIAN_POINT ( 'NONE',  ( 0.000000000000000000, 0.000000000000000000, 1.500000000000001332 ) ) ;
#18444 = CARTESIAN_POINT ( 'NONE',  ( 49.99999999999998579, 50.00000000000000000, -92.50000000000000000 ) ) ;
#18445 = CARTESIAN_POINT ( 'NONE',  ( -4.915268975789784278, 39.22418258073496844, 27.50000000000000355 ) ) ;
#18446 = CARTESIAN_POINT ( 'NONE',  ( -2.703030265324078307, -12.75514121382991384, 24.50000000000000000 ) ) ;
#18447 = ORIENTED_EDGE ( 'NONE', *, *, #15276, .T. ) ;
#18448 = CARTESIAN_POINT ( 'NONE',  ( -17.00407983531365019, 1.321870115990435801, 7.603368798681074736 ) ) ;
#18449 = DIRECTION ( 'NONE',  ( -4.625929269271481378E-15, 1.000000000000000000, 0.000000000000000000 ) ) ;
#18450 = CARTESIAN_POINT ( 'NONE',  ( 4.102102735472461958, -8.549050687778175117, 1.500000000000001332 ) ) ;
#18451 = ORIENTED_EDGE ( 'NONE', *, *, #19285, .T. ) ;
#18452 = DIRECTION ( 'NONE',  ( -0.000000000000000000, -0.000000000000000000, 1.000000000000000000 ) ) ;
#18453 = ORIENTED_EDGE ( 'NONE', *, *, #16572, .T. ) ;
#18454 = CARTESIAN_POINT ( 'NONE',  ( 7.869584159753955532, 10.39565510934977333, 1.500000000000001332 ) ) ;
#18455 = LINE ( 'NONE', #17836, #25967 ) ;
#18456 = ORIENTED_EDGE ( 'NONE', *, *, #25356, .T. ) ;
#18457 = CARTESIAN_POINT ( 'NONE',  ( -0.2646837113541495867, -19.99846847964001739, 5.849008070840544526 ) ) ;
#18458 = CARTESIAN_POINT ( 'NONE',  ( 9.634323311075775109, 1.438332125858202692, 1.500000000000001332 ) ) ;
#18459 = CARTESIAN_POINT ( 'NONE',  ( 69.99999999999998579, -70.00000000000000000, 12.49999999999999112 ) ) ;
#18460 = DIRECTION ( 'NONE',  ( -1.000000000000000000, 0.000000000000000000, 0.000000000000000000 ) ) ;
#18461 = CIRCLE ( 'NONE', #26419, 10.00000000000000000 ) ;
#18462 = CARTESIAN_POINT ( 'NONE',  ( 1.438332125858173605, -8.884323311075778662, -1.500000000000002665 ) ) ;
#18463 = DIRECTION ( 'NONE',  ( -0.000000000000000000, -0.000000000000000000, -1.000000000000000000 ) ) ;
#18464 = CARTESIAN_POINT ( 'NONE',  ( -10.18506332983504237, -29.04537757311072710, 24.50000000000000000 ) ) ;
#18465 = EDGE_LOOP ( 'NONE', ( #4783, #19162, #24919 ) ) ;
#18466 = CARTESIAN_POINT ( 'NONE',  ( -19.84344116185557283, 2.497567387674354489, 20.34789198813115263 ) ) ;
#18467 = CARTESIAN_POINT ( 'NONE',  ( -24.03057240117691862, 26.57182937991348481, 26.54355021145562787 ) ) ;
#18468 = ORIENTED_EDGE ( 'NONE', *, *, #4048, .F. ) ;
#18469 = CARTESIAN_POINT ( 'NONE',  ( -11.21147646446735102, -30.29926891764210595, 1.500000000000000000 ) ) ;
#18470 = CARTESIAN_POINT ( 'NONE',  ( -17.63988435498684382, -9.462624493092880229, 18.92976555901915603 ) ) ;
#18471 = CARTESIAN_POINT ( 'NONE',  ( -5.105024945673440229, 42.22604126506271172, -1.500000000000000000 ) ) ;
#18472 = CARTESIAN_POINT ( 'NONE',  ( 20.65888525914375862, -38.75220717792901581, -19.50000000000000355 ) ) ;
#18473 = VERTEX_POINT ( 'NONE', #12811 ) ;
#18474 = LINE ( 'NONE', #7060, #23367 ) ;
#18475 = DIRECTION ( 'NONE',  ( -0.000000000000000000, -0.000000000000000000, -1.000000000000000000 ) ) ;
#18476 = CARTESIAN_POINT ( 'NONE',  ( 38.89666010881209957, -3.348336038578077822, 32.19909834651174663 ) ) ;
#18477 = DIRECTION ( 'NONE',  ( 0.000000000000000000, -0.000000000000000000, -1.000000000000000000 ) ) ;
#18478 = ORIENTED_EDGE ( 'NONE', *, *, #15839, .F. ) ;
#18479 = AXIS2_PLACEMENT_3D ( 'NONE', #22261, #7771, #5274 ) ;
#18480 = PLANE ( 'NONE',  #14101 ) ;
#18481 = CARTESIAN_POINT ( 'NONE',  ( 34.07766914598172292, -21.40380666527112652, -1.500000000000000000 ) ) ;
#18482 = DIRECTION ( 'NONE',  ( 0.000000000000000000, 0.000000000000000000, -1.000000000000000000 ) ) ;
#18483 = ORIENTED_EDGE ( 'NONE', *, *, #24018, .F. ) ;
#18484 = CARTESIAN_POINT ( 'NONE',  ( -5.127072261997696501, -42.13114360820387105, 28.87158698979378713 ) ) ;
#18485 = ORIENTED_EDGE ( 'NONE', *, *, #17061, .T. ) ;
#18486 = CARTESIAN_POINT ( 'NONE',  ( -31.45274955338950207, 26.35877938683250576, -8.166661939820002658 ) ) ;
#18487 = CARTESIAN_POINT ( 'NONE',  ( -10.23401665697056195, -17.20427178438287186, 5.704143890883081269 ) ) ;
#18488 = DIRECTION ( 'NONE',  ( -0.000000000000000000, -0.000000000000000000, -1.000000000000000000 ) ) ;
#18489 = CARTESIAN_POINT ( 'NONE',  ( -23.21352257770656990, 10.78826658734919519, 45.15942333309111234 ) ) ;
#18490 = ORIENTED_EDGE ( 'NONE', *, *, #2170, .T. ) ;
#18491 = CARTESIAN_POINT ( 'NONE',  ( 12.18183868328554809, 11.93592587881222933, 20.34789198813114908 ) ) ;
#18492 = EDGE_CURVE ( 'NONE', #9106, #13113, #16868, .T. ) ;
#18493 = LINE ( 'NONE', #20815, #25834 ) ;
#18494 = DIRECTION ( 'NONE',  ( 1.000000000000000000, 0.000000000000000000, 0.000000000000000000 ) ) ;
#18495 = EDGE_CURVE ( 'NONE', #23990, #2092, #9806, .T. ) ;
#18496 = AXIS2_PLACEMENT_3D ( 'NONE', #4240, #6278, #25149 ) ;
#18497 = DIRECTION ( 'NONE',  ( 0.000000000000000000, 0.000000000000000000, 1.000000000000000000 ) ) ;
#18498 = VECTOR ( 'NONE', #24145, 1000.000000000000000 ) ;
#18499 = CARTESIAN_POINT ( 'NONE',  ( -25.07950435457407323, 11.50806656539752737, -16.55003854064094426 ) ) ;
#18500 = DIRECTION ( 'NONE',  ( -1.000000000000000000, 0.000000000000000000, 0.000000000000000000 ) ) ;
#18501 = DIRECTION ( 'NONE',  ( 1.000000000000000000, 0.000000000000000000, 0.000000000000000000 ) ) ;
#18502 = CARTESIAN_POINT ( 'NONE',  ( 16.80116347819186373, 38.39680910286394777, 23.11187228430608087 ) ) ;
#18503 = CARTESIAN_POINT ( 'NONE',  ( -18.44586851731391519, -7.729974993529595828, 19.60917204426171168 ) ) ;
#18504 = CARTESIAN_POINT ( 'NONE',  ( -15.56851150445305088, -6.881932713941044888, 19.56050940960062690 ) ) ;
#18505 = CARTESIAN_POINT ( 'NONE',  ( -9.290115248478288734, -14.26557846606243807, 19.85270094495842130 ) ) ;
#18506 = VERTEX_POINT ( 'NONE', #487 ) ;
#18507 = ORIENTED_EDGE ( 'NONE', *, *, #2498, .T. ) ;
#18508 = EDGE_CURVE ( 'NONE', #23584, #7538, #633, .T. ) ;
#18509 = DIRECTION ( 'NONE',  ( 1.000000000000000000, 0.000000000000000000, 0.000000000000000000 ) ) ;
#18510 = CARTESIAN_POINT ( 'NONE',  ( 39.00000000000000000, 5.563236990218597633, -1.500000000000000000 ) ) ;
#18511 = LINE ( 'NONE', #7107, #27345 ) ;
#18512 = VERTEX_POINT ( 'NONE', #22156 ) ;
#18513 = CARTESIAN_POINT ( 'NONE',  ( 49.99999999999999289, -50.00000000000000000, 70.00000000000000000 ) ) ;
#18514 = CARTESIAN_POINT ( 'NONE',  ( 15.58729175431054337, -6.863221649612937014, 20.19668224736330941 ) ) ;
#18515 = CARTESIAN_POINT ( 'NONE',  ( 5.278755796068665518, 7.392982946727100213, -1.500000000000000888 ) ) ;
#18516 = ORIENTED_EDGE ( 'NONE', *, *, #19851, .F. ) ;
#18517 = CARTESIAN_POINT ( 'NONE',  ( -19.70840172719294614, 3.506524300503914837, 6.641371103590088865 ) ) ;
#18518 = AXIS2_PLACEMENT_3D ( 'NONE', #4392, #16545, #7192 ) ;
#18519 = CARTESIAN_POINT ( 'NONE',  ( -10.89423172471906831, -16.79374140667819759, 18.44501272782439827 ) ) ;
#18520 = CARTESIAN_POINT ( 'NONE',  ( -50.00000000000000000, 87.00000000000001421, 22.49999999999999289 ) ) ;
#18521 = ORIENTED_EDGE ( 'NONE', *, *, #25806, .T. ) ;
#18522 = DIRECTION ( 'NONE',  ( -0.6707505147970023174, 0.7416830501633134842, 0.000000000000000000 ) ) ;
#18523 = ADVANCED_FACE ( 'NONE', ( #24648 ), #5479, .F. ) ;
#18524 = ADVANCED_FACE ( 'NONE', ( #21683 ), #322, .F. ) ;
#18525 = DIRECTION ( 'NONE',  ( 0.3598999890241700306, -0.9329908884337522190, 0.000000000000000000 ) ) ;
#18526 = FACE_OUTER_BOUND ( 'NONE', #212, .T. ) ;
#18527 = ORIENTED_EDGE ( 'NONE', *, *, #26344, .F. ) ;
#18528 = CARTESIAN_POINT ( 'NONE',  ( 16.85625572095001701, 2.395390699382102362, 19.96344307082652492 ) ) ;
#18529 = EDGE_CURVE ( 'NONE', #19397, #12669, #17755, .T. ) ;
#18530 = CARTESIAN_POINT ( 'NONE',  ( -5.976020107417636673, 19.08630880174946043, 18.34798005863226678 ) ) ;
#18531 = CARTESIAN_POINT ( 'NONE',  ( -0.1401636875787305447, -17.02258069761206372, 7.080843742048788414 ) ) ;
#18532 = CARTESIAN_POINT ( 'NONE',  ( 15.81416692036122207, -6.360574302898111654, 18.34798005863078885 ) ) ;
#18533 = DIRECTION ( 'NONE',  ( 0.9096319953545183301, 0.4154150130018865461, 0.000000000000000000 ) ) ;
#18534 = CARTESIAN_POINT ( 'NONE',  ( -17.06249589246193565, 0.6902251470929382515, 19.03762469184452755 ) ) ;
#18535 = DIRECTION ( 'NONE',  ( 0.000000000000000000, 0.000000000000000000, 1.000000000000000000 ) ) ;
#18536 = VERTEX_POINT ( 'NONE', #12662 ) ;
#18537 = EDGE_CURVE ( 'NONE', #23884, #28674, #16504, .T. ) ;
#18538 = EDGE_CURVE ( 'NONE', #14619, #8580, #18785, .T. ) ;
#18539 = CARTESIAN_POINT ( 'NONE',  ( -6.458576814766982643, 15.80792270644319331, 6.329955581934036069 ) ) ;
#18540 = CIRCLE ( 'NONE', #22504, 7.500000000000000000 ) ;
#18541 = CARTESIAN_POINT ( 'NONE',  ( 34.83396020575241891, -10.30249279383517624, 27.50000000000001066 ) ) ;
#18542 = ADVANCED_FACE ( 'NONE', ( #15132 ), #12506, .F. ) ;
#18543 = EDGE_LOOP ( 'NONE', ( #6622, #23823, #1747, #20828 ) ) ;
#18544 = ORIENTED_EDGE ( 'NONE', *, *, #24279, .F. ) ;
#18545 = ADVANCED_FACE ( 'NONE', ( #29026 ), #3153, .T. ) ;
#18546 = DIRECTION ( 'NONE',  ( 0.000000000000000000, 0.000000000000000000, -1.000000000000000000 ) ) ;
#18547 = EDGE_LOOP ( 'NONE', ( #16705, #16511, #18342, #19873 ) ) ;
#18548 = DIRECTION ( 'NONE',  ( -0.000000000000000000, -0.000000000000000000, 1.000000000000000000 ) ) ;
#18549 = CARTESIAN_POINT ( 'NONE',  ( -11.82521593960875528, 5.400395169024524655, 1.500000000000001332 ) ) ;
#18550 = ORIENTED_EDGE ( 'NONE', *, *, #3708, .F. ) ;
#18551 = VECTOR ( 'NONE', #20171, 1000.000000000000000 ) ;
#18552 = CARTESIAN_POINT ( 'NONE',  ( -19.54426622602688113, 37.07991288358297055, -1.499999999999999778 ) ) ;
#18553 = CARTESIAN_POINT ( 'NONE',  ( -33.56595177138117947, -10.45696648424866204, 39.84323675257729747 ) ) ;
#18554 = EDGE_LOOP ( 'NONE', ( #11044, #25716, #5628, #9754 ) ) ;
#18555 = CARTESIAN_POINT ( 'NONE',  ( 6.900000000000000355, 0.000000000000000000, 0.000000000000000000 ) ) ;
#18556 = ADVANCED_FACE ( 'NONE', ( #15596 ), #1427, .F. ) ;
#18557 = VERTEX_POINT ( 'NONE', #25115 ) ;
#18558 = CARTESIAN_POINT ( 'NONE',  ( 37.16608720827707657, 65.00000000000000000, 57.49999999999999289 ) ) ;
#18559 = ADVANCED_FACE ( 'NONE', ( #29648 ), #26305, .F. ) ;
#18560 = EDGE_LOOP ( 'NONE', ( #14700, #17174, #29840 ) ) ;
#18561 = EDGE_CURVE ( 'NONE', #10191, #21504, #9307, .T. ) ;
#18562 = ORIENTED_EDGE ( 'NONE', *, *, #22477, .T. ) ;
#18563 = EDGE_CURVE ( 'NONE', #12285, #20725, #24109, .T. ) ;
#18564 = CARTESIAN_POINT ( 'NONE',  ( -22.58267429318970443, -26.57182937991348481, 26.54355021145563143 ) ) ;
#18565 = CARTESIAN_POINT ( 'NONE',  ( 0.2718907110559959928, -17.03030470364380733, 20.22273502201483453 ) ) ;
#18566 = VECTOR ( 'NONE', #26125, 1000.000000000000000 ) ;
#18567 = AXIS2_PLACEMENT_3D ( 'NONE', #23838, #28381, #16515 ) ;
#18568 = CARTESIAN_POINT ( 'NONE',  ( 8.549050687778162683, 4.102102735472485051, 21.50000000000000000 ) ) ;
#18569 = CARTESIAN_POINT ( 'NONE',  ( 19.87213478643044340, 2.412525337365567513, 18.71435384576123440 ) ) ;
#18570 = ORIENTED_EDGE ( 'NONE', *, *, #1000, .T. ) ;
#18571 = EDGE_CURVE ( 'NONE', #8044, #8694, #5094, .T. ) ;
#18572 = VECTOR ( 'NONE', #27091, 1000.000000000000000 ) ;
#18573 = CARTESIAN_POINT ( 'NONE',  ( 10.74273727477993390, -16.89139546617319354, 7.557577766377196582 ) ) ;
#18574 = CARTESIAN_POINT ( 'NONE',  ( -50.00000000000000000, 50.00000000000000000, 97.07879600563551037 ) ) ;
#18575 = CARTESIAN_POINT ( 'NONE',  ( -13.99683207193583279, 9.784088562599672301, 6.892848776733236704 ) ) ;
#18576 = CARTESIAN_POINT ( 'NONE',  ( 4.400293182487616583, 19.52803631353506120, 18.92976555901915603 ) ) ;
#18577 = ORIENTED_EDGE ( 'NONE', *, *, #28868, .T. ) ;
#18578 = EDGE_LOOP ( 'NONE', ( #20572, #27919, #12941, #23206 ) ) ;
#18579 = CARTESIAN_POINT ( 'NONE',  ( 0.000000000000000000, 0.000000000000000000, -16.50000000000000000 ) ) ;
#18580 = CARTESIAN_POINT ( 'NONE',  ( -25.64627119138473432, -23.40052582045089480, -16.50000600000000262 ) ) ;
#18581 = CARTESIAN_POINT ( 'NONE',  ( 32.50000000000000000, 3.980102097228898626E-15, -52.50000000000000000 ) ) ;
#18582 = DIRECTION ( 'NONE',  ( 0.000000000000000000, 1.000000000000000000, -0.000000000000000000 ) ) ;
#18583 = CARTESIAN_POINT ( 'NONE',  ( -20.17405764020900705, 32.71829193411804937, 27.50000000000000000 ) ) ;
#18584 = DIRECTION ( 'NONE',  ( -1.000000000000000000, 0.000000000000000000, 0.000000000000000000 ) ) ;
#18585 = ADVANCED_FACE ( 'NONE', ( #14606 ), #29305, .T. ) ;
#18586 = ORIENTED_EDGE ( 'NONE', *, *, #28057, .T. ) ;
#18587 = ADVANCED_FACE ( 'NONE', ( #3063 ), #29267, .T. ) ;
#18588 = EDGE_CURVE ( 'NONE', #27029, #24252, #10544, .T. ) ;
#18589 = CARTESIAN_POINT ( 'NONE',  ( 1.368946144808715015, -19.95309466511745811, 6.523620417364439206 ) ) ;
#18590 = CARTESIAN_POINT ( 'NONE',  ( -5.604556300746500241, -15.53790034020399169, 24.50000000000000000 ) ) ;
#18591 = CARTESIAN_POINT ( 'NONE',  ( 39.52380524535562500, 7.028748154183637631, -6.500000000000000888 ) ) ;
#18592 = VERTEX_POINT ( 'NONE', #19590 ) ;
#18593 = FACE_OUTER_BOUND ( 'NONE', #21752, .T. ) ;
#18594 = VECTOR ( 'NONE', #11273, 1000.000000000000000 ) ;
#18595 = EDGE_LOOP ( 'NONE', ( #25412, #29069 ) ) ;
#18596 = DIRECTION ( 'NONE',  ( 1.000000000000000000, 0.000000000000000000, -0.000000000000000000 ) ) ;
#18597 = AXIS2_PLACEMENT_3D ( 'NONE', #25788, #28128, #1920 ) ;
#18598 = CARTESIAN_POINT ( 'NONE',  ( -8.456776945386934585E-15, 29.50000000000000000, 24.50000000000000000 ) ) ;
#18599 = VERTEX_POINT ( 'NONE', #24725 ) ;
#18600 = CARTESIAN_POINT ( 'NONE',  ( 4.948301831468912226, -39.21750186235175306, 27.50000000000001066 ) ) ;
#18601 = CARTESIAN_POINT ( 'NONE',  ( -39.52380524536136619, -7.028748154183644736, -11.49999999999999645 ) ) ;
#18602 = CARTESIAN_POINT ( 'NONE',  ( -4.163336342344337027E-14, 1.387778780781445676E-14, 67.49999999999997158 ) ) ;
#18603 = CARTESIAN_POINT ( 'NONE',  ( 13.00999358272542850, -0.8602714556717643291, 1.500000000000001332 ) ) ;
#18604 = CARTESIAN_POINT ( 'NONE',  ( -6.656778417335413423, 18.87854210339739325, 20.06253562465620632 ) ) ;
#18605 = DIRECTION ( 'NONE',  ( -1.000000000000000000, 0.000000000000000000, 0.000000000000000000 ) ) ;
#18606 = DIRECTION ( 'NONE',  ( -0.000000000000000000, -0.000000000000000000, -1.000000000000000000 ) ) ;
#18607 = EDGE_LOOP ( 'NONE', ( #29022, #1817, #4132 ) ) ;
#18608 = AXIS2_PLACEMENT_3D ( 'NONE', #19703, #12861, #17847 ) ;
#18609 = CARTESIAN_POINT ( 'NONE',  ( 0.000000000000000000, 0.000000000000000000, 1.500000000000001332 ) ) ;
#18610 = CARTESIAN_POINT ( 'NONE',  ( 15.81223572262636878, -6.365019322297388094, 20.34789198813115263 ) ) ;
#18611 = ORIENTED_EDGE ( 'NONE', *, *, #22710, .T. ) ;
#18612 = DIRECTION ( 'NONE',  ( -0.000000000000000000, 0.000000000000000000, 1.000000000000000000 ) ) ;
#18613 = AXIS2_PLACEMENT_3D ( 'NONE', #11209, #17937, #4036 ) ;
#18614 = CARTESIAN_POINT ( 'NONE',  ( 0.07661102881318986035, -8.673996836102570995, 2.976196775178701515 ) ) ;
#18615 = VECTOR ( 'NONE', #11559, 1000.000000000000227 ) ;
#18616 = DIRECTION ( 'NONE',  ( -0.000000000000000000, 1.000000000000000000, 0.000000000000000000 ) ) ;
#18617 = VERTEX_POINT ( 'NONE', #15198 ) ;
#18618 = CARTESIAN_POINT ( 'NONE',  ( -0.1522245795255700584, -19.99979613760744002, 18.47110296274026098 ) ) ;
#18619 = DIRECTION ( 'NONE',  ( 0.000000000000000000, 0.000000000000000000, 1.000000000000000000 ) ) ;
#18620 = CARTESIAN_POINT ( 'NONE',  ( 12.13427030824643715, -40.39764110210223436, 29.02507812129452347 ) ) ;
#18621 = DIRECTION ( 'NONE',  ( -0.2817325568414293380, -0.9594929736144974797, 0.000000000000000000 ) ) ;
#18622 = VERTEX_POINT ( 'NONE', #14748 ) ;
#18623 = CARTESIAN_POINT ( 'NONE',  ( -13.99139173414245185, 9.791236547353763697, 6.392658652357120275 ) ) ;
#18624 = ORIENTED_EDGE ( 'NONE', *, *, #23873, .F. ) ;
#18625 = EDGE_CURVE ( 'NONE', #21717, #9927, #29425, .T. ) ;
#18626 = CARTESIAN_POINT ( 'NONE',  ( 2.552544030762014415, -42.50000000000000000, -1.500000000000000000 ) ) ;
#18627 = CARTESIAN_POINT ( 'NONE',  ( 4.102102735472459294, -8.549050687778176894, 13.00000000000000178 ) ) ;
#18628 = EDGE_CURVE ( 'NONE', #24994, #5507, #17417, .T. ) ;
#18629 = EDGE_LOOP ( 'NONE', ( #1304, #22032, #4630, #24711, #16366 ) ) ;
#18630 = PRODUCT_DEFINITION_SHAPE ( 'NONE', 'NONE',  #30869 ) ;
#18631 = CARTESIAN_POINT ( 'NONE',  ( 16.65271093598738261, 3.715728438010606816, 18.45571264222803620 ) ) ;
#18632 = ORIENTED_EDGE ( 'NONE', *, *, #8434, .T. ) ;
#18633 = LINE ( 'NONE', #1788, #3923 ) ;
#18634 = VECTOR ( 'NONE', #13786, 1000.000000000000114 ) ;
#18635 = VECTOR ( 'NONE', #2482, 1000.000000000000000 ) ;
#18636 = DIRECTION ( 'NONE',  ( -0.000000000000000000, 0.000000000000000000, 1.000000000000000000 ) ) ;
#18637 = CARTESIAN_POINT ( 'NONE',  ( 7.028330626922776325, 10.93629592680536966, 1.500000000000001332 ) ) ;
#18638 = ORIENTED_EDGE ( 'NONE', *, *, #23669, .F. ) ;
#18639 = CARTESIAN_POINT ( 'NONE',  ( 23.94376008874366235, 13.17067969463889732, 43.43030304407326270 ) ) ;
#18640 = CARTESIAN_POINT ( 'NONE',  ( 26.83043119477639138, -8.695877139419035728, 1.500000000000000000 ) ) ;
#18641 = CARTESIAN_POINT ( 'NONE',  ( -52.16608720827707657, 51.86186943028246787, 12.49999999999998401 ) ) ;
#18642 = CARTESIAN_POINT ( 'NONE',  ( 33.42925964089141644, -11.06161099612213228, 35.54550565580004928 ) ) ;
#18643 = ORIENTED_EDGE ( 'NONE', *, *, #28412, .T. ) ;
#18644 = CYLINDRICAL_SURFACE ( 'NONE', #6799, 0.6002263538043630664 ) ;
#18645 = CARTESIAN_POINT ( 'NONE',  ( -18.58529988941444344, 7.388276390372320535, 24.50000000000000000 ) ) ;
#18646 = CARTESIAN_POINT ( 'NONE',  ( 49.99999999999998579, 50.00000000000000000, 12.49999999999998401 ) ) ;
#18647 = CYLINDRICAL_SURFACE ( 'NONE', #14024, 10.00000000000003375 ) ;
#18648 = CARTESIAN_POINT ( 'NONE',  ( 3.790840891470688589, 16.62820496721823815, 18.34938820207545618 ) ) ;
#18649 = CARTESIAN_POINT ( 'NONE',  ( -24.35970437652574105, 13.37404834226503247, 42.96778633356043287 ) ) ;
#18650 = CARTESIAN_POINT ( 'NONE',  ( -15.57772019539775421, -6.859948791675929414, 19.45164628100866722 ) ) ;
#18651 = DIRECTION ( 'NONE',  ( 0.000000000000000000, 0.000000000000000000, 1.000000000000000000 ) ) ;
#18652 = ORIENTED_EDGE ( 'NONE', *, *, #11025, .T. ) ;
#18653 = ORIENTED_EDGE ( 'NONE', *, *, #19693, .T. ) ;
#18654 = DIRECTION ( 'NONE',  ( 0.5406408174555974444, 0.8412535328311813165, 0.000000000000000000 ) ) ;
#18655 = CARTESIAN_POINT ( 'NONE',  ( -7.671651850954201990, -15.25824679864873445, 6.588756557121049795 ) ) ;
#18656 = CARTESIAN_POINT ( 'NONE',  ( 6.482337650448408262, 6.364020599487815844, 13.22130136205108819 ) ) ;
#18657 = VERTEX_POINT ( 'NONE', #26936 ) ;
#18658 = DIRECTION ( 'NONE',  ( 0.000000000000000000, 0.000000000000000000, 1.000000000000000000 ) ) ;
#18659 = CARTESIAN_POINT ( 'NONE',  ( 15.51152286861889529, -7.023094163498092790, 20.05479082170252525 ) ) ;
#18660 = CARTESIAN_POINT ( 'NONE',  ( 5.021901920966175048, 16.26348455184633579, 6.641371103590088865 ) ) ;
#18661 = ORIENTED_EDGE ( 'NONE', *, *, #15485, .T. ) ;
#18662 = CARTESIAN_POINT ( 'NONE',  ( -16.83148396119934631, 2.548526378087588640, 6.211014596808754007 ) ) ;
#18663 = CARTESIAN_POINT ( 'NONE',  ( 14.20032907733019556, 14.10870362182394722, 6.782048567692550378 ) ) ;
#18664 = CARTESIAN_POINT ( 'NONE',  ( -23.27838112031802709, -36.10018649381529343, -16.50000600000000262 ) ) ;
#18665 = CARTESIAN_POINT ( 'NONE',  ( -35.06085151626346175, 18.66574915858497619, 34.76280655890868587 ) ) ;
#18666 = ORIENTED_EDGE ( 'NONE', *, *, #14683, .T. ) ;
#18667 = CARTESIAN_POINT ( 'NONE',  ( -1.195154792889455697, -9.406652940105981742, 13.00000000000000178 ) ) ;
#18668 = CARTESIAN_POINT ( 'NONE',  ( -14.70620249426165849, -8.682611668023952234, 6.521906765011494578 ) ) ;
#18669 = CARTESIAN_POINT ( 'NONE',  ( -14.94050307174418712, 13.29624634855319698, 5.849008070840538309 ) ) ;
#18670 = ORIENTED_EDGE ( 'NONE', *, *, #17534, .F. ) ;
#18671 = VECTOR ( 'NONE', #8010, 1000.000000000000000 ) ;
#18672 = CARTESIAN_POINT ( 'NONE',  ( 16.87858066272376689, 2.200498455871256365, 19.47784884541372108 ) ) ;
#18673 = CARTESIAN_POINT ( 'NONE',  ( 24.57973596967191554, -7.302173446879564267, 45.11631295118271368 ) ) ;
#18674 = CARTESIAN_POINT ( 'NONE',  ( 11.21147646446735102, -30.29926891764210595, -1.500000000000000000 ) ) ;
#18675 = CARTESIAN_POINT ( 'NONE',  ( 37.99999999999999289, 80.00000000000000000, 27.08257569495583184 ) ) ;
#18676 = FACE_OUTER_BOUND ( 'NONE', #23818, .T. ) ;
#18677 = B_SPLINE_CURVE_WITH_KNOTS ( 'NONE', 3,
 ( #5191, #347, #9870, #17353, #21875, #3165, #19387, #7841, #28905, #812 ),
 .UNSPECIFIED., .F., .F.,
 ( 4, 3, 3, 4 ),
 ( -0.005033671593837414984, 0.000000000000000000, 0.005033946531780188541, 0.01006789358107997023 ),
 .UNSPECIFIED. ) ;
#18678 = CARTESIAN_POINT ( 'NONE',  ( -2.810445847081918913, -9.056208293496299078, 13.00000000000000178 ) ) ;
#18679 = CARTESIAN_POINT ( 'NONE',  ( -19.96205336850438883, 1.490391487655212899, 19.36813350477385143 ) ) ;
#18680 = DIRECTION ( 'NONE',  ( 1.000000000000000000, 0.000000000000000000, 0.000000000000000000 ) ) ;
#18681 = ORIENTED_EDGE ( 'NONE', *, *, #23679, .T. ) ;
#18682 = DIRECTION ( 'NONE',  ( -0.000000000000000000, -0.000000000000000000, 1.000000000000000000 ) ) ;
#18683 = DIRECTION ( 'NONE',  ( 1.000000000000000000, 0.000000000000000000, -0.000000000000000000 ) ) ;
#18684 = ORIENTED_EDGE ( 'NONE', *, *, #7846, .T. ) ;
#18685 = EDGE_LOOP ( 'NONE', ( #6985, #7719, #556, #17363 ) ) ;
#18686 = CARTESIAN_POINT ( 'NONE',  ( 10.47960520055065992, -7.757439966934453146, 1.500000000000001332 ) ) ;
#18687 = EDGE_CURVE ( 'NONE', #20672, #10252, #26254, .T. ) ;
#18688 = ORIENTED_EDGE ( 'NONE', *, *, #20067, .T. ) ;
#18689 =( BOUNDED_SURFACE ( )  B_SPLINE_SURFACE ( 3, 1, ( 
 ( #4976, #19166 ),
 ( #2791, #22116 ),
 ( #14951, #17131 ),
 ( #10262, #28686 ) ),
 .UNSPECIFIED., .F., .F., .T. ) 
 B_SPLINE_SURFACE_WITH_KNOTS ( ( 4, 4 ),
 ( 2, 2 ),
 ( 0.000000000000000000, 1.000000000000000000 ),
 ( 0.000000000000000000, 1.000000000000000000 ),
 .UNSPECIFIED. ) 
 GEOMETRIC_REPRESENTATION_ITEM ( )  RATIONAL_B_SPLINE_SURFACE ( (
 ( 1.000000000000000000, 1.000000000000000000),
 ( 0.9908525036704132205, 0.9908525036704132205),
 ( 0.9908525036704132205, 0.9908525036704132205),
 ( 1.000000000000000000, 1.000000000000000000) ) ) 
 REPRESENTATION_ITEM ( '' )  SURFACE ( )  );
#18690 = FACE_OUTER_BOUND ( 'NONE', #19131, .T. ) ;
#18691 = VECTOR ( 'NONE', #26845, 1000.000000000000000 ) ;
#18692 = DIRECTION ( 'NONE',  ( 0.2972711322815266288, -0.9547931052914337968, 0.000000000000000000 ) ) ;
#18693 = ORIENTED_EDGE ( 'NONE', *, *, #7108, .T. ) ;
#18694 = ADVANCED_FACE ( 'NONE', ( #5408 ), #15054, .T. ) ;
#18695 = DIRECTION ( 'NONE',  ( 0.000000000000000000, 0.000000000000000000, 1.000000000000000000 ) ) ;
#18696 = CARTESIAN_POINT ( 'NONE',  ( 3.637110358602580362, -19.99473753024311762, -1.500000000000000000 ) ) ;
#18697 = ORIENTED_EDGE ( 'NONE', *, *, #1489, .T. ) ;
#18698 = ORIENTED_EDGE ( 'NONE', *, *, #30363, .F. ) ;
#18699 = ADVANCED_FACE ( 'NONE', ( #24571 ), #1189, .T. ) ;
#18700 = DIRECTION ( 'NONE',  ( 1.000000000000000000, 4.440892098500626162E-15, 0.000000000000000000 ) ) ;
#18701 = ORIENTED_EDGE ( 'NONE', *, *, #1327, .F. ) ;
#18702 = EDGE_CURVE ( 'NONE', #13171, #7773, #22758, .T. ) ;
#18703 = CIRCLE ( 'NONE', #11732, 6.000000000000005329 ) ;
#18704 = ORIENTED_EDGE ( 'NONE', *, *, #17566, .T. ) ;
#18705 = EDGE_CURVE ( 'NONE', #26694, #26441, #8059, .T. ) ;
#18706 = DIRECTION ( 'NONE',  ( -0.6707505147970024284, -0.7416830501633134842, 0.000000000000000000 ) ) ;
#18707 = CARTESIAN_POINT ( 'NONE',  ( -17.64439154790314390, -9.416908767371234390, 7.161525567826898531 ) ) ;
#18708 = VECTOR ( 'NONE', #9701, 1000.000000000000000 ) ;
#18709 = DIRECTION ( 'NONE',  ( 1.000000000000000000, 0.000000000000000000, 0.000000000000000000 ) ) ;
#18710 = DIRECTION ( 'NONE',  ( 0.000000000000000000, -1.132880637372608986E-16, 1.000000000000000000 ) ) ;
#18711 = CARTESIAN_POINT ( 'NONE',  ( 19.81199842303382042, 2.865066961627989350, 18.39701043959520987 ) ) ;
#18712 = ORIENTED_EDGE ( 'NONE', *, *, #23115, .T. ) ;
#18713 = CARTESIAN_POINT ( 'NONE',  ( -16.92089108241427198, 1.982400079378048963, 18.39701043959520987 ) ) ;
#18714 = PLANE ( 'NONE',  #11283 ) ;
#18715 = AXIS2_PLACEMENT_3D ( 'NONE', #6076, #5927, #8439 ) ;
#18716 = CARTESIAN_POINT ( 'NONE',  ( -15.76141475779636814, 12.34077778289584160, 5.872146474157316831 ) ) ;
#18717 = DIRECTION ( 'NONE',  ( -0.7557495743542579358, 0.6548607339452854337, -0.000000000000000000 ) ) ;
#18718 = ORIENTED_EDGE ( 'NONE', *, *, #13934, .F. ) ;
#18719 = ORIENTED_EDGE ( 'NONE', *, *, #12618, .F. ) ;
#18720 = CARTESIAN_POINT ( 'NONE',  ( 40.05104235265675783, 2.353288714459732311, -6.500000000000000888 ) ) ;
#18721 = EDGE_CURVE ( 'NONE', #14619, #5400, #20196, .T. ) ;
#18722 = CARTESIAN_POINT ( 'NONE',  ( 6.187077094091595342, 11.47693674426096599, 1.500000000000001332 ) ) ;
#18723 = EDGE_CURVE ( 'NONE', #8908, #30200, #8367, .T. ) ;
#18724 = CARTESIAN_POINT ( 'NONE',  ( 5.687793815610356241, -6.974883619896809606, 21.50000000000000000 ) ) ;
#18725 = EDGE_CURVE ( 'NONE', #4539, #1968, #23263, .T. ) ;
#18726 = DIRECTION ( 'NONE',  ( -0.000000000000000000, -0.000000000000000000, -1.000000000000000000 ) ) ;
#18727 = PRESENTATION_LAYER_ASSIGNMENT (  '', '', ( #17719 ) ) ;
#18728 = CARTESIAN_POINT ( 'NONE',  ( -29.73688679209877606, 22.29461321502727600, 27.50000000000000355 ) ) ;
#18729 = DIRECTION ( 'NONE',  ( 1.000000000000000000, 0.000000000000000000, 0.000000000000000000 ) ) ;
#18730 = ORIENTED_EDGE ( 'NONE', *, *, #28232, .T. ) ;
#18731 = EDGE_CURVE ( 'NONE', #1458, #23298, #29107, .T. ) ;
#18732 = CARTESIAN_POINT ( 'NONE',  ( 1.159631224985658848, -19.96657546246603587, 7.272192800924335288 ) ) ;
#18733 = CARTESIAN_POINT ( 'NONE',  ( 14.46116907065692914, 13.81605838820131638, 20.15039051365863543 ) ) ;
#18734 = CARTESIAN_POINT ( 'NONE',  ( -8.999114229549592281, 0.1262659238205133538, 21.50000000000000000 ) ) ;
#18735 = EDGE_CURVE ( 'NONE', #16362, #26160, #12926, .T. ) ;
#18736 = EDGE_LOOP ( 'NONE', ( #9505, #23098, #1898 ) ) ;
#18737 = DIRECTION ( 'NONE',  ( -0.8932538319083086487, 0.4495526574063634095, 0.000000000000000000 ) ) ;
#18738 = VERTEX_POINT ( 'NONE', #30032 ) ;
#18739 = EDGE_CURVE ( 'NONE', #23193, #1001, #30475, .T. ) ;
#18740 = CARTESIAN_POINT ( 'NONE',  ( 16.14429390779611850, -5.555032456232104288, 6.131018562779544823 ) ) ;
#18741 = AXIS2_PLACEMENT_3D ( 'NONE', #7074, #16583, #9568 ) ;
#18742 = ORIENTED_EDGE ( 'NONE', *, *, #575, .F. ) ;
#18743 = CARTESIAN_POINT ( 'NONE',  ( 28.71210443682918978, -23.83196592705972705, 27.50000000000000000 ) ) ;
#18744 = CARTESIAN_POINT ( 'NONE',  ( 0.3552109633508242492, -3.484997970623515684, 9.000000000000003553 ) ) ;
#18745 = B_SPLINE_CURVE_WITH_KNOTS ( 'NONE', 3,
 ( #30677, #26019, #25707, #25867, #23968, #21012, #16353, #4336, #23363, #7294, #16807, #26322, #11668, #2615 ),
 .UNSPECIFIED., .F., .F.,
 ( 4, 2, 2, 2, 2, 2, 4 ),
 ( 0.008361799641757327456, 0.009326569779210591715, 0.01029133991666385597, 0.01222088019157035327, 0.01318565032902361579, 0.01415042046647687832, 0.01607996074138338602 ),
 .UNSPECIFIED. ) ;
#18746 = PLANE ( 'NONE',  #21607 ) ;
#18747 = CARTESIAN_POINT ( 'NONE',  ( 32.51029956715037628, -26.37762564238233765, -16.50000000000000355 ) ) ;
#18748 = CARTESIAN_POINT ( 'NONE',  ( -6.922783288613183039, 18.78247243577000347, 19.14333282897057842 ) ) ;
#18749=STYLED_ITEM('',(#30886),#2768);
#18750 = DIRECTION ( 'NONE',  ( -0.000000000000000000, -0.000000000000000000, 1.000000000000000000 ) ) ;
#18751 = CARTESIAN_POINT ( 'NONE',  ( 0.9307681286968572110, -9.436481611552755666, 1.500000000000001332 ) ) ;
#18752 = DIRECTION ( 'NONE',  ( -0.000000000000000000, 1.132880637372608986E-16, -1.000000000000000000 ) ) ;
#18753 = ORIENTED_EDGE ( 'NONE', *, *, #13534, .T. ) ;
#18754 = EDGE_CURVE ( 'NONE', #4645, #12148, #18299, .T. ) ;
#18755 = DIRECTION ( 'NONE',  ( 1.000000000000000000, 0.000000000000000000, 0.000000000000000000 ) ) ;
#18756 = EDGE_CURVE ( 'NONE', #4436, #26054, #9314, .T. ) ;
#18757 = CARTESIAN_POINT ( 'NONE',  ( 2.687479363073301819, 44.39187623479102740, -19.50000000000000355 ) ) ;
#18758 = CARTESIAN_POINT ( 'NONE',  ( -8.743977807160096205, -3.668292057955974350, 21.50000000000000000 ) ) ;
#18759 = ORIENTED_EDGE ( 'NONE', *, *, #18561, .F. ) ;
#18760 = DIRECTION ( 'NONE',  ( -1.000000000000000000, 0.000000000000000000, 0.000000000000000000 ) ) ;
#18761 = AXIS2_PLACEMENT_3D ( 'NONE', #19450, #17262, #12129 ) ;
#18762 = CARTESIAN_POINT ( 'NONE',  ( -17.69908921317806971, -9.351398086983023106, 18.73743063545763121 ) ) ;
#18763 = EDGE_CURVE ( 'NONE', #17664, #16485, #30247, .T. ) ;
#18764 = CARTESIAN_POINT ( 'NONE',  ( -13.37849590498012553, 10.56201291617987792, 20.34789198813115263 ) ) ;
#18765 = AXIS2_PLACEMENT_3D ( 'NONE', #10696, #6019, #29725 ) ;
#18766 = CARTESIAN_POINT ( 'NONE',  ( 4.336808689942017736E-16, 42.50000000000000000, -1.500000000000000000 ) ) ;
#18767 = VECTOR ( 'NONE', #3613, 1000.000000000000000 ) ;
#18768 = CARTESIAN_POINT ( 'NONE',  ( 20.65888525914559892, 38.75220717792412728, -19.50000000000000355 ) ) ;
#18769 = ORIENTED_EDGE ( 'NONE', *, *, #9731, .F. ) ;
#18770 = FACE_OUTER_BOUND ( 'NONE', #17179, .T. ) ;
#18771 = CARTESIAN_POINT ( 'NONE',  ( -9.062880100047301823, -0.6210184355499139830, -1.500000000000001776 ) ) ;
#18772 = CARTESIAN_POINT ( 'NONE',  ( 17.79366536559482626, -37.84673028964422059, 29.26143670286390019 ) ) ;
#18773 = PLANE ( 'NONE',  #21035 ) ;
#18774 = EDGE_LOOP ( 'NONE', ( #17227, #18438 ) ) ;
#18775 = CIRCLE ( 'NONE', #7819, 3.559164065751841743 ) ;
#18776 = DIRECTION ( 'NONE',  ( 1.000000000000000000, 0.000000000000000000, 0.000000000000000000 ) ) ;
#18777 = CARTESIAN_POINT ( 'NONE',  ( -3.914781618004753216, -8.197313248159932897, -1.500000000000002665 ) ) ;
#18778 = VERTEX_POINT ( 'NONE', #1949 ) ;
#18779 = AXIS2_PLACEMENT_3D ( 'NONE', #14282, #24270, #19134 ) ;
#18780 = ORIENTED_EDGE ( 'NONE', *, *, #29254, .F. ) ;
#18781 = DIRECTION ( 'NONE',  ( 1.000000000000000000, 0.000000000000000000, 0.000000000000000000 ) ) ;
#18782 = AXIS2_PLACEMENT_3D ( 'NONE', #26219, #19365, #19199 ) ;
#18783 = ORIENTED_EDGE ( 'NONE', *, *, #28430, .F. ) ;
#18784 = CARTESIAN_POINT ( 'NONE',  ( 0.4458717728788682555, -17.03078575579515785, 18.39701043959520987 ) ) ;
#18785 = CIRCLE ( 'NONE', #25262, 0.7500000000000006661 ) ;
#18786 = AXIS2_PLACEMENT_3D ( 'NONE', #9237, #28273, #6898 ) ;
#18787 = AXIS2_PLACEMENT_3D ( 'NONE', #5295, #14803, #2970 ) ;
#18788 = CARTESIAN_POINT ( 'NONE',  ( -4.163336342344337027E-14, 1.387778780781445676E-14, 67.49999999999997158 ) ) ;
#18789 = CARTESIAN_POINT ( 'NONE',  ( 1.653546806191835694, -16.99301016096993067, 18.82680253904184298 ) ) ;
#18790 = ORIENTED_EDGE ( 'NONE', *, *, #13948, .F. ) ;
#18791 = CARTESIAN_POINT ( 'NONE',  ( -23.17581250239728519, -34.50630206824673252, -1.499999999999999778 ) ) ;
#18792 = DIRECTION ( 'NONE',  ( 1.000000000000000000, 0.000000000000000000, 0.000000000000000000 ) ) ;
#18793 = DIRECTION ( 'NONE',  ( -0.000000000000000000, -0.000000000000000000, 1.000000000000000000 ) ) ;
#18794 = DIRECTION ( 'NONE',  ( 0.000000000000000000, 0.000000000000000000, 1.000000000000000000 ) ) ;
#18795 = ORIENTED_EDGE ( 'NONE', *, *, #29004, .T. ) ;
#18796 = EDGE_CURVE ( 'NONE', #14360, #28974, #11164, .T. ) ;
#18797 = VECTOR ( 'NONE', #9234, 1000.000000000000000 ) ;
#18798 = CIRCLE ( 'NONE', #1369, 15.00000000000000000 ) ;
#18799 = CARTESIAN_POINT ( 'NONE',  ( -39.52380524536133777, -7.028748154183623420, -6.500000000000000888 ) ) ;
#18800 = CARTESIAN_POINT ( 'NONE',  ( -13.29701885108704751, 10.65950381955433102, 18.34727598691067740 ) ) ;
#18801 = DIRECTION ( 'NONE',  ( -0.000000000000000000, -0.000000000000000000, -1.000000000000000000 ) ) ;
#18802 = CARTESIAN_POINT ( 'NONE',  ( 19.64177907938615064, 36.71644397333972876, 24.50000000000000000 ) ) ;
#18803 = CARTESIAN_POINT ( 'NONE',  ( -18.25684187146043058, -8.167166100028884657, 20.22277707861863050 ) ) ;
#18804 = CIRCLE ( 'NONE', #5350, 1.447898107987198646 ) ;
#18805 = FACE_OUTER_BOUND ( 'NONE', #3171, .T. ) ;
#18806 = CARTESIAN_POINT ( 'NONE',  ( 29.55332031600788767, -27.89853503085224773, -1.500000000000000000 ) ) ;
#18807 = VECTOR ( 'NONE', #24953, 1000.000000000000000 ) ;
#18808 = ORIENTED_EDGE ( 'NONE', *, *, #12401, .F. ) ;
#18809 = ORIENTED_EDGE ( 'NONE', *, *, #22020, .T. ) ;
#18810 = AXIS2_PLACEMENT_3D ( 'NONE', #25542, #26000, #4628 ) ;
#18811 = CARTESIAN_POINT ( 'NONE',  ( 32.81350286003733885, 7.028748154183637631, -6.500000000000000888 ) ) ;
#18812 = CARTESIAN_POINT ( 'NONE',  ( 4.336808689942017736E-16, 42.50000000000000000, -1.500000000000000000 ) ) ;
#18813 = CARTESIAN_POINT ( 'NONE',  ( -22.94541271838176044, 35.03073867844246081, -6.500000000000000888 ) ) ;
#18814 = ORIENTED_EDGE ( 'NONE', *, *, #2750, .F. ) ;
#18815 = AXIS2_PLACEMENT_3D ( 'NONE', #3795, #4242, #10816 ) ;
#18816 = CARTESIAN_POINT ( 'NONE',  ( 18.16954353748349860, -8.401983848419027012, 20.25336174263950184 ) ) ;
#18817 = CARTESIAN_POINT ( 'NONE',  ( 6.262709072525336929, 19.01302309856008321, 6.530762810602277924 ) ) ;
#18818 = AXIS2_PLACEMENT_3D ( 'NONE', #9614, #19124, #14446 ) ;
#18819 = VERTEX_POINT ( 'NONE', #25658 ) ;
#18820 = DIRECTION ( 'NONE',  ( -0.000000000000000000, -0.000000000000000000, -1.000000000000000000 ) ) ;
#18821 = VECTOR ( 'NONE', #13771, 1000.000000000000000 ) ;
#18822 = CARTESIAN_POINT ( 'NONE',  ( 14.40720023010961981, 13.89764844773314501, 7.366751648393900176 ) ) ;
#18823 = AXIS2_PLACEMENT_3D ( 'NONE', #18037, #27403, #10698 ) ;
#18824 = DIRECTION ( 'NONE',  ( -1.000000000000000000, 0.000000000000000000, 0.000000000000000000 ) ) ;
#18825 = CARTESIAN_POINT ( 'NONE',  ( -18.45311310706550856, 32.73271211070382236, 37.49999999995343103 ) ) ;
#18826 = EDGE_LOOP ( 'NONE', ( #185, #13148 ) ) ;
#18827 = DIRECTION ( 'NONE',  ( -1.982541115402065356E-16, 0.000000000000000000, 1.000000000000000000 ) ) ;
#18828 = DIRECTION ( 'NONE',  ( -0.000000000000000000, 1.132880637372608986E-16, -1.000000000000000000 ) ) ;
#18829 = CARTESIAN_POINT ( 'NONE',  ( -15.25895845836713605, 12.92986402562788406, 7.652108011868849147 ) ) ;
#18830 = VECTOR ( 'NONE', #9921, 1000.000000000000000 ) ;
#18831 = VERTEX_POINT ( 'NONE', #22682 ) ;
#18832 = AXIS2_PLACEMENT_3D ( 'NONE', #23596, #28759, #14235 ) ;
#18833 = CARTESIAN_POINT ( 'NONE',  ( -15.51938817160315232, -6.998174447281578558, 7.176035686813569292 ) ) ;
#18834 = CARTESIAN_POINT ( 'NONE',  ( 16.87927834490895052, 2.194149605794880831, 19.41069149716888020 ) ) ;
#18835 = CARTESIAN_POINT ( 'NONE',  ( 25.07174449839132890, -6.739288358966160963, 44.79593483594005221 ) ) ;
#18836 = DIRECTION ( 'NONE',  ( -0.000000000000000000, -0.000000000000000000, 1.000000000000000000 ) ) ;
#18837 = CARTESIAN_POINT ( 'NONE',  ( 0.05528831664089196157, -17.02727625121208632, 7.359006845440219102 ) ) ;
#18838 = ADVANCED_FACE ( 'NONE', ( #25512 ), #25185, .T. ) ;
#18839 = CYLINDRICAL_SURFACE ( 'NONE', #25714, 0.7441270634457181066 ) ;
#18840 = CARTESIAN_POINT ( 'NONE',  ( 0.000000000000000000, 0.000000000000000000, 21.50000000000000000 ) ) ;
#18841 = DIRECTION ( 'NONE',  ( -0.000000000000000000, -0.000000000000000000, 1.000000000000000000 ) ) ;
#18842 = DIRECTION ( 'NONE',  ( -0.000000000000000000, -0.000000000000000000, 1.000000000000000000 ) ) ;
#18843 = EDGE_LOOP ( 'NONE', ( #13170, #6002, #448, #29549 ) ) ;
#18844 = CIRCLE ( 'NONE', #29303, 37.99999999999933920 ) ;
#18845 = CARTESIAN_POINT ( 'NONE',  ( -5.800828033475949219, 16.03801949186916431, 5.653604225791663218 ) ) ;
#18846 = CARTESIAN_POINT ( 'NONE',  ( 0.000000000000000000, 39.50000000000000000, 34.80090346875809360 ) ) ;
#18847 = AXIS2_PLACEMENT_3D ( 'NONE', #26392, #18606, #28118 ) ;
#18848 = ORIENTED_EDGE ( 'NONE', *, *, #757, .F. ) ;
#18849 = ORIENTED_EDGE ( 'NONE', *, *, #1790, .F. ) ;
#18850 = DIRECTION ( 'NONE',  ( 0.000000000000000000, 0.000000000000000000, 1.000000000000000000 ) ) ;
#18851 = DIRECTION ( 'NONE',  ( -0.000000000000000000, -0.000000000000000000, 1.000000000000000000 ) ) ;
#18852 = ORIENTED_EDGE ( 'NONE', *, *, #29443, .F. ) ;
#18853 = AXIS2_PLACEMENT_3D ( 'NONE', #30470, #11463, #27849 ) ;
#18854 = LINE ( 'NONE', #21158, #6688 ) ;
#18855 = CARTESIAN_POINT ( 'NONE',  ( -32.28307784207223108, 8.475829241206282560, 41.62281023987520001 ) ) ;
#18856 = ORIENTED_EDGE ( 'NONE', *, *, #23411, .T. ) ;
#18857 = DIRECTION ( 'NONE',  ( 1.000000000000000000, 0.000000000000000000, 0.000000000000000000 ) ) ;
#18858 = CYLINDRICAL_SURFACE ( 'NONE', #15976, 0.7500000000000006661 ) ;
#18859 = VERTEX_POINT ( 'NONE', #18033 ) ;
#18860 = DIRECTION ( 'NONE',  ( -1.000000000000000000, -0.000000000000000000, -0.000000000000000000 ) ) ;
#18861 = ORIENTED_EDGE ( 'NONE', *, *, #25566, .T. ) ;
#18862 = ORIENTED_EDGE ( 'NONE', *, *, #2938, .T. ) ;
#18863 = AXIS2_PLACEMENT_3D ( 'NONE', #11518, #9167, #18680 ) ;
#18864 = AXIS2_PLACEMENT_3D ( 'NONE', #15618, #24668, #5966 ) ;
#18865 = EDGE_LOOP ( 'NONE', ( #28207, #28678, #11032, #21166 ) ) ;
#18866 = ADVANCED_FACE ( 'NONE', ( #13196 ), #6626, .F. ) ;
#18867 = DIRECTION ( 'NONE',  ( 1.000000000000000000, 0.000000000000000000, 0.000000000000000000 ) ) ;
#18868 = CARTESIAN_POINT ( 'NONE',  ( -0.2028048457280972328, -17.02068360090513721, 19.08155846658119259 ) ) ;
#18869 = VECTOR ( 'NONE', #2259, 1000.000000000000000 ) ;
#18870 = CARTESIAN_POINT ( 'NONE',  ( 0.4236634240584232769, -20.01342612130734722, 7.652108011868850035 ) ) ;
#18871 = LINE ( 'NONE', #16978, #3586 ) ;
#18872 = CARTESIAN_POINT ( 'NONE',  ( -23.26375789455195431, 12.37328455203049593, 48.65081625091716688 ) ) ;
#18873 = DIRECTION ( 'NONE',  ( -0.000000000000000000, -0.000000000000000000, 1.000000000000000000 ) ) ;
#18874 = ORIENTED_EDGE ( 'NONE', *, *, #25932, .F. ) ;
#18875 = EDGE_CURVE ( 'NONE', #15172, #4676, #2338, .T. ) ;
#18876 = PLANE ( 'NONE',  #22209 ) ;
#18877 = DIRECTION ( 'NONE',  ( -0.4495526574063634095, -0.8932538319083086487, 0.000000000000000000 ) ) ;
#18878 = DIRECTION ( 'NONE',  ( 1.000000000000000000, 0.000000000000000000, 0.000000000000000000 ) ) ;
#18879 = DIRECTION ( 'NONE',  ( -0.000000000000000000, -0.000000000000000000, -1.000000000000000000 ) ) ;
#18880 = ORIENTED_EDGE ( 'NONE', *, *, #6578, .F. ) ;
#18881 =( BOUNDED_SURFACE ( )  B_SPLINE_SURFACE ( 3, 1, ( 
 ( #13958, #2412 ),
 ( #23453, #28316 ),
 ( #21108, #25965 ),
 ( #4592, #23602 ) ),
 .UNSPECIFIED., .F., .F., .T. ) 
 B_SPLINE_SURFACE_WITH_KNOTS ( ( 4, 4 ),
 ( 2, 2 ),
 ( 0.000000000000000000, 1.000000000000000000 ),
 ( 0.000000000000000000, 1.000000000000000000 ),
 .UNSPECIFIED. ) 
 GEOMETRIC_REPRESENTATION_ITEM ( )  RATIONAL_B_SPLINE_SURFACE ( (
 ( 1.000000000000000000, 1.000000000000000000),
 ( 0.9908525036704132205, 0.9908525036704132205),
 ( 0.9908525036704132205, 0.9908525036704132205),
 ( 1.000000000000000000, 1.000000000000000000) ) ) 
 REPRESENTATION_ITEM ( '' )  SURFACE ( )  );
#18882 = EDGE_LOOP ( 'NONE', ( #3944, #13504, #23093, #3422 ) ) ;
#18883 = DIRECTION ( 'NONE',  ( -0.000000000000000000, -0.000000000000000000, -1.000000000000000000 ) ) ;
#18884 = CARTESIAN_POINT ( 'NONE',  ( 1.000000000000008438, 19.97498435543819184, 24.50000000000000000 ) ) ;
#18885 = CARTESIAN_POINT ( 'NONE',  ( -40.05104235265675783, 2.353288714454549790, -6.500000000000000888 ) ) ;
#18886 = PRODUCT_DEFINITION_SHAPE ( 'NONE', 'NONE',  #2093 ) ;
#18887 = LINE ( 'NONE', #28398, #14322 ) ;
#18888 = CARTESIAN_POINT ( 'NONE',  ( 4.340342926364955112, 8.430595340551274575, 13.00000000000000178 ) ) ;
#18889 = AXIS2_PLACEMENT_3D ( 'NONE', #13673, #13817, #23157 ) ;
#18890 = CARTESIAN_POINT ( 'NONE',  ( -33.27395842691333172, 15.08718781055274860, 27.50000000000000355 ) ) ;
#18891 = EDGE_CURVE ( 'NONE', #14452, #29313, #28540, .T. ) ;
#18892 = CARTESIAN_POINT ( 'NONE',  ( 32.81350286003733885, -7.028748154183637631, -6.500000000000000888 ) ) ;
#18893 = VERTEX_POINT ( 'NONE', #16911 ) ;
#18894 = CARTESIAN_POINT ( 'NONE',  ( -19.95825857724417318, 1.540497788607360752, 6.341840715582230281 ) ) ;
#18895 = VECTOR ( 'NONE', #30399, 1000.000000000000000 ) ;
#18896 = FACE_OUTER_BOUND ( 'NONE', #1418, .T. ) ;
#18897 = CARTESIAN_POINT ( 'NONE',  ( 39.99999999999998579, 67.32050807568877815, 12.49999999999999112 ) ) ;
#18898 = VERTEX_POINT ( 'NONE', #69 ) ;
#18899 = CARTESIAN_POINT ( 'NONE',  ( -9.824744466605366711, -8.513189541288717521, 1.500000000000001332 ) ) ;
#18900 = EDGE_LOOP ( 'NONE', ( #16699, #25441, #27718, #8589 ) ) ;
#18901 = CARTESIAN_POINT ( 'NONE',  ( -1.722266914199011234, -42.46879315525252707, 28.84242400037395626 ) ) ;
#18902 = AXIS2_PLACEMENT_3D ( 'NONE', #7355, #24167, #22149 ) ;
#18903 = CARTESIAN_POINT ( 'NONE',  ( 0.3518703668723787148, -19.99690444156084723, 7.652108011868850035 ) ) ;
#18904 = VERTEX_POINT ( 'NONE', #11761 ) ;
#18905 = CARTESIAN_POINT ( 'NONE',  ( 23.04694076046884987, -30.34744638473161160, 27.50000000000000355 ) ) ;
#18906 = EDGE_CURVE ( 'NONE', #25162, #12583, #7087, .T. ) ;
#18907 = FACE_BOUND ( 'NONE', #83, .T. ) ;
#18908 = EDGE_CURVE ( 'NONE', #27029, #26519, #6815, .T. ) ;
#18909 = B_SPLINE_CURVE_WITH_KNOTS ( 'NONE', 3,
 ( #25969, #28320, #23765, #2248, #23458, #23153, #25665, #6946, #4454, #11945, #20960, #11769, #2418, #11621, #11476, #16455, #30796, #30484, #18800, #21112 ),
 .UNSPECIFIED., .F., .F.,
 ( 4, 2, 2, 2, 2, 2, 2, 2, 2, 4 ),
 ( 0.000000000000000000, 0.06250000000000177636, 0.1250000000000035527, 0.1875000000000053291, 0.2187500000000054678, 0.2500000000000056066, 0.3125000000000042188, 0.3750000000000028311, 0.4375000000000014433, 0.5000000000000000000 ),
 .UNSPECIFIED. ) ;
#18910 = CARTESIAN_POINT ( 'NONE',  ( -8.884323311075783991, -1.438332125858144295, -3.621320343559650379 ) ) ;
#18911 = CARTESIAN_POINT ( 'NONE',  ( -18.44586851731391519, -7.729974993529599381, 6.913388067999409081 ) ) ;
#18912 = DIRECTION ( 'NONE',  ( -0.000000000000000000, -0.000000000000000000, -1.000000000000000000 ) ) ;
#18913 = DIRECTION ( 'NONE',  ( 0.7557495743542581579, 0.6548607339452852116, -0.000000000000000000 ) ) ;
#18914 = CARTESIAN_POINT ( 'NONE',  ( 69.99999999999998579, -50.00000000000000000, -92.50000000000000000 ) ) ;
#18915 = ORIENTED_EDGE ( 'NONE', *, *, #28094, .T. ) ;
#18916 = EDGE_CURVE ( 'NONE', #16863, #2233, #17788, .T. ) ;
#18917 = CIRCLE ( 'NONE', #4970, 10.00000000000003730 ) ;
#18918 = CARTESIAN_POINT ( 'NONE',  ( 25.19442432473618254, -35.44676296258426618, -19.50000000000000355 ) ) ;
#18919 = DIRECTION ( 'NONE',  ( 1.000000000000000000, -5.780230957810361426E-15, 0.000000000000000000 ) ) ;
#18920 = EDGE_LOOP ( 'NONE', ( #23267, #23963 ) ) ;
#18921 = EDGE_CURVE ( 'NONE', #15693, #8747, #12305, .T. ) ;
#18922 = CARTESIAN_POINT ( 'NONE',  ( -6.812559277181930106, 5.881244434206302607, -3.621320343559650379 ) ) ;
#18923 = CARTESIAN_POINT ( 'NONE',  ( -17.91516185886248635, -8.931344358737691280, 20.29915277494337644 ) ) ;
#18925 = EDGE_CURVE ( 'NONE', #26229, #19866, #16743, .T. ) ;
#18924 = CARTESIAN_POINT ( 'NONE',  ( 22.49999999999992184, 1.387778780781445676E-14, 52.50000000000000000 ) ) ;
#18926 = CARTESIAN_POINT ( 'NONE',  ( 37.16608720827707657, -65.00000000000000000, 57.49999999999999289 ) ) ;
#18927 = COLOUR_RGB ( '',0.7921568627450980005, 0.8196078431372548767, 0.9333333333333333481 ) ;
#18928 = PLANE ( 'NONE',  #18597 ) ;
#18929 = VERTEX_POINT ( 'NONE', #21726 ) ;
#18930 = CARTESIAN_POINT ( 'NONE',  ( -0.2664633505552017056, -19.99844781589862563, 20.14992337338002670 ) ) ;
#18931 = EDGE_CURVE ( 'NONE', #16453, #8571, #28934, .T. ) ;
#18932 = CARTESIAN_POINT ( 'NONE',  ( -52.16608720827707657, -36.86186943028246787, 12.49999999999999112 ) ) ;
#18933 = CARTESIAN_POINT ( 'NONE',  ( 39.00152643798587349, 0.5466461374812251472, 35.07981065047974312 ) ) ;
#18934 = CARTESIAN_POINT ( 'NONE',  ( -6.809999484610175458, 18.80496293131999863, 7.161525567826885208 ) ) ;
#18935 = VERTEX_POINT ( 'NONE', #4900 ) ;
#18936 = DIRECTION ( 'NONE',  ( 0.000000000000000000, 1.132880637372608986E-16, -1.000000000000000000 ) ) ;
#18937 = CARTESIAN_POINT ( 'NONE',  ( -10.11202017158466759, 41.14070756921185534, -1.500000000000000000 ) ) ;
#18938 = FACE_BOUND ( 'NONE', #10834, .T. ) ;
#18939 = ORIENTED_EDGE ( 'NONE', *, *, #27178, .T. ) ;
#18940 = VERTEX_POINT ( 'NONE', #5056 ) ;
#18941 = DIRECTION ( 'NONE',  ( -0.000000000000000000, 0.000000000000000000, 1.000000000000000000 ) ) ;
#18942 = AXIS2_PLACEMENT_3D ( 'NONE', #1289, #25139, #17513 ) ;
#18943 = ORIENTED_EDGE ( 'NONE', *, *, #9181, .F. ) ;
#18944 = EDGE_LOOP ( 'NONE', ( #25184, #1778, #16663, #21745 ) ) ;
#18945 = CARTESIAN_POINT ( 'NONE',  ( 0.6650193650332599793, -17.02944248263315785, 20.34789198813115263 ) ) ;
#18946 = EDGE_CURVE ( 'NONE', #24152, #7862, #21756, .T. ) ;
#18947 = EDGE_CURVE ( 'NONE', #24164, #30839, #29325, .T. ) ;
#18948 = CARTESIAN_POINT ( 'NONE',  ( -10.06548534245862747, -17.30301317789299631, 7.500147780736496017 ) ) ;
#18949 = CARTESIAN_POINT ( 'NONE',  ( -33.31178504393444229, 22.11114403104716430, 17.99999999999999645 ) ) ;
#18950 = CARTESIAN_POINT ( 'NONE',  ( 0.9949940796826611811, -19.99317329078838057, 18.56793045041961321 ) ) ;
#18951 = ORIENTED_EDGE ( 'NONE', *, *, #27142, .T. ) ;
#18952 = EDGE_CURVE ( 'NONE', #509, #25203, #20768, .T. ) ;
#18953 = CARTESIAN_POINT ( 'NONE',  ( 12.56641067637329812, 40.32935944495179115, -1.500000000000003997 ) ) ;
#18954 = DIRECTION ( 'NONE',  ( -0.000000000000000000, -0.000000000000000000, -1.000000000000000000 ) ) ;
#18955 = CARTESIAN_POINT ( 'NONE',  ( 1.342668813586976206, -19.95494644892924185, 19.08830981656263859 ) ) ;
#18956 = DIRECTION ( 'NONE',  ( -0.000000000000000000, -0.000000000000000000, 1.000000000000000000 ) ) ;
#18957 = ORIENTED_EDGE ( 'NONE', *, *, #22370, .T. ) ;
#18958 = DIRECTION ( 'NONE',  ( -0.000000000000000000, 0.000000000000000000, -1.000000000000000000 ) ) ;
#18959 = CYLINDRICAL_SURFACE ( 'NONE', #16325, 6.000000000000005329 ) ;
#18960 = CARTESIAN_POINT ( 'NONE',  ( 26.80246859415415273, -7.028748154183637631, -1.499999999999999556 ) ) ;
#18961 = DIRECTION ( 'NONE',  ( 0.000000000000000000, 0.000000000000000000, 1.000000000000000000 ) ) ;
#18962 = CARTESIAN_POINT ( 'NONE',  ( -18.30120037456298121, -8.066899270990504078, 18.54479204710284890 ) ) ;
#18963 = EDGE_CURVE ( 'NONE', #4466, #8993, #17888, .T. ) ;
#18964 = CARTESIAN_POINT ( 'NONE',  ( -23.20393738267338790, 0.000000000000000000, -1.500000000000000000 ) ) ;
#18965 = CARTESIAN_POINT ( 'NONE',  ( 33.26787633654602416, -9.290711110048579968, 36.21660691973271895 ) ) ;
#18966 = ORIENTED_EDGE ( 'NONE', *, *, #17557, .F. ) ;
#18967 = ORIENTED_EDGE ( 'NONE', *, *, #17100, .F. ) ;
#18968 = DIRECTION ( 'NONE',  ( 0.000000000000000000, 0.000000000000000000, -1.000000000000000000 ) ) ;
#18969 = CARTESIAN_POINT ( 'NONE',  ( 2.552544031601107211, 42.49999999998228617, -1.500000000000000000 ) ) ;
#18970 = DIRECTION ( 'NONE',  ( -0.000000000000000000, -0.000000000000000000, -1.000000000000000000 ) ) ;
#18971 = CARTESIAN_POINT ( 'NONE',  ( 11.91611018267552247, -16.06265986513583854, 19.61564845152809156 ) ) ;
#18972 = ORIENTED_EDGE ( 'NONE', *, *, #12625, .F. ) ;
#18973 = CARTESIAN_POINT ( 'NONE',  ( 0.000000000000000000, 0.000000000000000000, 0.000000000000000000 ) ) ;
#18974 = CARTESIAN_POINT ( 'NONE',  ( 17.92822150912323309, -8.904799031605451276, 19.22654678686458141 ) ) ;
#18975 = CARTESIAN_POINT ( 'NONE',  ( 5.624045005368200734, 19.21181948662072969, 5.701226463332907279 ) ) ;
#18976 = EDGE_CURVE ( 'NONE', #4502, #8522, #11610, .T. ) ;
#18977 = ORIENTED_EDGE ( 'NONE', *, *, #15917, .T. ) ;
#18978 = CARTESIAN_POINT ( 'NONE',  ( 14.89737979318874572, 13.37085219355980570, 7.652108011868850035 ) ) ;
#18979 = EDGE_CURVE ( 'NONE', #27312, #12499, #7343, .T. ) ;
#18980 = CARTESIAN_POINT ( 'NONE',  ( -23.47668842614531215, 34.05319493990059954, 29.63203809737341743 ) ) ;
#18981 = ORIENTED_EDGE ( 'NONE', *, *, #11311, .F. ) ;
#18982 = CARTESIAN_POINT ( 'NONE',  ( 24.44496207165490276, 7.595930209050162141, 45.15942333309104129 ) ) ;
#18983 = VECTOR ( 'NONE', #28417, 1000.000000000000000 ) ;
#18984 = CARTESIAN_POINT ( 'NONE',  ( 0.000000000000000000, 1.604273173167211147E-31, -87.50000000000000000 ) ) ;
#18985 = AXIS2_PLACEMENT_3D ( 'NONE', #3983, #18333, #27847 ) ;
#18986 = CARTESIAN_POINT ( 'NONE',  ( -4.163336342344337027E-14, 1.387778780781445676E-14, 62.49999999999999289 ) ) ;
#18987 = EDGE_LOOP ( 'NONE', ( #20258, #6673 ) ) ;
#18988 = CARTESIAN_POINT ( 'NONE',  ( -15.56851150445305443, -6.881932713941046664, 6.864725433338323413 ) ) ;
#18989 = DIRECTION ( 'NONE',  ( 1.000000000000000000, 0.000000000000000000, 0.000000000000000000 ) ) ;
#18990 = FACE_OUTER_BOUND ( 'NONE', #25309, .T. ) ;
#18991 = CARTESIAN_POINT ( 'NONE',  ( -0.2073672225646047973, -17.02047435233534145, 6.864725433338323413 ) ) ;
#18992 = DIRECTION ( 'NONE',  ( -1.000000000000000000, 0.000000000000000000, 0.000000000000000000 ) ) ;
#18993 = DIRECTION ( 'NONE',  ( 0.000000000000000000, 0.000000000000000000, -1.000000000000000000 ) ) ;
#18994 = CARTESIAN_POINT ( 'NONE',  ( 32.98805937973593672, -80.00000000000000000, 8.000000000000003553 ) ) ;
#18995 = LINE ( 'NONE', #6984, #15885 ) ;
#18996 = VERTEX_POINT ( 'NONE', #1463 ) ;
#18997 = DIRECTION ( 'NONE',  ( 0.000000000000000000, 0.000000000000000000, -1.000000000000000000 ) ) ;
#18998 = DIRECTION ( 'NONE',  ( 1.000000000000000000, 0.000000000000000000, 0.000000000000000000 ) ) ;
#18999 = ORIENTED_EDGE ( 'NONE', *, *, #18352, .F. ) ;
#19000 = ORIENTED_EDGE ( 'NONE', *, *, #16965, .T. ) ;
#19001 = CARTESIAN_POINT ( 'NONE',  ( -15.97601187733368278, 12.03191775062556879, 6.523620417364449864 ) ) ;
#19002 = DIRECTION ( 'NONE',  ( 1.000000000000000000, 0.000000000000000000, 0.000000000000000000 ) ) ;
#19003 = EDGE_LOOP ( 'NONE', ( #13871, #24203, #3477, #27255 ) ) ;
#19004 = CARTESIAN_POINT ( 'NONE',  ( 14.89738168138696217, 13.37085340703111669, 20.34789198813115263 ) ) ;
#19005 = PLANE ( 'NONE',  #17922 ) ;
#19006 = VERTEX_POINT ( 'NONE', #6122 ) ;
#19007 = CARTESIAN_POINT ( 'NONE',  ( 16.17688602565675282, -5.469326772727303165, 19.03762469184452755 ) ) ;
#19008 = CARTESIAN_POINT ( 'NONE',  ( 16.56029649016583605, 4.170884463584000557, 19.58863275299554019 ) ) ;
#19009 = EDGE_CURVE ( 'NONE', #16284, #13582, #30137, .T. ) ;
#19010 = DIRECTION ( 'NONE',  ( 1.000000000000000000, 0.000000000000000000, 0.000000000000000000 ) ) ;
#19011 = EDGE_CURVE ( 'NONE', #23254, #19951, #11122, .T. ) ;
#19012 = ORIENTED_EDGE ( 'NONE', *, *, #25792, .T. ) ;
#19013 = EDGE_CURVE ( 'NONE', #17197, #1665, #14786, .T. ) ;
#19014 = CARTESIAN_POINT ( 'NONE',  ( 15.40017468080184315, -7.251222802971749815, 19.60617949693493500 ) ) ;
#19015 = ORIENTED_EDGE ( 'NONE', *, *, #3131, .T. ) ;
#19016 = VECTOR ( 'NONE', #30521, 1000.000000000000000 ) ;
#19017 = ORIENTED_EDGE ( 'NONE', *, *, #8613, .F. ) ;
#19018 = CARTESIAN_POINT ( 'NONE',  ( -4.163336342344337027E-14, 1.387778780781445676E-14, 24.50000000000000000 ) ) ;
#19019 = CARTESIAN_POINT ( 'NONE',  ( 8.099999999999999645, 7.347880794884121708E-16, -6.000000000000001776 ) ) ;
#19020 = AXIS2_PLACEMENT_3D ( 'NONE', #18984, #18828, #17092 ) ;
#19021 = CARTESIAN_POINT ( 'NONE',  ( 1.153863525602934592, -19.98436899483066753, 6.041646659195333058 ) ) ;
#19022 = CARTESIAN_POINT ( 'NONE',  ( -15.00088867516242175, -39.32768935608851990, 29.12215979044223246 ) ) ;
#19023 = CARTESIAN_POINT ( 'NONE',  ( 1.762690206876408761, -16.98588469933353196, 19.08844262864050023 ) ) ;
#19024 = ORIENTED_EDGE ( 'NONE', *, *, #7482, .F. ) ;
#19025 = CARTESIAN_POINT ( 'NONE',  ( 10.44014025173321514, -17.07989312292649942, 7.272049892295485485 ) ) ;
#19026 = CARTESIAN_POINT ( 'NONE',  ( 4.390207617113956573, -7.856594496258208160, 21.50000000000000000 ) ) ;
#19027 = DIRECTION ( 'NONE',  ( -0.000000000000000000, -0.000000000000000000, 1.000000000000000000 ) ) ;
#19028 = ORIENTED_EDGE ( 'NONE', *, *, #2958, .T. ) ;
#19029 = ORIENTED_EDGE ( 'NONE', *, *, #3488, .F. ) ;
#19030 = CARTESIAN_POINT ( 'NONE',  ( -39.70095622561521509, -7.028748154183642072, -13.16666434783603989 ) ) ;
#19031 = DIRECTION ( 'NONE',  ( 0.000000000000000000, 0.000000000000000000, 1.000000000000000000 ) ) ;
#19032 = AXIS2_PLACEMENT_3D ( 'NONE', #2217, #23726, #23425 ) ;
#19033 = CARTESIAN_POINT ( 'NONE',  ( -6.187077094091591789, 11.47693674426096955, 1.500000000000001332 ) ) ;
#19034 = DIRECTION ( 'NONE',  ( -0.000000000000000000, -0.000000000000000000, 1.000000000000000000 ) ) ;
#19035 = DIRECTION ( 'NONE',  ( -0.000000000000000000, -0.000000000000000000, -1.000000000000000000 ) ) ;
#19036 = CARTESIAN_POINT ( 'NONE',  ( -32.57644024395770543, 16.81967142788571579, 27.50000000000000000 ) ) ;
#19037 = CARTESIAN_POINT ( 'NONE',  ( 0.09318607064769421355, 1.767053008364807942, -9.000000000000003553 ) ) ;
#19038 = EDGE_LOOP ( 'NONE', ( #2757, #4403, #6121, #14368 ) ) ;
#19039 = CARTESIAN_POINT ( 'NONE',  ( -19.53847887038948272, -33.17743341422470849, 34.50000000000000711 ) ) ;
#19040 = CARTESIAN_POINT ( 'NONE',  ( 14.33033395197103843, 13.95171706641511378, 19.96797677718662811 ) ) ;
#19041 = CARTESIAN_POINT ( 'NONE',  ( -37.99999999999999289, 70.00000000000000000, -75.50000000000000000 ) ) ;
#19042 = VERTEX_POINT ( 'NONE', #13627 ) ;
#19043 = DIRECTION ( 'NONE',  ( 0.000000000000000000, 0.000000000000000000, 1.000000000000000000 ) ) ;
#19044 = VERTEX_POINT ( 'NONE', #10974 ) ;
#19045 = CARTESIAN_POINT ( 'NONE',  ( -5.127072262013854242, -42.13114360820154047, 28.87158698979397897 ) ) ;
#19046 = CARTESIAN_POINT ( 'NONE',  ( -18.48743143136275435, 39.23974440348072079, -16.50000000000000355 ) ) ;
#19047 = ORIENTED_EDGE ( 'NONE', *, *, #7080, .T. ) ;
#19048 = CARTESIAN_POINT ( 'NONE',  ( 32.55221183676798091, 16.87602028573894231, 27.50000000000000711 ) ) ;
#19049 = CARTESIAN_POINT ( 'NONE',  ( 9.149370483914699648, 49.15727498498932135, -43.10339609117139759 ) ) ;
#19050 = AXIS2_PLACEMENT_3D ( 'NONE', #9782, #6823, #19146 ) ;
#19051 = CARTESIAN_POINT ( 'NONE',  ( 10.67036453489834003, -13.33339184394925070, 19.61324152429827095 ) ) ;
#19052 = CARTESIAN_POINT ( 'NONE',  ( -18.15587082468813307, -8.389233089038013347, 7.626647697317579855 ) ) ;
#19053 = CARTESIAN_POINT ( 'NONE',  ( -0.9621688436940065703, -9.033033306777454641, 21.50000000000000000 ) ) ;
#19054 = CARTESIAN_POINT ( 'NONE',  ( 10.68225562352957247, -16.90870462272444286, 20.22277707861861984 ) ) ;
#19055 = ORIENTED_EDGE ( 'NONE', *, *, #16782, .F. ) ;
#19056 = FACE_OUTER_BOUND ( 'NONE', #23057, .T. ) ;
#19057 = CARTESIAN_POINT ( 'NONE',  ( 37.98493438989863336, -11.12428508576153341, -1.500000000000000000 ) ) ;
#19058 = CARTESIAN_POINT ( 'NONE',  ( 39.52380524535562500, 7.028748154183637631, -11.49999999999999645 ) ) ;
#19059 = VERTEX_POINT ( 'NONE', #8491 ) ;
#19060 = LINE ( 'NONE', #26399, #17545 ) ;
#19061 = CARTESIAN_POINT ( 'NONE',  ( -17.59999711780629994, -9.536506973003673338, 19.47783254395485031 ) ) ;
#19062 = CARTESIAN_POINT ( 'NONE',  ( -3.515970705488605130, -17.06554576617236307, -1.500000000000000000 ) ) ;
#19063 = DIRECTION ( 'NONE',  ( 0.000000000000000000, 1.000000000000000000, 0.000000000000000000 ) ) ;
#19064 = CARTESIAN_POINT ( 'NONE',  ( -2.931009552726339784, -14.22630671667915969, -1.500000000000000000 ) ) ;
#19065 = ORIENTED_EDGE ( 'NONE', *, *, #14946, .T. ) ;
#19066 = AXIS2_PLACEMENT_3D ( 'NONE', #26589, #1837, #9018 ) ;
#19067 = CARTESIAN_POINT ( 'NONE',  ( 6.974883619896790954, 5.687793815610376669, 21.50000000000000000 ) ) ;
#19068 = EDGE_CURVE ( 'NONE', #26638, #7923, #27767, .T. ) ;
#19069 = CARTESIAN_POINT ( 'NONE',  ( 38.93844114562506320, 2.472344433271586706, 32.21256721326712835 ) ) ;
#19071 = AXIS2_PLACEMENT_3D ( 'NONE', #22210, #12712, #845 ) ;
#19070 = CARTESIAN_POINT ( 'NONE',  ( 0.000000000000000000, 0.000000000000000000, -1.500000000000000000 ) ) ;
#19072 = ORIENTED_EDGE ( 'NONE', *, *, #18151, .F. ) ;
#19073 = DIRECTION ( 'NONE',  ( 1.000000000000000000, 0.000000000000000000, 0.000000000000000000 ) ) ;
#19074 = VERTEX_POINT ( 'NONE', #18293 ) ;
#19075 = EDGE_CURVE ( 'NONE', #20004, #26411, #8822, .T. ) ;
#19076 = DIRECTION ( 'NONE',  ( 0.000000000000000000, 0.000000000000000000, -1.000000000000000000 ) ) ;
#19077 = CARTESIAN_POINT ( 'NONE',  ( -28.34828976096172326, 29.18752572968383063, 1.500000000000000000 ) ) ;
#19078 = VERTEX_POINT ( 'NONE', #25146 ) ;
#19079 = EDGE_CURVE ( 'NONE', #25672, #25827, #25563, .T. ) ;
#19080 = ORIENTED_EDGE ( 'NONE', *, *, #13004, .T. ) ;
#19081 = CARTESIAN_POINT ( 'NONE',  ( -24.03057240117691862, 26.57182937991348481, -1.500000000000001332 ) ) ;
#19082 = EDGE_CURVE ( 'NONE', #6597, #19542, #30270, .T. ) ;
#19083 = EDGE_LOOP ( 'NONE', ( #29206, #7880, #3046, #646, #4386, #21835, #17652, #2022, #29167 ) ) ;
#19084 = ORIENTED_EDGE ( 'NONE', *, *, #3095, .T. ) ;
#19085 = CARTESIAN_POINT ( 'NONE',  ( -24.44496207165490276, -7.595930209050158588, 45.15942333309111234 ) ) ;
#19086 = EDGE_CURVE ( 'NONE', #11240, #17664, #18329, .T. ) ;
#19087 = CARTESIAN_POINT ( 'NONE',  ( -8.266165397079792143, -14.91833037834293840, 7.603368798681074736 ) ) ;
#19088 = CARTESIAN_POINT ( 'NONE',  ( -34.22142550507209080, 20.39476870213973214, 17.85497485759970004 ) ) ;
#19089 = EDGE_CURVE ( 'NONE', #9030, #9450, #11430, .T. ) ;
#19090 = CARTESIAN_POINT ( 'NONE',  ( 0.7788148826605766351, -17.02744010918315354, 20.34789198813115263 ) ) ;
#19091 = ORIENTED_EDGE ( 'NONE', *, *, #25952, .T. ) ;
#19092 = CARTESIAN_POINT ( 'NONE',  ( 33.13218612630368654, 7.028748154183637631, -1.942616967526160643 ) ) ;
#19093 = EDGE_CURVE ( 'NONE', #3168, #26303, #3634, .T. ) ;
#19094 = VECTOR ( 'NONE', #19958, 1000.000000000000000 ) ;
#19095 = CARTESIAN_POINT ( 'NONE',  ( 0.8038475772933700858, -5.196152422706651564, 9.000000000000001776 ) ) ;
#19096 = CARTESIAN_POINT ( 'NONE',  ( 0.6154569680869020898, -19.99089747819055418, 20.32200205377525037 ) ) ;
#19097 = CARTESIAN_POINT ( 'NONE',  ( -4.163336342344337027E-14, 1.387778780781445676E-14, 24.50000000000000000 ) ) ;
#19098 = ORIENTED_EDGE ( 'NONE', *, *, #13501, .F. ) ;
#19099 = AXIS2_PLACEMENT_3D ( 'NONE', #13743, #4375, #21365 ) ;
#19100 = DIRECTION ( 'NONE',  ( -0.000000000000000000, 0.000000000000000000, 1.000000000000000000 ) ) ;
#19101 = CARTESIAN_POINT ( 'NONE',  ( -19.50000000000000711, 1.387778780781445676E-14, 62.49999999999999289 ) ) ;
#19102 = DIRECTION ( 'NONE',  ( 0.000000000000000000, 0.000000000000000000, 1.000000000000000000 ) ) ;
#19103 = CARTESIAN_POINT ( 'NONE',  ( -19.87500762523393050, 2.235808837979148311, 7.626218077512941562 ) ) ;
#19104 = CARTESIAN_POINT ( 'NONE',  ( 19.74328841314636307, 3.194145055459935101, 7.652108011868850035 ) ) ;
#19105 = CARTESIAN_POINT ( 'NONE',  ( -18.10797733959156020, -8.533081443083743167, 18.35377592296120497 ) ) ;
#19106 = FACE_OUTER_BOUND ( 'NONE', #23413, .T. ) ;
#19107 = ORIENTED_EDGE ( 'NONE', *, *, #21639, .T. ) ;
#19108 = ORIENTED_EDGE ( 'NONE', *, *, #14661, .T. ) ;
#19109 = CARTESIAN_POINT ( 'NONE',  ( 23.96732207938043402, -33.98584080152387088, -1.500000000000000000 ) ) ;
#19110 = EDGE_CURVE ( 'NONE', #2495, #15425, #9851, .T. ) ;
#19111 = CYLINDRICAL_SURFACE ( 'NONE', #17880, 50.00000000000000000 ) ;
#19112 = EDGE_CURVE ( 'NONE', #25215, #29598, #23414, .T. ) ;
#19113 = CARTESIAN_POINT ( 'NONE',  ( 11.32565050298867959, -16.48467196965850690, 20.32200205377525393 ) ) ;
#19114 = EDGE_LOOP ( 'NONE', ( #7960, #12635, #10295, #2725 ) ) ;
#19115 = AXIS2_PLACEMENT_3D ( 'NONE', #19407, #18956, #28925 ) ;
#19116 = CARTESIAN_POINT ( 'NONE',  ( 15.45343642833785935, -7.142940632752240226, 18.80699882434806369 ) ) ;
#19117 = CARTESIAN_POINT ( 'NONE',  ( 4.870982490315499902, 16.31268916845847627, 6.111214848085761986 ) ) ;
#19118 = AXIS2_PLACEMENT_3D ( 'NONE', #24438, #2936, #3079 ) ;
#19119 = VERTEX_POINT ( 'NONE', #10892 ) ;
#19120 = VECTOR ( 'NONE', #10996, 1000.000000000000000 ) ;
#19121 = FACE_OUTER_BOUND ( 'NONE', #18736, .T. ) ;
#19122 = ADVANCED_FACE ( 'NONE', ( #12763 ), #10578, .F. ) ;
#19123 = DIRECTION ( 'NONE',  ( 0.000000000000000000, 0.000000000000000000, 1.000000000000000000 ) ) ;
#19124 = DIRECTION ( 'NONE',  ( 0.4154150130018859910, 0.9096319953545186632, 0.000000000000000000 ) ) ;
#19125 = CARTESIAN_POINT ( 'NONE',  ( -36.22259173693688439, 9.790317618809798006, 37.49999999994849986 ) ) ;
#19126 = ORIENTED_EDGE ( 'NONE', *, *, #16652, .F. ) ;
#19127 = CARTESIAN_POINT ( 'NONE',  ( -28.37932450449293853, 10.51822134874671022, 1.500000000000000000 ) ) ;
#19128 = EDGE_CURVE ( 'NONE', #3416, #14124, #22292, .T. ) ;
#19129 = CARTESIAN_POINT ( 'NONE',  ( 0.000000000000000000, 0.000000000000000000, -16.50000000000000000 ) ) ;
#19130 = DIRECTION ( 'NONE',  ( -0.000000000000000000, -0.000000000000000000, -1.000000000000000000 ) ) ;
#19131 = EDGE_LOOP ( 'NONE', ( #21093, #19080, #6416, #1631 ) ) ;
#19132 = CARTESIAN_POINT ( 'NONE',  ( -15.45998620766333431, -7.136073936211801083, 5.940635272151477686 ) ) ;
#19133 = CARTESIAN_POINT ( 'NONE',  ( -7.856594496258223259, -4.390207617113929039, 21.50000000000000000 ) ) ;
#19134 = DIRECTION ( 'NONE',  ( 0.000000000000000000, -0.000000000000000000, 1.000000000000000000 ) ) ;
#19135 = PRODUCT_DEFINITION_SHAPE ( 'NONE', 'NONE',  #30861 ) ;
#19136 = CARTESIAN_POINT ( 'NONE',  ( -0.01062192699083326121, -17.02590662965304347, 6.018569869498933578 ) ) ;
#19137 = CARTESIAN_POINT ( 'NONE',  ( 16.65122935894595813, 13.93942108199718888, 1.500000000000000000 ) ) ;
#19138 = DIRECTION ( 'NONE',  ( 0.000000000000000000, 0.000000000000000000, -1.000000000000000000 ) ) ;
#19139 = AXIS2_PLACEMENT_3D ( 'NONE', #22598, #1090, #7644 ) ;
#19140 = DIRECTION ( 'NONE',  ( -0.000000000000000000, -0.000000000000000000, 1.000000000000000000 ) ) ;
#19141 = PLANE ( 'NONE',  #21837 ) ;
#19142 = ORIENTED_EDGE ( 'NONE', *, *, #10165, .F. ) ;
#19143 = EDGE_CURVE ( 'NONE', #19850, #13279, #19314, .T. ) ;
#19144 = ADVANCED_FACE ( 'NONE', ( #1068 ), #3720, .F. ) ;
#19145 = CARTESIAN_POINT ( 'NONE',  ( -6.047835543919368284, 15.95440705812618809, 5.759928666072748449 ) ) ;
#19146 = DIRECTION ( 'NONE',  ( -1.000000000000000000, 0.000000000000000000, 0.000000000000000000 ) ) ;
#19147 = ORIENTED_EDGE ( 'NONE', *, *, #23433, .F. ) ;
#19148 = VERTEX_POINT ( 'NONE', #24924 ) ;
#19149 = CIRCLE ( 'NONE', #14187, 6.999999999999999112 ) ;
#19150 = CARTESIAN_POINT ( 'NONE',  ( -15.89797731339010234, 12.13494807016273924, 6.149077423860697778 ) ) ;
#19151 = CARTESIAN_POINT ( 'NONE',  ( -11.90245152369472059, 48.56370570873113479, -64.14171519351066308 ) ) ;
#19152 = LINE ( 'NONE', #28197, #10379 ) ;
#19153 = ORIENTED_EDGE ( 'NONE', *, *, #10885, .F. ) ;
#19154 = DIRECTION ( 'NONE',  ( -0.000000000000000000, -0.000000000000000000, 1.000000000000000000 ) ) ;
#19155 = CARTESIAN_POINT ( 'NONE',  ( 49.99999999999998579, -67.00000000000000000, 59.49999999999999289 ) ) ;
#19156 = ORIENTED_EDGE ( 'NONE', *, *, #11667, .F. ) ;
#19157 = CARTESIAN_POINT ( 'NONE',  ( 18.71162862491809875, -7.111980085401800267, 19.69140814234746273 ) ) ;
#19158 = CARTESIAN_POINT ( 'NONE',  ( -8.824744466605359605, -8.513189541288717521, 24.50000000000000000 ) ) ;
#19159 = ORIENTED_EDGE ( 'NONE', *, *, #14766, .F. ) ;
#19160 = CARTESIAN_POINT ( 'NONE',  ( 15.38884489568443037, -7.274072546993983757, 19.47784884541372818 ) ) ;
#19161 = AXIS2_PLACEMENT_3D ( 'NONE', #14734, #5539, #7426 ) ;
#19162 = ORIENTED_EDGE ( 'NONE', *, *, #10765, .T. ) ;
#19163 = EDGE_LOOP ( 'NONE', ( #18957, #18245, #29783, #15010 ) ) ;
#19164 = CARTESIAN_POINT ( 'NONE',  ( 37.99999999999999289, 90.00000000000001421, -40.50000000000000711 ) ) ;
#19165 = LINE ( 'NONE', #29143, #8663 ) ;
#19166 = CARTESIAN_POINT ( 'NONE',  ( -15.57266529552203416, 38.96488032230103471, -1.500000000000000000 ) ) ;
#19167 = CARTESIAN_POINT ( 'NONE',  ( -14.71622834324241147, -8.664216105422211101, 19.61324152429827095 ) ) ;
#19168 = CARTESIAN_POINT ( 'NONE',  ( 1.664698296051879023, -16.99226504954120287, 19.85459532544248873 ) ) ;
#19169 = CARTESIAN_POINT ( 'NONE',  ( 19.82606750293204811, 2.764250834391621225, 18.44501272782439827 ) ) ;
#19170 = VERTEX_POINT ( 'NONE', #22722 ) ;
#19171 = CARTESIAN_POINT ( 'NONE',  ( -16.89118935510124331, 2.183074208216233547, 18.49267272388512140 ) ) ;
#19172 = EDGE_CURVE ( 'NONE', #19937, #19074, #3375, .T. ) ;
#19173 = DIRECTION ( 'NONE',  ( 0.000000000000000000, 1.000000000000000000, 0.000000000000000000 ) ) ;
#19174 = LINE ( 'NONE', #12162, #28749 ) ;
#19175 = ORIENTED_EDGE ( 'NONE', *, *, #21369, .F. ) ;
#19176 = ORIENTED_EDGE ( 'NONE', *, *, #20682, .T. ) ;
#19177 = CARTESIAN_POINT ( 'NONE',  ( 40.05104235265675783, -2.353288714521559744, -6.500000000000000888 ) ) ;
#19178 = CARTESIAN_POINT ( 'NONE',  ( -4.163336342344337027E-14, 1.387778780781445676E-14, 1.500000000000000000 ) ) ;
#19179 = CYLINDRICAL_SURFACE ( 'NONE', #8875, 0.7500000000000006661 ) ;
#19180 = CARTESIAN_POINT ( 'NONE',  ( -5.369726540290506556, 19.28438192063506662, 18.55820869691756769 ) ) ;
#19181 = CARTESIAN_POINT ( 'NONE',  ( -15.52715705409340785, -6.980092275572870264, 6.143977687428009204 ) ) ;
#19182 = CARTESIAN_POINT ( 'NONE',  ( 0.000000000000000000, 0.000000000000000000, 21.50000000000000000 ) ) ;
#19183 = CARTESIAN_POINT ( 'NONE',  ( -5.976020107417634009, 19.08630880174946043, 5.652196082369965069 ) ) ;
#19184 = ORIENTED_EDGE ( 'NONE', *, *, #20210, .F. ) ;
#19185 = LINE ( 'NONE', #5467, #10250 ) ;
#19186 = FACE_OUTER_BOUND ( 'NONE', #16503, .T. ) ;
#19187 = DIRECTION ( 'NONE',  ( -0.000000000000000000, -0.000000000000000000, -1.000000000000000000 ) ) ;
#19188 = EDGE_LOOP ( 'NONE', ( #4717, #12535, #1647 ) ) ;
#19189 = CARTESIAN_POINT ( 'NONE',  ( 13.01404215953674104, 10.97082360537801549, 6.755862304746362845 ) ) ;
#19190 = ORIENTED_EDGE ( 'NONE', *, *, #26687, .T. ) ;
#19191 = CARTESIAN_POINT ( 'NONE',  ( 16.15906311113807803, -5.516254886378326283, 7.098451512883313441 ) ) ;
#19192 = CYLINDRICAL_SURFACE ( 'NONE', #11396, 6.000000000000005329 ) ;
#19193 = B_SPLINE_CURVE_WITH_KNOTS ( 'NONE', 3,
 ( #4548, #21385, #19052, #16404, #26069, #14673, #21215, #18911, #6890, #25918, #28724, #14526, #24024, #4700, #21686, #28886, #16870, #7197 ),
 .UNSPECIFIED., .F., .F.,
 ( 4, 2, 2, 2, 2, 2, 2, 2, 4 ),
 ( 0.003174295595554331266, 0.003570702171545574004, 0.003967108747536816742, 0.004363515323528056010, 0.004759921899519296146, 0.005156328475510535414, 0.005552735051501772948, 0.005949141627493012216, 0.006345548203484250617 ),
 .UNSPECIFIED. ) ;
#19194 = DIRECTION ( 'NONE',  ( 1.000000000000000000, 0.000000000000000000, 0.000000000000000000 ) ) ;
#19195 = ORIENTED_EDGE ( 'NONE', *, *, #18739, .F. ) ;
#19196 = CARTESIAN_POINT ( 'NONE',  ( 22.58682123248537366, -30.76127850100380101, 27.50000000000000711 ) ) ;
#19197 = CARTESIAN_POINT ( 'NONE',  ( 3.971879806607525598, 16.57852306707252055, 5.652605728828375753 ) ) ;
#19198 = CARTESIAN_POINT ( 'NONE',  ( 5.069257791428381843, -7.538175180318440027, 13.22130136205108819 ) ) ;
#19199 = DIRECTION ( 'NONE',  ( 1.000000000000000000, -2.396195514597832977E-15, 0.000000000000000000 ) ) ;
#19200 = CARTESIAN_POINT ( 'NONE',  ( -6.364020599487750118, 6.482337650448473099, -1.500000000000001110 ) ) ;
#19201 = DIRECTION ( 'NONE',  ( 1.000000000000000000, 0.000000000000000000, 0.000000000000000000 ) ) ;
#19202 = ORIENTED_EDGE ( 'NONE', *, *, #27367, .F. ) ;
#19203 = CARTESIAN_POINT ( 'NONE',  ( 15.70571165143382508, -6.606148062399648246, 7.626437579292364433 ) ) ;
#19204 = CARTESIAN_POINT ( 'NONE',  ( 39.00000000000000000, 5.563236990218597633, -1.500000000000000000 ) ) ;
#19205 = CIRCLE ( 'NONE', #6281, 0.7500000000000006661 ) ;
#19206 = DIRECTION ( 'NONE',  ( -0.9329908884337522190, 0.3598999890241700306, 0.000000000000000000 ) ) ;
#19207 = ORIENTED_EDGE ( 'NONE', *, *, #25631, .F. ) ;
#19208 = FACE_OUTER_BOUND ( 'NONE', #12922, .T. ) ;
#19209 = CARTESIAN_POINT ( 'NONE',  ( 9.056208293496309736, -2.810445847081889159, 21.50000000000000000 ) ) ;
#19210 = DIRECTION ( 'NONE',  ( -0.000000000000000000, -0.000000000000000000, 1.000000000000000000 ) ) ;
#19211 = DIRECTION ( 'NONE',  ( -0.000000000000000000, -0.000000000000000000, 1.000000000000000000 ) ) ;
#19212 = CARTESIAN_POINT ( 'NONE',  ( -32.74775157610409337, 27.21557300919391054, -19.50000000000000355 ) ) ;
#19213 = ORIENTED_EDGE ( 'NONE', *, *, #17035, .F. ) ;
#19214 = VECTOR ( 'NONE', #21866, 1000.000000000000000 ) ;
#19215 = CARTESIAN_POINT ( 'NONE',  ( 38.89137791791456067, -3.432770781813833771, 35.06776335884041629 ) ) ;
#19216 = FACE_OUTER_BOUND ( 'NONE', #3898, .T. ) ;
#19217 = ORIENTED_EDGE ( 'NONE', *, *, #24212, .T. ) ;
#19218 = AXIS2_PLACEMENT_3D ( 'NONE', #19664, #7824, #26865 ) ;
#19219 = CYLINDRICAL_SURFACE ( 'NONE', #22655, 50.00000000000000000 ) ;
#19220 = VERTEX_POINT ( 'NONE', #8403 ) ;
#19221 = CARTESIAN_POINT ( 'NONE',  ( 28.78283879316666827, -7.125616703334846314, 41.10667063058290438 ) ) ;
#19222 = FACE_OUTER_BOUND ( 'NONE', #30287, .T. ) ;
#19223 = ORIENTED_EDGE ( 'NONE', *, *, #8248, .T. ) ;
#19224 = VERTEX_POINT ( 'NONE', #1534 ) ;
#19225 = CARTESIAN_POINT ( 'NONE',  ( 7.869584159753955532, 10.39565510934977333, 24.50000000000000000 ) ) ;
#19226 = ORIENTED_EDGE ( 'NONE', *, *, #7357, .T. ) ;
#19227 = VECTOR ( 'NONE', #29578, 1000.000000000000000 ) ;
#19228 = ORIENTED_EDGE ( 'NONE', *, *, #8911, .F. ) ;
#19229 = ORIENTED_EDGE ( 'NONE', *, *, #15695, .F. ) ;
#19230 = CARTESIAN_POINT ( 'NONE',  ( -0.6060441907983137311, -20.00878639882294507, 19.00652017443069752 ) ) ;
#19231 = VECTOR ( 'NONE', #22332, 1000.000000000000000 ) ;
#19232 = DIRECTION ( 'NONE',  ( 0.7557495743542581579, 0.6548607339452852116, -0.000000000000000000 ) ) ;
#19233 = CARTESIAN_POINT ( 'NONE',  ( -32.98805937973593672, 22.67054169308932643, 18.00000000000000000 ) ) ;
#19234 = CARTESIAN_POINT ( 'NONE',  ( 1.424502173535765914, -17.00587888132690040, 18.56793045041961321 ) ) ;
#19235 = ORIENTED_EDGE ( 'NONE', *, *, #10935, .F. ) ;
#19236 = ADVANCED_FACE ( 'NONE', ( #18063 ), #20088, .F. ) ;
#19237 = DIRECTION ( 'NONE',  ( -1.000000000000000000, 0.000000000000000000, 0.000000000000000000 ) ) ;
#19238 = CIRCLE ( 'NONE', #11762, 12.18947652193948272 ) ;
#19239 = CARTESIAN_POINT ( 'NONE',  ( 27.86235613436985759, 14.72519157938689460, 43.48653168448679196 ) ) ;
#19240 = CARTESIAN_POINT ( 'NONE',  ( 11.67645754117907586, 12.46194352177088582, 19.58863275299554019 ) ) ;
#19241 = FACE_OUTER_BOUND ( 'NONE', #3627, .T. ) ;
#19242 = ORIENTED_EDGE ( 'NONE', *, *, #3095, .F. ) ;
#19243 = AXIS2_PLACEMENT_3D ( 'NONE', #22074, #20048, #708 ) ;
#19244 = TOROIDAL_SURFACE ( 'NONE', #27225, 7.000000000000000000, 3.000000000000000000 ) ;
#19245 = CARTESIAN_POINT ( 'NONE',  ( -37.16608720827707657, 65.00000000000000000, 97.07879600563551037 ) ) ;
#19246 = CARTESIAN_POINT ( 'NONE',  ( -14.80332652839583574, -8.501125445468646902, 6.041646659195333058 ) ) ;
#19247 = CARTESIAN_POINT ( 'NONE',  ( -6.842536740270957374, 18.81187820119070508, 7.098451512883313441 ) ) ;
#19248 = DIRECTION ( 'NONE',  ( -0.4495526574063634095, 0.8932538319083086487, 0.000000000000000000 ) ) ;
#19249 = DIRECTION ( 'NONE',  ( -0.000000000000000000, 0.000000000000000000, 1.000000000000000000 ) ) ;
#19250 = EDGE_CURVE ( 'NONE', #9427, #22347, #733, .T. ) ;
#19251 = CARTESIAN_POINT ( 'NONE',  ( -18.07538971572905950, -8.601943808150396720, 18.34777357837151968 ) ) ;
#19252 = CARTESIAN_POINT ( 'NONE',  ( 12.56641067637628240, -40.32935944494942504, -1.500000000000000000 ) ) ;
#19253 = VECTOR ( 'NONE', #29540, 1000.000000000000000 ) ;
#19254 = ORIENTED_EDGE ( 'NONE', *, *, #26046, .F. ) ;
#19255 = ORIENTED_EDGE ( 'NONE', *, *, #12223, .T. ) ;
#19256 = FILL_AREA_STYLE_COLOUR ( '', #18927 ) ;
#19257 = VECTOR ( 'NONE', #9159, 1000.000000000000000 ) ;
#19258 = CARTESIAN_POINT ( 'NONE',  ( 39.83602371821015709, 11.57901747687536265, -19.50000000000000355 ) ) ;
#19259 = CARTESIAN_POINT ( 'NONE',  ( -13.23068377149358987, 10.73719040084102794, 7.632642797338977658 ) ) ;
#19260 = CYLINDRICAL_SURFACE ( 'NONE', #28518, 0.7441270634457337607 ) ;
#19261 = ORIENTED_EDGE ( 'NONE', *, *, #9397, .T. ) ;
#19262 = APPLICATION_PROTOCOL_DEFINITION ( 'draft international standard', 'automotive_design', 1998, #5613 ) ;
#19263 = DIRECTION ( 'NONE',  ( 1.982541115402065110E-16, 0.000000000000000000, -1.000000000000000000 ) ) ;
#19265 = EDGE_CURVE ( 'NONE', #17481, #1130, #638, .T. ) ;
#19264 = VECTOR ( 'NONE', #15550, 1000.000000000000000 ) ;
#19266 = CARTESIAN_POINT ( 'NONE',  ( 4.370315982788584463, 16.46653586241586709, 5.701226463332907279 ) ) ;
#19268 = EDGE_CURVE ( 'NONE', #254, #20928, #3240, .T. ) ;
#19267 = VECTOR ( 'NONE', #17366, 1000.000000000000000 ) ;
#19269 = ORIENTED_EDGE ( 'NONE', *, *, #2602, .T. ) ;
#19270 = CARTESIAN_POINT ( 'NONE',  ( -26.44644203219470668, 9.801837641955994940, 1.500000000000000000 ) ) ;
#19271 = CIRCLE ( 'NONE', #29739, 5.000000000000004441 ) ;
#19272 = CARTESIAN_POINT ( 'NONE',  ( 14.30907656312162324, 13.99861481489062243, 7.196036389296800451 ) ) ;
#19273 = DIRECTION ( 'NONE',  ( 0.000000000000000000, 0.000000000000000000, -1.000000000000000000 ) ) ;
#19274 = CARTESIAN_POINT ( 'NONE',  ( -26.14179753137254636, 26.91385278145934024, 37.49999999999091216 ) ) ;
#19275 = ORIENTED_EDGE ( 'NONE', *, *, #21160, .T. ) ;
#19276 = CYLINDRICAL_SURFACE ( 'NONE', #2887, 9.482273699623480212 ) ;
#19277 = CARTESIAN_POINT ( 'NONE',  ( 25.47847050916410439, -26.57182937991349903, -1.500000000000001332 ) ) ;
#19278 = CARTESIAN_POINT ( 'NONE',  ( 23.27838112219106392, 36.10018657900367600, -16.50000600000000262 ) ) ;
#19279 = CIRCLE ( 'NONE', #23252, 20.00000000000000000 ) ;
#19280 = EDGE_LOOP ( 'NONE', ( #2980, #4825, #30560, #25652 ) ) ;
#19281 = CARTESIAN_POINT ( 'NONE',  ( -15.35255149521179874, -7.379222211227442152, 7.557577766377196582 ) ) ;
#19282 = FACE_OUTER_BOUND ( 'NONE', #29754, .T. ) ;
#19283 = EDGE_CURVE ( 'NONE', #25580, #8889, #14400, .T. ) ;
#19284 = DIRECTION ( 'NONE',  ( -0.000000000000000000, -0.000000000000000000, 1.000000000000000000 ) ) ;
#19285 = EDGE_CURVE ( 'NONE', #19397, #1725, #9303, .T. ) ;
#19286 = CARTESIAN_POINT ( 'NONE',  ( -0.5567245496722502685, -20.01015347392404564, 6.211014596808754007 ) ) ;
#19287 = AXIS2_PLACEMENT_3D ( 'NONE', #17631, #27460, #3908 ) ;
#19288 = EDGE_CURVE ( 'NONE', #14448, #315, #1040, .T. ) ;
#19289 = DIRECTION ( 'NONE',  ( 0.000000000000000000, 1.000000000000000000, 0.000000000000000000 ) ) ;
#19290 = VECTOR ( 'NONE', #12434, 1000.000000000000000 ) ;
#19291 = DIRECTION ( 'NONE',  ( 1.000000000000000000, 0.000000000000000000, 0.000000000000000000 ) ) ;
#19292 = CARTESIAN_POINT ( 'NONE',  ( 37.45985526150776934, -11.82899854519495797, 10.75678081308941003 ) ) ;
#19293 = CARTESIAN_POINT ( 'NONE',  ( -32.98805937973593672, 80.00000000000000000, 18.00000000000000000 ) ) ;
#19294 = VERTEX_POINT ( 'NONE', #25850 ) ;
#19295 = EDGE_CURVE ( 'NONE', #22222, #29647, #25771, .T. ) ;
#19296 = DIRECTION ( 'NONE',  ( 0.000000000000000000, 0.000000000000000000, -1.000000000000000000 ) ) ;
#19297 = AXIS2_PLACEMENT_3D ( 'NONE', #22440, #22127, #26834 ) ;
#19298 = CARTESIAN_POINT ( 'NONE',  ( -3.196529495465446402, -8.413215745754985875, -3.621320343559650379 ) ) ;
#19299 = ORIENTED_EDGE ( 'NONE', *, *, #16012, .T. ) ;
#19300 = ORIENTED_EDGE ( 'NONE', *, *, #92, .F. ) ;
#19301 = EDGE_CURVE ( 'NONE', #10553, #25466, #12851, .T. ) ;
#19302 = CARTESIAN_POINT ( 'NONE',  ( -13.76736161019652371, 39.80458471794007380, 21.94892721098231902 ) ) ;
#19303 = AXIS2_PLACEMENT_3D ( 'NONE', #5371, #23927, #28469 ) ;
#19304 = EDGE_CURVE ( 'NONE', #17232, #13976, #14315, .T. ) ;
#19305 = CARTESIAN_POINT ( 'NONE',  ( -9.148437479020795848, 49.15745090874974466, -43.10266427149625201 ) ) ;
#19306 = ORIENTED_EDGE ( 'NONE', *, *, #22384, .T. ) ;
#19307 = CARTESIAN_POINT ( 'NONE',  ( -3.515970705488605130, 17.06554576617236307, 1.500000000000000000 ) ) ;
#19308 = ADVANCED_FACE ( 'NONE', ( #11192 ), #4482, .F. ) ;
#19309 = ORIENTED_EDGE ( 'NONE', *, *, #22337, .F. ) ;
#19310 = CARTESIAN_POINT ( 'NONE',  ( 15.87456320658223241, -6.220724357885990763, 18.35718225375110180 ) ) ;
#19311 = CARTESIAN_POINT ( 'NONE',  ( 16.61290147319822452, 3.916522693408248657, 18.64703902303423178 ) ) ;
#19312 = DIRECTION ( 'NONE',  ( 1.000000000000000000, 0.000000000000000000, 0.000000000000000000 ) ) ;
#19313 = VERTEX_POINT ( 'NONE', #23488 ) ;
#19314 = CIRCLE ( 'NONE', #30747, 4.999999999999997335 ) ;
#19315 = CARTESIAN_POINT ( 'NONE',  ( -15.57266529552203416, 38.96488032230103471, 1.500000000000000000 ) ) ;
#19316 = ORIENTED_EDGE ( 'NONE', *, *, #30693, .T. ) ;
#19317 = VERTEX_POINT ( 'NONE', #2129 ) ;
#19318 = EDGE_CURVE ( 'NONE', #12217, #1853, #22786, .T. ) ;
#19319 = EDGE_CURVE ( 'NONE', #4512, #6958, #6365, .T. ) ;
#19320 = CARTESIAN_POINT ( 'NONE',  ( 2.703030265324084080, -12.75514121382991384, 24.50000000000000000 ) ) ;
#19321 = CARTESIAN_POINT ( 'NONE',  ( -12.74366836927934798, 11.28516576207253408, 19.66989035740801839 ) ) ;
#19322 = CIRCLE ( 'NONE', #8387, 3.000000000000002665 ) ;
#19323 = VECTOR ( 'NONE', #24346, 1000.000000000000000 ) ;
#19324 = EDGE_CURVE ( 'NONE', #6974, #22885, #17309, .T. ) ;
#19325 = CARTESIAN_POINT ( 'NONE',  ( -9.772441304892783620, -17.47026709695451174, 18.82680253904184298 ) ) ;
#19326 = CARTESIAN_POINT ( 'NONE',  ( 19.74328841314636307, 3.194145055459935101, 7.652108011868850035 ) ) ;
#19327 = DIRECTION ( 'NONE',  ( -0.000000000000000000, -0.000000000000000000, 1.000000000000000000 ) ) ;
#19328 = CARTESIAN_POINT ( 'NONE',  ( 0.000000000000000000, -7.422978769709303177E-15, 65.52304386563415051 ) ) ;
#19329 = VERTEX_POINT ( 'NONE', #16331 ) ;
#19330 = DIRECTION ( 'NONE',  ( 0.000000000000000000, 1.000000000000000000, 0.000000000000000000 ) ) ;
#19331 = CARTESIAN_POINT ( 'NONE',  ( -28.11661694678904766, 29.45258986749694330, 11.85255554064003647 ) ) ;
#19332 = VECTOR ( 'NONE', #29420, 1000.000000000000000 ) ;
#19333 = CARTESIAN_POINT ( 'NONE',  ( 15.05691039802740150, 13.16451011206821597, 20.32243167357989577 ) ) ;
#19334 = FACE_OUTER_BOUND ( 'NONE', #27444, .T. ) ;
#19335 = ORIENTED_EDGE ( 'NONE', *, *, #20814, .T. ) ;
#19336 = ORIENTED_EDGE ( 'NONE', *, *, #11860, .T. ) ;
#19337 = VECTOR ( 'NONE', #15987, 1000.000000000000000 ) ;
#19338 = FACE_OUTER_BOUND ( 'NONE', #4578, .T. ) ;
#19339 = DIRECTION ( 'NONE',  ( -0.5406408174555974444, -0.8412535328311813165, 0.000000000000000000 ) ) ;
#19340 = DIRECTION ( 'NONE',  ( 1.000000000000000000, 0.000000000000000000, 0.000000000000000000 ) ) ;
#19341 = CARTESIAN_POINT ( 'NONE',  ( -13.89991139849285773, 7.447222512978775022, -0.6213203435596476032 ) ) ;
#19342 = CARTESIAN_POINT ( 'NONE',  ( -15.52789627658390614, -6.978352780205158368, 7.156916968540300239 ) ) ;
#19343 = CARTESIAN_POINT ( 'NONE',  ( -10.18506332983503881, -29.04537757311073065, 1.500000000000001332 ) ) ;
#19344 = CIRCLE ( 'NONE', #11388, 7.500000000000000000 ) ;
#19345 = ORIENTED_EDGE ( 'NONE', *, *, #16438, .F. ) ;
#19346 = VECTOR ( 'NONE', #17375, 1000.000000000000000 ) ;
#19347 = ORIENTED_EDGE ( 'NONE', *, *, #30510, .F. ) ;
#19348 = DIRECTION ( 'NONE',  ( 0.000000000000000000, 1.000000000000000000, 0.000000000000000000 ) ) ;
#19349 = CIRCLE ( 'NONE', #5905, 6.000000000000005329 ) ;
#19350 = CARTESIAN_POINT ( 'NONE',  ( 37.99999999999999289, 70.00000000000000000, -81.50000000000001421 ) ) ;
#19351 = DIRECTION ( 'NONE',  ( 0.000000000000000000, 0.000000000000000000, 1.000000000000000000 ) ) ;
#19352 = ORIENTED_EDGE ( 'NONE', *, *, #25991, .F. ) ;
#19353 = CARTESIAN_POINT ( 'NONE',  ( 20.71335220384823117, 27.86167394782616213, -16.50001200000000168 ) ) ;
#19354 = ORIENTED_EDGE ( 'NONE', *, *, #13347, .T. ) ;
#19355 = ADVANCED_FACE ( 'NONE', ( #6362 ), #13694, .F. ) ;
#19356 = CARTESIAN_POINT ( 'NONE',  ( 18.73355814148580833, -7.053980495653730642, 6.672349528511551497 ) ) ;
#19357 = EDGE_CURVE ( 'NONE', #3847, #5226, #4022, .T. ) ;
#19358 = CARTESIAN_POINT ( 'NONE',  ( -33.25198513809938561, 23.59839681648617216, -8.166573414591429270 ) ) ;
#19359 = AXIS2_PLACEMENT_3D ( 'NONE', #6190, #15691, #3851 ) ;
#19360 = DIRECTION ( 'NONE',  ( -0.000000000000000000, -0.000000000000000000, -1.000000000000000000 ) ) ;
#19361 = ORIENTED_EDGE ( 'NONE', *, *, #3335, .F. ) ;
#19362 = CARTESIAN_POINT ( 'NONE',  ( 5.225607896785846584, 19.32380464960333555, 5.652605728828375753 ) ) ;
#19363 = CARTESIAN_POINT ( 'NONE',  ( 37.99999999999999289, 209.2686044187655909, -34.50000000000000000 ) ) ;
#19364 = PLANE ( 'NONE',  #4854 ) ;
#19365 = DIRECTION ( 'NONE',  ( 0.000000000000000000, -0.000000000000000000, -1.000000000000000000 ) ) ;
#19366 = CARTESIAN_POINT ( 'NONE',  ( -0.8750451464063155882, -9.041888939645136958, 21.50000000000000000 ) ) ;
#19367 = CARTESIAN_POINT ( 'NONE',  ( 26.80246859415415273, -7.028748154183637631, -1.499999999999999556 ) ) ;
#19368 = CARTESIAN_POINT ( 'NONE',  ( 0.1469846612282507681, 6.696526368584472699, -6.401276095386996268 ) ) ;
#19369 = ORIENTED_EDGE ( 'NONE', *, *, #12030, .F. ) ;
#19370 = CARTESIAN_POINT ( 'NONE',  ( 26.36764545593179676, 31.31467416275351923, -1.500000000000000000 ) ) ;
#19371 = CIRCLE ( 'NONE', #28356, 1.000000000000010436 ) ;
#19372 = CARTESIAN_POINT ( 'NONE',  ( 13.22505861668195237, -42.10773672056998862, -19.50000000000000355 ) ) ;
#19373 = VECTOR ( 'NONE', #20745, 1000.000000000000000 ) ;
#19374 = PLANE ( 'NONE',  #10335 ) ;
#19375 = EDGE_LOOP ( 'NONE', ( #9958, #15410, #8695, #26565 ) ) ;
#19376 = CARTESIAN_POINT ( 'NONE',  ( -15.75094665830067697, -12.32508334119358828, 1.500000000000001332 ) ) ;
#19377 = CARTESIAN_POINT ( 'NONE',  ( 6.437793815610357129, -6.974883619896809606, 21.50000000000000000 ) ) ;
#19378 = CARTESIAN_POINT ( 'NONE',  ( -2.516121109503243858, -8.728722367416578365, 21.50000000000000000 ) ) ;
#19379 = CARTESIAN_POINT ( 'NONE',  ( -2.552544030762004645, -42.50000000000000000, -1.500000000000000000 ) ) ;
#19380 = CIRCLE ( 'NONE', #11932, 9.482273699623480212 ) ;
#19381 = CARTESIAN_POINT ( 'NONE',  ( 0.000000000000000000, 0.000000000000000000, -1.500000000000000000 ) ) ;
#19382 = B_SPLINE_CURVE_WITH_KNOTS ( 'NONE', 3,
 ( #10866, #20208, #15684, #13367, #3381, #20374, #29900, #22404 ),
 .UNSPECIFIED., .F., .F.,
 ( 4, 2, 2, 4 ),
 ( 0.000000000000000000, 0.005288043134213118134, 0.007932064701319680236, 0.01057608626842624147 ),
 .UNSPECIFIED. ) ;
#19383 = CARTESIAN_POINT ( 'NONE',  ( 34.13328053751565250, 15.58287797514595141, 37.50000000001482903 ) ) ;
#19384 = CARTESIAN_POINT ( 'NONE',  ( 19.65639872822723433, 3.693339721720553914, 7.528076282304597022 ) ) ;
#19385 = EDGE_LOOP ( 'NONE', ( #4422, #24147, #9054, #622 ) ) ;
#19386 = AXIS2_PLACEMENT_3D ( 'NONE', #16269, #25791, #25491 ) ;
#19387 = CARTESIAN_POINT ( 'NONE',  ( 33.14492814497746309, -23.43596551657708105, -6.499906363187121450 ) ) ;
#19388 = ORIENTED_EDGE ( 'NONE', *, *, #11258, .F. ) ;
#19389 = CARTESIAN_POINT ( 'NONE',  ( -40.00000000000000000, 67.32050807568877815, 12.49999999999999112 ) ) ;
#19390 = CARTESIAN_POINT ( 'NONE',  ( -28.34828976096172326, 29.18752572968383063, -1.500000000000000000 ) ) ;
#19391 = ORIENTED_EDGE ( 'NONE', *, *, #381, .T. ) ;
#19392 = ORIENTED_EDGE ( 'NONE', *, *, #799, .T. ) ;
#19393 = CARTESIAN_POINT ( 'NONE',  ( -4.776122516674677878E-15, -42.50000000000000000, 24.50000000000000000 ) ) ;
#19394 = VERTEX_POINT ( 'NONE', #1831 ) ;
#19395 = AXIS2_PLACEMENT_3D ( 'NONE', #28944, #19576, #394 ) ;
#19396 = ORIENTED_EDGE ( 'NONE', *, *, #4224, .T. ) ;
#19397 = VERTEX_POINT ( 'NONE', #11356 ) ;
#19398 = CARTESIAN_POINT ( 'NONE',  ( -0.5696721008582762424, -20.00987732873323210, 19.77662771831109367 ) ) ;
#19399 = CARTESIAN_POINT ( 'NONE',  ( -23.16735716920978660, 10.90794401664034474, 49.39349105325691625 ) ) ;
#19400 = CARTESIAN_POINT ( 'NONE',  ( -9.723733991145046218, -17.49730778217155702, 6.233981582756856987 ) ) ;
#19401 = CARTESIAN_POINT ( 'NONE',  ( 4.641725321057754705, 16.38498716467266547, 18.54473042795394733 ) ) ;
#19402 = CARTESIAN_POINT ( 'NONE',  ( 1.068432182113367768, -19.98925970413800002, 20.06253562465620632 ) ) ;
#19403 = ORIENTED_EDGE ( 'NONE', *, *, #5134, .T. ) ;
#19404 = CARTESIAN_POINT ( 'NONE',  ( 39.99999999999998579, 80.00000000000001421, 52.49999999999999289 ) ) ;
#19405 = CARTESIAN_POINT ( 'NONE',  ( 22.54178090630008313, -36.64935163255146477, -16.50000000000000000 ) ) ;
#19406 = CARTESIAN_POINT ( 'NONE',  ( 1.340340228783118537, -19.95510490826381655, 19.61564845152807735 ) ) ;
#19407 = CARTESIAN_POINT ( 'NONE',  ( -6.812559277181930106, 5.881244434206302607, 1.500000000000001332 ) ) ;
#19408 = EDGE_LOOP ( 'NONE', ( #16986, #29990, #20713, #30566 ) ) ;
#19409 = CIRCLE ( 'NONE', #11446, 7.500000000000013323 ) ;
#19410 = DIRECTION ( 'NONE',  ( 0.000000000000000000, 0.000000000000000000, 1.000000000000000000 ) ) ;
#19411 = CARTESIAN_POINT ( 'NONE',  ( -17.81743587613173574, -9.123988531026229865, 5.810767894563978686 ) ) ;
#19412 = CARTESIAN_POINT ( 'NONE',  ( -6.723597995833586083, 18.85470073956823356, 7.280727868105637768 ) ) ;
#19413 = CARTESIAN_POINT ( 'NONE',  ( -8.840471615930058036, 1.687027447297517080, 21.50000000000000000 ) ) ;
#19414 = CARTESIAN_POINT ( 'NONE',  ( -14.41708049311053053, 17.22181377296911720, 1.500000000000000000 ) ) ;
#19415 = CARTESIAN_POINT ( 'NONE',  ( -15.51812306427840937, -7.001296657735109896, 18.80699882434806369 ) ) ;
#19416 = CYLINDRICAL_SURFACE ( 'NONE', #28047, 0.7500000000000006661 ) ;
#19417 = ORIENTED_EDGE ( 'NONE', *, *, #22948, .F. ) ;
#19418 = VERTEX_POINT ( 'NONE', #20850 ) ;
#19419 = DIRECTION ( 'NONE',  ( -1.000000000000000000, 0.000000000000000000, -0.000000000000000000 ) ) ;
#19420 = CARTESIAN_POINT ( 'NONE',  ( 9.675133109038689838, -8.168544852422947145, -1.500000000000000000 ) ) ;
#19421 = DIRECTION ( 'NONE',  ( -0.000000000000000000, -0.000000000000000000, -1.000000000000000000 ) ) ;
#19422 = CARTESIAN_POINT ( 'NONE',  ( 37.16608720827707657, 65.00000000000000000, 12.49999999999999112 ) ) ;
#19423 = VERTEX_POINT ( 'NONE', #30376 ) ;
#19424 = AXIS2_PLACEMENT_3D ( 'NONE', #4725, #2394, #17043 ) ;
#19425 = LINE ( 'NONE', #5234, #12440 ) ;
#19426 = CARTESIAN_POINT ( 'NONE',  ( 3.685570353517261477, -16.10136545388692397, 24.50000000000000000 ) ) ;
#19427 = VERTEX_POINT ( 'NONE', #9012 ) ;
#19428 = CARTESIAN_POINT ( 'NONE',  ( 6.184030279945252673, 19.03884152227148263, 19.77662771831109367 ) ) ;
#19429 = CYLINDRICAL_SURFACE ( 'NONE', #12754, 5.000000000000004441 ) ;
#19430 = AXIS2_PLACEMENT_3D ( 'NONE', #3848, #11024, #24907 ) ;
#19431 = DIRECTION ( 'NONE',  ( -0.000000000000000000, -0.000000000000000000, 1.000000000000000000 ) ) ;
#19432 = CARTESIAN_POINT ( 'NONE',  ( -38.80437957496877033, -4.450587475999619791, 35.05861520490779526 ) ) ;
#19433 = ORIENTED_EDGE ( 'NONE', *, *, #18336, .F. ) ;
#19434 = DIRECTION ( 'NONE',  ( -0.000000000000000000, -0.000000000000000000, 1.000000000000000000 ) ) ;
#19435 = ADVANCED_FACE ( 'NONE', ( #18526 ), #28029, .F. ) ;
#19436 = DIRECTION ( 'NONE',  ( -0.000000000000000000, -0.000000000000000000, -1.000000000000000000 ) ) ;
#19437 = CARTESIAN_POINT ( 'NONE',  ( -5.105024945675580739, -42.22604126506273303, -1.500000000000000000 ) ) ;
#19438 = ORIENTED_EDGE ( 'NONE', *, *, #16781, .T. ) ;
#19439 = CARTESIAN_POINT ( 'NONE',  ( -15.26311659977724311, -7.574663188999290142, 7.632642797338977658 ) ) ;
#19440 = CARTESIAN_POINT ( 'NONE',  ( -42.49999999999998579, -50.00000000000000000, 97.07879600563551037 ) ) ;
#19441 = CARTESIAN_POINT ( 'NONE',  ( 14.70507365826912327, 13.55638513645770438, 7.626218077512938009 ) ) ;
#19442 = CARTESIAN_POINT ( 'NONE',  ( 0.7070334246190017602, -17.02861022043351724, 5.653912893140659257 ) ) ;
#19443 = CIRCLE ( 'NONE', #9964, 11.99999999999999645 ) ;
#19444 = DIRECTION ( 'NONE',  ( -0.000000000000000000, 0.000000000000000000, 1.000000000000000000 ) ) ;
#19445 = DIRECTION ( 'NONE',  ( -0.000000000000000000, -0.000000000000000000, 1.000000000000000000 ) ) ;
#19446 = CARTESIAN_POINT ( 'NONE',  ( 37.95968219450539749, -9.750946698478889729, 13.55336906631367810 ) ) ;
#19447 = FACE_OUTER_BOUND ( 'NONE', #20176, .T. ) ;
#19448 = ORIENTED_EDGE ( 'NONE', *, *, #26344, .T. ) ;
#19449 = B_SPLINE_CURVE_WITH_KNOTS ( 'NONE', 3,
 ( #13756, #13911, #12032, #28108, #16242, #4235, #1902, #26064, #2355, #11885, #2047, #19046, #16704, #21380, #4542, #4850, #17, #9529, #6730, #21063, #25760, #28563, #11569, #14367, #30586, #9683, #16101, #25621, #4695, #6883, #9225 ),
 .UNSPECIFIED., .F., .F.,
 ( 4, 2, 1, 1, 2, 2, 1, 2, 2, 2, 2, 2, 1, 2, 2, 1, 2, 4 ),
 ( 0.4060398654371175087, 0.4089824111038223298, 0.4119249567705270954, 0.4178100481039366820, 0.4207525937706414476, 0.4222238666039939137, 0.4236951394373462687, 0.4295802307707560219, 0.4531205961043950348, 0.4648907787712145412, 0.4678333244379194178, 0.4707758701046242944, 0.4766609614380340476, 0.4825460527714438563, 0.4884311441048536095, 0.4943162354382634183, 0.4972587811049682949, 0.5002013267716731715 ),
 .UNSPECIFIED. ) ;
#19450 = CARTESIAN_POINT ( 'NONE',  ( 0.000000000000000000, -2.435693370351110282E-15, 21.50000000000000355 ) ) ;
#19451 = LINE ( 'NONE', #15209, #11595 ) ;
#19452 = ORIENTED_EDGE ( 'NONE', *, *, #6578, .T. ) ;
#19453 = ORIENTED_EDGE ( 'NONE', *, *, #803, .F. ) ;
#19454 = CARTESIAN_POINT ( 'NONE',  ( -29.99999999999933209, 1.755172820525642916E-14, 77.49999999999998579 ) ) ;
#19455 = CARTESIAN_POINT ( 'NONE',  ( -7.531728742324322212, 49.43635587137926990, -41.99112863159430020 ) ) ;
#19456 = VERTEX_POINT ( 'NONE', #24415 ) ;
#19457 = EDGE_CURVE ( 'NONE', #4264, #14731, #27395, .T. ) ;
#19458 = CARTESIAN_POINT ( 'NONE',  ( 13.01739631533118668, 10.96666867565305381, 19.33715507985239412 ) ) ;
#19459 = EDGE_CURVE ( 'NONE', #14649, #5977, #14604, .T. ) ;
#19460 = CARTESIAN_POINT ( 'NONE',  ( -11.19021577446866900, -16.59822551944401781, 6.018569869498933578 ) ) ;
#19461 = ORIENTED_EDGE ( 'NONE', *, *, #1965, .T. ) ;
#19462 = ADVANCED_FACE ( 'NONE', ( #7272 ), #14911, .F. ) ;
#19463 = CARTESIAN_POINT ( 'NONE',  ( 18.55936137128098196, -7.500557692851354652, 20.19593175699879595 ) ) ;
#19464 = CARTESIAN_POINT ( 'NONE',  ( 69.99999999999998579, -70.00000000000000000, -92.50000000000000000 ) ) ;
#19465 = VECTOR ( 'NONE', #22915, 1000.000000000000000 ) ;
#19466 = FACE_OUTER_BOUND ( 'NONE', #898, .T. ) ;
#19467 = VERTEX_POINT ( 'NONE', #2449 ) ;
#19468 = CARTESIAN_POINT ( 'NONE',  ( 15.75996277359000075, -6.485024779738598255, 20.34789198813116329 ) ) ;
#19469 = ORIENTED_EDGE ( 'NONE', *, *, #5920, .T. ) ;
#19470 = ADVANCED_FACE ( 'NONE', ( #14746, #12269 ), #26301, .T. ) ;
#19471 = VERTEX_POINT ( 'NONE', #21617 ) ;
#19472 = ADVANCED_FACE ( 'NONE', ( #30823 ), #24107, .F. ) ;
#19473 = CARTESIAN_POINT ( 'NONE',  ( 13.71656802822472088, 39.80869574967974245, 29.07849776505763018 ) ) ;
#19474 = CARTESIAN_POINT ( 'NONE',  ( -6.157909564977937400, 15.91569265719595627, 18.56793045041961321 ) ) ;
#19475 = CARTESIAN_POINT ( 'NONE',  ( -14.74940038399478581, 13.53421240139457815, 19.77662771831109367 ) ) ;
#19476 = EDGE_CURVE ( 'NONE', #2130, #13676, #23655, .T. ) ;
#19477 = CARTESIAN_POINT ( 'NONE',  ( -7.715867830805694716, -15.23386229593460683, 19.03762469184452755 ) ) ;
#19478 = EDGE_CURVE ( 'NONE', #6853, #20269, #21460, .T. ) ;
#19479 = CARTESIAN_POINT ( 'NONE',  ( -7.055757556308441814, 41.80458111945913657, 28.90000488980968640 ) ) ;
#19480 = DIRECTION ( 'NONE',  ( 0.000000000000000000, -1.132880637372608986E-16, 1.000000000000000000 ) ) ;
#19481 = CARTESIAN_POINT ( 'NONE',  ( -26.11179934312166040, -14.04991663536888780, 41.10667063058298254 ) ) ;
#19482 = VERTEX_POINT ( 'NONE', #7905 ) ;
#19483 = CARTESIAN_POINT ( 'NONE',  ( 11.11866449908640675, -16.64592002940951332, 5.652196082367002106 ) ) ;
#19484 = PLANE ( 'NONE',  #10772 ) ;
#19485 = CIRCLE ( 'NONE', #20957, 0.7500000000000004441 ) ;
#19486 = CARTESIAN_POINT ( 'NONE',  ( 9.007989464659763357, -14.44232047555455445, 6.519181285484531685 ) ) ;
#19487 = ORIENTED_EDGE ( 'NONE', *, *, #12500, .F. ) ;
#19488 = ORIENTED_EDGE ( 'NONE', *, *, #21231, .T. ) ;
#19489 = CARTESIAN_POINT ( 'NONE',  ( 9.169883732660084164, -9.268939115642975679, 1.500000000000001332 ) ) ;
#19490 = CARTESIAN_POINT ( 'NONE',  ( 10.25423333689188077, -17.17121715837755147, 6.518927109361853489 ) ) ;
#19491 = FACE_BOUND ( 'NONE', #887, .T. ) ;
#19492 = DIRECTION ( 'NONE',  ( 0.000000000000000000, 0.000000000000000000, 1.000000000000000000 ) ) ;
#19493 = EDGE_CURVE ( 'NONE', #26671, #20990, #22534, .T. ) ;
#19494 = LINE ( 'NONE', #29008, #974 ) ;
#19495 = B_SPLINE_CURVE_WITH_KNOTS ( 'NONE', 3,
 ( #10968, #814, #12992, #20002, #17986 ),
 .UNSPECIFIED., .F., .F.,
 ( 4, 1, 4 ),
 ( 0.6430105143128194145, 0.6483083546374348582, 0.6536061949620504130 ),
 .UNSPECIFIED. ) ;
#19496 = ORIENTED_EDGE ( 'NONE', *, *, #10148, .F. ) ;
#19497 = ADVANCED_FACE ( 'NONE', ( #8201 ), #27394, .T. ) ;
#19498 = AXIS2_PLACEMENT_3D ( 'NONE', #18840, #26153, #4326 ) ;
#19499 = CARTESIAN_POINT ( 'NONE',  ( -34.17152791855434657, -12.46745445544742381, 34.49999999999998579 ) ) ;
#19500 = DIRECTION ( 'NONE',  ( 0.000000000000000000, 0.000000000000000000, 1.000000000000000000 ) ) ;
#19501 = EDGE_CURVE ( 'NONE', #24485, #21278, #5870, .T. ) ;
#19502 = CARTESIAN_POINT ( 'NONE',  ( 26.31094384852241319, 8.315730187098496984, -16.55003854064094426 ) ) ;
#19503 = ORIENTED_EDGE ( 'NONE', *, *, #26310, .T. ) ;
#19504 = CARTESIAN_POINT ( 'NONE',  ( 15.45804667738991967, 12.71867858434618093, 7.176035686813569292 ) ) ;
#19505 = ORIENTED_EDGE ( 'NONE', *, *, #24631, .T. ) ;
#19506 = CARTESIAN_POINT ( 'NONE',  ( -25.47847050916410439, -26.57182937991348481, 1.500000000000001332 ) ) ;
#19507 = ADVANCED_FACE ( 'NONE', ( #27226 ), #3874, .T. ) ;
#19508 = CARTESIAN_POINT ( 'NONE',  ( 16.59744209609359444, 3.993643014828355486, 18.73314399819311760 ) ) ;
#19509 = CIRCLE ( 'NONE', #13539, 9.084132297865673777 ) ;
#19510 = CARTESIAN_POINT ( 'NONE',  ( 0.000000000000000000, -2.435693370351110282E-15, 21.50000000000000355 ) ) ;
#19511 = VERTEX_POINT ( 'NONE', #3828 ) ;
#19512 = ADVANCED_FACE ( 'NONE', ( #17704 ), #6014, .T. ) ;
#19513 = DIRECTION ( 'NONE',  ( 0.000000000000000000, 0.000000000000000000, 1.000000000000000000 ) ) ;
#19514 = CARTESIAN_POINT ( 'NONE',  ( 0.000000000000000000, 0.000000000000000000, -52.50000000000000000 ) ) ;
#19515 = ORIENTED_EDGE ( 'NONE', *, *, #29806, .T. ) ;
#19516 = CARTESIAN_POINT ( 'NONE',  ( 4.079864335184373303, 39.26151969706030798, 34.49999999999998579 ) ) ;
#19517 = DIRECTION ( 'NONE',  ( -0.000000000000000000, -0.000000000000000000, -1.000000000000000000 ) ) ;
#19518 = CARTESIAN_POINT ( 'NONE',  ( -23.17581250239728519, -34.50630206824672541, 1.499999999999999778 ) ) ;
#19519 = CARTESIAN_POINT ( 'NONE',  ( 10.27641578865089933, -17.15802603149301220, 19.60917204426171878 ) ) ;
#19520 = ORIENTED_EDGE ( 'NONE', *, *, #22532, .T. ) ;
#19521 = B_SPLINE_CURVE_WITH_KNOTS ( 'NONE', 3,
 ( #5616, #17768, #7791, #5141, #9986, #17303, #26835, #24625, #5460, #19490, #3259, #17144, #24321, #609, #24474, #23043, #27288, #18083 ),
 .UNSPECIFIED., .F., .F.,
 ( 4, 2, 2, 2, 2, 2, 2, 2, 4 ),
 ( 0.003174295595554316955, 0.003570702171545545815, 0.003967108747536775108, 0.004363515323528003968, 0.004759921899519232828, 0.005156328475510462556, 0.005552735051501691416, 0.005949141627492920276, 0.006345548203484149136 ),
 .UNSPECIFIED. ) ;
#19522 = AXIS2_PLACEMENT_3D ( 'NONE', #21396, #36, #6457 ) ;
#19523 = CARTESIAN_POINT ( 'NONE',  ( 0.000000000000000000, 80.00000000000000000, 50.49999999999998579 ) ) ;
#19524 = DIRECTION ( 'NONE',  ( -0.000000000000000000, -0.000000000000000000, 1.000000000000000000 ) ) ;
#19525 = EDGE_LOOP ( 'NONE', ( #26224, #19223, #15533, #16231 ) ) ;
#19526 = CARTESIAN_POINT ( 'NONE',  ( 28.00352791766682259, -29.58015274189969901, 12.54700467726770441 ) ) ;
#19527 = CARTESIAN_POINT ( 'NONE',  ( -12.86767874445213877, -1.850092897552710225, 1.500000000000001332 ) ) ;
#19528 = EDGE_CURVE ( 'NONE', #28201, #15417, #10390, .T. ) ;
#19529 = CARTESIAN_POINT ( 'NONE',  ( -14.81512577538152442, 13.43580467474268758, 18.72886616302735163 ) ) ;
#19530 = CARTESIAN_POINT ( 'NONE',  ( 6.899999999999999467, -5.196152422706639129, -9.000000000000000000 ) ) ;
#19531 = EDGE_CURVE ( 'NONE', #5009, #24948, #15521, .T. ) ;
#19532 = CARTESIAN_POINT ( 'NONE',  ( -34.07766914599911701, 21.40380666528009002, -1.500000000000000000 ) ) ;
#19533 = CARTESIAN_POINT ( 'NONE',  ( -1.000000000000008438, 13.00000000000001421, 1.500000000000001332 ) ) ;
#19534 = CARTESIAN_POINT ( 'NONE',  ( 29.78800378361061263, 27.44470329932194019, 34.56933849413994864 ) ) ;
#19535 = CARTESIAN_POINT ( 'NONE',  ( 0.4269445148198162121, -2.969464325642846347, 24.50000000000000000 ) ) ;
#19536 = ORIENTED_EDGE ( 'NONE', *, *, #13572, .T. ) ;
#19537 = DIRECTION ( 'NONE',  ( 0.000000000000000000, -1.132880637372608986E-16, 1.000000000000000000 ) ) ;
#19538 = ORIENTED_EDGE ( 'NONE', *, *, #8981, .T. ) ;
#19539 = DIRECTION ( 'NONE',  ( 0.000000000000000000, 0.000000000000000000, 1.000000000000000000 ) ) ;
#19540 = DIRECTION ( 'NONE',  ( -0.000000000000000000, -0.000000000000000000, 1.000000000000000000 ) ) ;
#19541 = VERTEX_POINT ( 'NONE', #1186 ) ;
#19542 = VERTEX_POINT ( 'NONE', #15051 ) ;
#19543 = CARTESIAN_POINT ( 'NONE',  ( -50.00000000000000000, 0.000000000000000000, -87.50000000000000000 ) ) ;
#19544 = CIRCLE ( 'NONE', #4601, 9.482273699623480212 ) ;
#19545 = ORIENTED_EDGE ( 'NONE', *, *, #5839, .F. ) ;
#19546 = ORIENTED_EDGE ( 'NONE', *, *, #16120, .F. ) ;
#19547 = EDGE_LOOP ( 'NONE', ( #26440, #2896, #21015, #25758 ) ) ;
#19548 = CARTESIAN_POINT ( 'NONE',  ( 12.50000000000000000, 1.530808498934191521E-15, -52.50000000000000000 ) ) ;
#19549 = CARTESIAN_POINT ( 'NONE',  ( -31.11230703446257451, 19.97580969618028846, 34.49999999999998579 ) ) ;
#19550 = DIRECTION ( 'NONE',  ( -0.000000000000000000, -0.000000000000000000, 1.000000000000000000 ) ) ;
#19551 = CARTESIAN_POINT ( 'NONE',  ( 4.819993392704754243, 16.32915940662073595, 18.72771030977187579 ) ) ;
#19552 = CARTESIAN_POINT ( 'NONE',  ( 39.99999999999998579, 80.00000000000001421, 47.49999999999999289 ) ) ;
#19553 = ORIENTED_EDGE ( 'NONE', *, *, #28807, .F. ) ;
#19554 = DIRECTION ( 'NONE',  ( 1.000000000000000000, 0.000000000000000000, 0.000000000000000000 ) ) ;
#19555 = DIRECTION ( 'NONE',  ( 1.000000000000000000, 0.000000000000000000, 0.000000000000000000 ) ) ;
#19556 = CARTESIAN_POINT ( 'NONE',  ( 2.599508007902112006, -14.29059753516471964, 1.500000000000000000 ) ) ;
#19557 = PLANE ( 'NONE',  #21572 ) ;
#19558 = EDGE_LOOP ( 'NONE', ( #29861, #10013, #9424, #26717 ) ) ;
#19559 = CARTESIAN_POINT ( 'NONE',  ( -10.62374177707235035, -16.96647932868177122, 20.34789198813115263 ) ) ;
#19560 = CARTESIAN_POINT ( 'NONE',  ( -14.96594037876678307, -8.187306180225535357, 5.749491821935610147 ) ) ;
#19561 = CARTESIAN_POINT ( 'NONE',  ( -6.803558837019166639, 18.82611028990652358, 6.131018562779544823 ) ) ;
#19562 = VECTOR ( 'NONE', #20495, 1000.000000000000000 ) ;
#19563 = AXIS2_PLACEMENT_3D ( 'NONE', #12508, #7665, #17641 ) ;
#19564 = DIRECTION ( 'NONE',  ( -0.000000000000000000, -0.000000000000000000, -1.000000000000000000 ) ) ;
#19565 = CIRCLE ( 'NONE', #3633, 0.7499999999999997780 ) ;
#19566 = CARTESIAN_POINT ( 'NONE',  ( -15.55662731361435114, -6.910399801605404235, 19.00652017443069752 ) ) ;
#19567 = DIRECTION ( 'NONE',  ( -0.000000000000000000, -0.000000000000000000, -1.000000000000000000 ) ) ;
#19568 = EDGE_LOOP ( 'NONE', ( #21942, #21357, #24181, #9652 ) ) ;
#19569 = ORIENTED_EDGE ( 'NONE', *, *, #25406, .T. ) ;
#19570 = EDGE_CURVE ( 'NONE', #20897, #23537, #7854, .T. ) ;
#19571 = CARTESIAN_POINT ( 'NONE',  ( -5.125804696664928883, 19.33206434738277579, 18.84056766331481825 ) ) ;
#19572 = CARTESIAN_POINT ( 'NONE',  ( -12.70761245252103677, 11.32417831140434039, 6.641371103590088865 ) ) ;
#19573 = CARTESIAN_POINT ( 'NONE',  ( -0.1027882698832301017, -17.02358378464768762, 7.156916968540298463 ) ) ;
#19574 = ORIENTED_EDGE ( 'NONE', *, *, #11161, .T. ) ;
#19575 = PRODUCT_CONTEXT ( 'NONE', #9626, 'mechanical' ) ;
#19576 = DIRECTION ( 'NONE',  ( 0.000000000000000000, 0.000000000000000000, 1.000000000000000000 ) ) ;
#19577 = CARTESIAN_POINT ( 'NONE',  ( 0.000000000000000000, 80.00000000000000000, 50.49999999999998579 ) ) ;
#19578 = ORIENTED_EDGE ( 'NONE', *, *, #16087, .F. ) ;
#19579 = DIRECTION ( 'NONE',  ( -0.000000000000000000, -0.000000000000000000, -1.000000000000000000 ) ) ;
#19580 = DIRECTION ( 'NONE',  ( 0.000000000000000000, 0.000000000000000000, 1.000000000000000000 ) ) ;
#19581 = CARTESIAN_POINT ( 'NONE',  ( 15.57266529552203416, -38.96488032230103471, -1.500000000000000000 ) ) ;
#19582 = CARTESIAN_POINT ( 'NONE',  ( -38.70399152336479176, 5.266273049938332562, 32.13928303338958159 ) ) ;
#19583 = ORIENTED_EDGE ( 'NONE', *, *, #29410, .F. ) ;
#19584 = DIRECTION ( 'NONE',  ( -1.000000000000000000, 0.000000000000000000, 0.000000000000000000 ) ) ;
#19585 = CIRCLE ( 'NONE', #1151, 45.00000000000000711 ) ;
#19586 = VECTOR ( 'NONE', #5841, 1000.000000000000000 ) ;
#19587 = CARTESIAN_POINT ( 'NONE',  ( 11.79327001302698719, 42.17510997215990898, -16.50000000000000355 ) ) ;
#19588 = DIRECTION ( 'NONE',  ( -1.000000000000000000, 0.000000000000000000, 0.000000000000000000 ) ) ;
#19589 = ORIENTED_EDGE ( 'NONE', *, *, #7466, .F. ) ;
#19590 = CARTESIAN_POINT ( 'NONE',  ( -8.090471615930056259, 1.687027447297517080, -1.500000000000001776 ) ) ;
#19591 = CYLINDRICAL_SURFACE ( 'NONE', #9883, 0.7500000000000011102 ) ;
#19592 = DIRECTION ( 'NONE',  ( 0.000000000000000000, 0.000000000000000000, -1.000000000000000000 ) ) ;
#19593 = CARTESIAN_POINT ( 'NONE',  ( 0.7453234696411443760, -17.02803278171227674, 5.651989602109218858 ) ) ;
#19594 = CARTESIAN_POINT ( 'NONE',  ( -47.00000000000000000, 90.00000000000001421, 52.49999999999999289 ) ) ;
#19595 = DIRECTION ( 'NONE',  ( 1.000000000000000000, 0.000000000000000000, 0.000000000000000000 ) ) ;
#19596 = DIRECTION ( 'NONE',  ( 0.000000000000000000, 0.000000000000000000, 1.000000000000000000 ) ) ;
#19597 = CARTESIAN_POINT ( 'NONE',  ( 0.000000000000000000, 0.000000000000000000, 21.50000000000000000 ) ) ;
#19598 = EDGE_LOOP ( 'NONE', ( #3094, #5325, #11181, #8756, #30311, #5515 ) ) ;
#19599 = CARTESIAN_POINT ( 'NONE',  ( 49.99999999999998579, -70.00000000000000000, 12.49999999999999112 ) ) ;
#19600 = VECTOR ( 'NONE', #29689, 999.9999999999998863 ) ;
#19601 = CARTESIAN_POINT ( 'NONE',  ( 29.61203839202725518, -15.40012917324033381, 37.38016955275580244 ) ) ;
#19602 = VERTEX_POINT ( 'NONE', #18031 ) ;
#19603 = ORIENTED_EDGE ( 'NONE', *, *, #10180, .F. ) ;
#19604 = VECTOR ( 'NONE', #7962, 1000.000000000000000 ) ;
#19605 = CARTESIAN_POINT ( 'NONE',  ( 24.03057240117691862, -26.57182937991349903, 1.500000000000000000 ) ) ;
#19606 = CARTESIAN_POINT ( 'NONE',  ( -14.03716236476662615, 47.98954181453471080, -49.68998407197084788 ) ) ;
#19607 = VECTOR ( 'NONE', #471, 1000.000000000000114 ) ;
#19608 = ORIENTED_EDGE ( 'NONE', *, *, #20284, .T. ) ;
#19609 = CARTESIAN_POINT ( 'NONE',  ( 15.48724201788533605, 12.68311944884417919, 18.90679857307105749 ) ) ;
#19610 = CARTESIAN_POINT ( 'NONE',  ( -9.147715168420965881, -14.36154699054607420, 5.940635272151477686 ) ) ;
#19611 = ORIENTED_EDGE ( 'NONE', *, *, #21099, .F. ) ;
#19612 = CARTESIAN_POINT ( 'NONE',  ( -25.64627119138473432, -23.40052582045089480, -16.50001200000000168 ) ) ;
#19613 = CARTESIAN_POINT ( 'NONE',  ( 16.74328840634221649, 3.194145055459935101, 20.34789198813115263 ) ) ;
#19614 = CARTESIAN_POINT ( 'NONE',  ( 40.57663165180618847, 0.1223933743677056846, -16.50000000000000000 ) ) ;
#19615 = VERTEX_POINT ( 'NONE', #17414 ) ;
#19616 = CARTESIAN_POINT ( 'NONE',  ( 23.94669763007064134, -13.17250946182262972, 43.42684587397059204 ) ) ;
#19617 = ORIENTED_EDGE ( 'NONE', *, *, #4610, .F. ) ;
#19618 = VECTOR ( 'NONE', #5299, 1000.000000000000000 ) ;
#19619 = DIRECTION ( 'NONE',  ( -1.000000000000000000, 0.000000000000000000, 0.000000000000000000 ) ) ;
#19620 = CARTESIAN_POINT ( 'NONE',  ( -6.587417658830998946, 18.90298706665744177, 18.56793045041961321 ) ) ;
#19621 = CARTESIAN_POINT ( 'NONE',  ( -12.72607405277288350, 11.30422146305940423, 19.11611934778430921 ) ) ;
#19622 = CARTESIAN_POINT ( 'NONE',  ( -10.45807895166739243, -17.06883091098138649, 18.34838970509067479 ) ) ;
#19623 = CARTESIAN_POINT ( 'NONE',  ( -33.91683774368993198, -20.99019730004604156, 30.97961946053406734 ) ) ;
#19624 = FACE_OUTER_BOUND ( 'NONE', #28730, .T. ) ;
#19625 = DIRECTION ( 'NONE',  ( -0.000000000000000000, 1.132880637372608986E-16, -1.000000000000000000 ) ) ;
#19626 = CARTESIAN_POINT ( 'NONE',  ( -16.99246856547862450, 1.423159825038152970, 5.678370764302467677 ) ) ;
#19627 = CYLINDRICAL_SURFACE ( 'NONE', #3306, 7.500000000000013323 ) ;
#19628 = DIRECTION ( 'NONE',  ( 0.000000000000000000, 0.000000000000000000, 1.000000000000000000 ) ) ;
#19629 = ORIENTED_EDGE ( 'NONE', *, *, #7108, .F. ) ;
#19630 = EDGE_LOOP ( 'NONE', ( #10247, #30082, #14736, #9717, #26739, #442 ) ) ;
#19631 = DIRECTION ( 'NONE',  ( 0.000000000000000000, 0.000000000000000000, 1.000000000000000000 ) ) ;
#19632 = CARTESIAN_POINT ( 'NONE',  ( -4.163336342344337027E-14, 1.387778780781445676E-14, 92.49999999999998579 ) ) ;
#19633 = ADVANCED_FACE ( 'NONE', ( #22232 ), #12896, .F. ) ;
#19634 = CARTESIAN_POINT ( 'NONE',  ( 18.33599632111990374, -7.986941774664180649, 20.34789198813115263 ) ) ;
#19635 = FACE_OUTER_BOUND ( 'NONE', #14770, .T. ) ;
#19636 = CARTESIAN_POINT ( 'NONE',  ( 6.437683520590171682, -6.962021646281551845, 1.500000000000001332 ) ) ;
#19637 = CIRCLE ( 'NONE', #24630, 9.084132297865673777 ) ;
#19638 = CARTESIAN_POINT ( 'NONE',  ( -32.24119442679361214, -26.76047168400493703, -16.50000600000000262 ) ) ;
#19639 = B_SPLINE_CURVE_WITH_KNOTS ( 'NONE', 3,
 ( #16892, #3161, #12685, #14851, #22178, #10330, #19844, #29367, #17508, #27028, #26410, #5036, #21705, #345, #19384, #14691, #4516, #19326 ),
 .UNSPECIFIED., .F., .F.,
 ( 4, 2, 2, 2, 2, 2, 2, 2, 4 ),
 ( 0.000000000000000000, 0.0003967869494442895651, 0.0007935738988885791302, 0.001190360848332868695, 0.001587147797777158260, 0.001983934747221447609, 0.002380721696665737391, 0.002777508646110027173, 0.003174295595554316521 ),
 .UNSPECIFIED. ) ;
#19640 = VERTEX_POINT ( 'NONE', #19908 ) ;
#19641 = CARTESIAN_POINT ( 'NONE',  ( -19.12102597850193675, -33.46912219541083999, 34.50000000000000000 ) ) ;
#19642 = ADVANCED_FACE ( 'NONE', ( #3528, #20047, #5551, #20363, #10688, #10541 ), #707, .F. ) ;
#19643 = DIRECTION ( 'NONE',  ( -0.000000000000000000, -0.000000000000000000, -1.000000000000000000 ) ) ;
#19644 = CARTESIAN_POINT ( 'NONE',  ( 19.77267785325472005, 3.123260753354264452, 5.653912893140659257 ) ) ;
#19645 = ORIENTED_EDGE ( 'NONE', *, *, #11667, .T. ) ;
#19646 = EDGE_CURVE ( 'NONE', #7775, #18617, #11836, .T. ) ;
#19647 = CARTESIAN_POINT ( 'NONE',  ( 13.00026995858111611, 10.98778251907842574, 6.420335371522007506 ) ) ;
#19648 = VERTEX_POINT ( 'NONE', #5701 ) ;
#19649 = CARTESIAN_POINT ( 'NONE',  ( 15.94288127717319981, -6.058927977062421810, 7.603368798681074736 ) ) ;
#19650 = DIRECTION ( 'NONE',  ( -0.000000000000000000, -0.000000000000000000, -1.000000000000000000 ) ) ;
#19651 = CARTESIAN_POINT ( 'NONE',  ( -24.50429677314016175, 7.442113211156452302, 45.14840481399660632 ) ) ;
#19652 = ORIENTED_EDGE ( 'NONE', *, *, #21005, .F. ) ;
#19653 = DIRECTION ( 'NONE',  ( 1.000000000000000000, 0.000000000000000000, 0.000000000000000000 ) ) ;
#19654 = CARTESIAN_POINT ( 'NONE',  ( 0.6210184355499436260, -9.062880100047301823, 21.50000000000000000 ) ) ;
#19655 = DIRECTION ( 'NONE',  ( 1.000000000000000000, 0.000000000000000000, 0.000000000000000000 ) ) ;
#19656 = DIRECTION ( 'NONE',  ( -1.000000000000000000, 0.000000000000000000, 0.000000000000000000 ) ) ;
#19657 = AXIS2_PLACEMENT_3D ( 'NONE', #24913, #22871, #8391 ) ;
#19658 = CARTESIAN_POINT ( 'NONE',  ( -9.268856789657274220, 38.25380398711767072, 34.80090346875804386 ) ) ;
#19659 = CARTESIAN_POINT ( 'NONE',  ( -12.72536390617885260, -2.839914339433650348, 24.50000000000000000 ) ) ;
#19660 = DIRECTION ( 'NONE',  ( 0.000000000000000000, 0.000000000000000000, -1.000000000000000000 ) ) ;
#19661 = EDGE_CURVE ( 'NONE', #24153, #14363, #15195, .T. ) ;
#19662 = VERTEX_POINT ( 'NONE', #3682 ) ;
#19663 = EDGE_CURVE ( 'NONE', #27284, #11315, #2470, .T. ) ;
#19664 = CARTESIAN_POINT ( 'NONE',  ( 0.000000000000000000, -2.435693370351110282E-15, 21.50000000000000355 ) ) ;
#19665 = EDGE_CURVE ( 'NONE', #17265, #21024, #22315, .T. ) ;
#19666 = CARTESIAN_POINT ( 'NONE',  ( -15.97321056478111245, 12.06495093120146578, 19.58863275299554019 ) ) ;
#19667 = CARTESIAN_POINT ( 'NONE',  ( -3.662523238938586001, -12.47340865698848056, 1.500000000000001332 ) ) ;
#19668 = EDGE_CURVE ( 'NONE', #12408, #6787, #12876, .T. ) ;
#19669 = ORIENTED_EDGE ( 'NONE', *, *, #985, .T. ) ;
#19670 = CARTESIAN_POINT ( 'NONE',  ( 32.04552055021039791, -24.22732060750177752, 17.91633598528648719 ) ) ;
#19671 = CARTESIAN_POINT ( 'NONE',  ( -45.40481444351987506, 69.10337004759016111, 60.91566614034201876 ) ) ;
#19672 = EDGE_CURVE ( 'NONE', #2092, #13119, #25957, .T. ) ;
#19673 = CARTESIAN_POINT ( 'NONE',  ( 3.118309183252346628, 17.14266753270391774, 1.500000000000000000 ) ) ;
#19674 = CARTESIAN_POINT ( 'NONE',  ( -1.687027447297492211, -8.840471615930066918, -3.621320343559650379 ) ) ;
#19675 = CARTESIAN_POINT ( 'NONE',  ( -40.89187623478217404, 5.790488632116478129, -19.50000000000000355 ) ) ;
#19676 = EDGE_CURVE ( 'NONE', #4103, #27029, #20508, .T. ) ;
#19677 = SURFACE_SIDE_STYLE ('',( #10170 ) ) ;
#19678 = CARTESIAN_POINT ( 'NONE',  ( 19.71846758372799613, 31.98570203240115717, 37.49999999996673949 ) ) ;
#19679 = EDGE_CURVE ( 'NONE', #11174, #11716, #6477, .T. ) ;
#19680 = DIRECTION ( 'NONE',  ( 0.000000000000000000, 0.000000000000000000, -1.000000000000000000 ) ) ;
#19681 = ORIENTED_EDGE ( 'NONE', *, *, #28902, .F. ) ;
#19682 = CARTESIAN_POINT ( 'NONE',  ( -4.163336342344337027E-14, 1.387778780781445676E-14, 24.50000000000000000 ) ) ;
#19683 = ORIENTED_EDGE ( 'NONE', *, *, #11839, .F. ) ;
#19684 = CARTESIAN_POINT ( 'NONE',  ( -24.35970437652574105, -13.37404834226503070, 42.96778633356041865 ) ) ;
#19685 = SHAPE_REPRESENTATION ( 'Vane Snap Cap', ( #7396 ), #15375 ) ;
#19686 = CARTESIAN_POINT ( 'NONE',  ( -70.00000000000000000, -70.00000000000000000, 12.49999999999999112 ) ) ;
#19687 = VERTEX_POINT ( 'NONE', #18181 ) ;
#19688 = CIRCLE ( 'NONE', #6270, 37.60050224823048381 ) ;
#19689 = VERTEX_POINT ( 'NONE', #11313 ) ;
#19690 = CARTESIAN_POINT ( 'NONE',  ( 1.000000000000008438, 19.97498435543819184, 24.50000000000000000 ) ) ;
#19691 = VERTEX_POINT ( 'NONE', #6318 ) ;
#19692 = DIRECTION ( 'NONE',  ( 0.000000000000000000, 0.000000000000000000, -1.000000000000000000 ) ) ;
#19693 = EDGE_CURVE ( 'NONE', #5849, #9666, #8972, .T. ) ;
#19694 = DIRECTION ( 'NONE',  ( 0.6548607339452782172, -0.7557495743542642641, 0.000000000000000000 ) ) ;
#19695 = CARTESIAN_POINT ( 'NONE',  ( 0.000000000000000000, 0.000000000000000000, 0.000000000000000000 ) ) ;
#19696 = CARTESIAN_POINT ( 'NONE',  ( -35.30770907227059752, 18.09651441509958048, 17.46635781055317338 ) ) ;
#19697 = CARTESIAN_POINT ( 'NONE',  ( 11.80555446153501897, -11.55276080277260320, 1.500000000000000000 ) ) ;
#19698 =( GEOMETRIC_REPRESENTATION_CONTEXT ( 3 ) GLOBAL_UNCERTAINTY_ASSIGNED_CONTEXT ( ( #6438 ) ) GLOBAL_UNIT_ASSIGNED_CONTEXT ( ( #1443, #30274, #6260 ) ) REPRESENTATION_CONTEXT ( 'NONE', 'WORKASPACE' ) );
#19699 = VERTEX_POINT ( 'NONE', #18340 ) ;
#19700 = CARTESIAN_POINT ( 'NONE',  ( -11.35999944890270363, -16.46057145267185007, 6.781503518395074259 ) ) ;
#19701 = PLANE ( 'NONE',  #2635 ) ;
#19702 = SURFACE_STYLE_USAGE ( .BOTH. , #10194 ) ;
#19703 = CARTESIAN_POINT ( 'NONE',  ( 37.99999999999999289, 70.00000000000000000, -34.50000000000000000 ) ) ;
#19704 = ADVANCED_FACE ( 'NONE', ( #4440 ), #13951, .F. ) ;
#19705 = ORIENTED_EDGE ( 'NONE', *, *, #8836, .T. ) ;
#19706 = B_SPLINE_CURVE_WITH_KNOTS ( 'NONE', 3,
 ( #3508, #25327, #17857, #27375, #5995, #3655, #18013, #27522, #6143, #15649, #25161, #13330, #7210, #4255, #28584, #28434 ),
 .UNSPECIFIED., .F., .F.,
 ( 4, 2, 2, 2, 2, 2, 2, 4 ),
 ( 2.980251112119010967E-07, 0.0009280375473568674505, 0.001391907308479688144, 0.001855777069602508947, 0.002319646830725329966, 0.002783516591848150552, 0.003247386352970971137, 0.003711256114093792156 ),
 .UNSPECIFIED. ) ;
#19707 = EDGE_CURVE ( 'NONE', #25448, #30732, #14831, .T. ) ;
#19708 = CARTESIAN_POINT ( 'NONE',  ( -15.10044507415839199, -7.916284227987608446, 7.643931100913408550 ) ) ;
#19709 = CARTESIAN_POINT ( 'NONE',  ( -6.485206790418930112, 15.79815780198025621, 6.892848776733236704 ) ) ;
#19710 = AXIS2_PLACEMENT_3D ( 'NONE', #3052, #19580, #29253 ) ;
#19711 = DIRECTION ( 'NONE',  ( 0.5503133621338236470, 0.8349582046168341209, 0.000000000000000000 ) ) ;
#19712 = CARTESIAN_POINT ( 'NONE',  ( -18.45239215198389715, -7.760673075470068127, 19.00652017443069752 ) ) ;
#19713 = AXIS2_PLACEMENT_3D ( 'NONE', #6412, #29821, #30263 ) ;
#19714 = LINE ( 'NONE', #1009, #10618 ) ;
#19715 = ORIENTED_EDGE ( 'NONE', *, *, #3679, .F. ) ;
#19716 = VERTEX_POINT ( 'NONE', #6767 ) ;
#19717 = LINE ( 'NONE', #28627, #20411 ) ;
#19718 = FACE_OUTER_BOUND ( 'NONE', #24906, .T. ) ;
#19719 = CARTESIAN_POINT ( 'NONE',  ( 0.4053375914187597462, -37.50239422248243670, 37.50000000001958256 ) ) ;
#19720 = DIRECTION ( 'NONE',  ( -1.000000000000000000, -0.000000000000000000, -0.000000000000000000 ) ) ;
#19721 = EDGE_LOOP ( 'NONE', ( #19985, #6498, #27719, #8344, #8479, #24623 ) ) ;
#19722 = PRODUCT_CONTEXT ( 'NONE', #10574, 'mechanical' ) ;
#19723 = CARTESIAN_POINT ( 'NONE',  ( 16.18315216712441895, -5.452792103149284308, 19.08844262864049313 ) ) ;
#19724 = AXIS2_PLACEMENT_3D ( 'NONE', #23673, #2485, #12001 ) ;
#19725 = LINE ( 'NONE', #10214, #6707 ) ;
#19726 = EDGE_LOOP ( 'NONE', ( #21503, #20891, #8623, #4269 ) ) ;
#19727 = CARTESIAN_POINT ( 'NONE',  ( 4.467866064779364876, 16.43745301482979215, 18.44501272782439827 ) ) ;
#19728 = DIRECTION ( 'NONE',  ( -1.000000000000000000, 0.000000000000000000, 0.000000000000000000 ) ) ;
#19729 = CARTESIAN_POINT ( 'NONE',  ( -4.163336342344337027E-14, 1.387778780781445676E-14, 77.49999999999998579 ) ) ;
#19730 = CARTESIAN_POINT ( 'NONE',  ( -34.63718683596842141, -19.58198806418189264, 34.73973886756552076 ) ) ;
#19731 = ORIENTED_EDGE ( 'NONE', *, *, #16501, .T. ) ;
#19732 = FACE_BOUND ( 'NONE', #12973, .T. ) ;
#19733 = CIRCLE ( 'NONE', #14239, 0.6002263538043648428 ) ;
#19734 = ADVANCED_FACE ( 'NONE', ( #1646 ), #2085, .T. ) ;
#19735 = VECTOR ( 'NONE', #20478, 1000.000000000000000 ) ;
#19736 = DIRECTION ( 'NONE',  ( -1.000000000000000000, 0.000000000000000000, -0.000000000000000000 ) ) ;
#19737 = FACE_OUTER_BOUND ( 'NONE', #20504, .T. ) ;
#19738 = ORIENTED_EDGE ( 'NONE', *, *, #15129, .F. ) ;
#19739 = CARTESIAN_POINT ( 'NONE',  ( -18.24419300814587075, -8.237927942618478383, 5.749228751562096562 ) ) ;
#19740 = CARTESIAN_POINT ( 'NONE',  ( 12.24063095261064404, 4.490763173670002217, 1.500000000000001332 ) ) ;
#19741 = FILL_AREA_STYLE ('',( #874 ) ) ;
#19742 = DIRECTION ( 'NONE',  ( -0.000000000000000000, -0.000000000000000000, -1.000000000000000000 ) ) ;
#19743 = CARTESIAN_POINT ( 'NONE',  ( -1.687027447297492211, -8.840471615930066918, -1.500000000000002665 ) ) ;
#19744 = CYLINDRICAL_SURFACE ( 'NONE', #14328, 9.482273699623480212 ) ;
#19745 = CARTESIAN_POINT ( 'NONE',  ( 37.18355798296265391, -12.83305167619315412, 15.73854473963378098 ) ) ;
#19746 = CIRCLE ( 'NONE', #1834, 28.20443790117971261 ) ;
#19747 = DIRECTION ( 'NONE',  ( -0.000000000000000000, -0.000000000000000000, -1.000000000000000000 ) ) ;
#19748 = ORIENTED_EDGE ( 'NONE', *, *, #8281, .T. ) ;
#19749 = CARTESIAN_POINT ( 'NONE',  ( 49.99999999999998579, -50.00000000000000000, 59.49999999999999289 ) ) ;
#19750 = CARTESIAN_POINT ( 'NONE',  ( 2.094186647214743235, -9.248129367672072831, 21.50000000000000000 ) ) ;
#19751 = ORIENTED_EDGE ( 'NONE', *, *, #17186, .F. ) ;
#19752 = EDGE_LOOP ( 'NONE', ( #7059, #22796, #17485, #2653 ) ) ;
#19753 = AXIS2_PLACEMENT_3D ( 'NONE', #20763, #11267, #13477 ) ;
#19754 = CYLINDRICAL_SURFACE ( 'NONE', #23594, 2.000000000000005329 ) ;
#19755 = CARTESIAN_POINT ( 'NONE',  ( -3.420703685013330553, 49.88518064725936796, -40.38700250513966239 ) ) ;
#19756 = AXIS2_PLACEMENT_3D ( 'NONE', #6777, #11320, #6176 ) ;
#19757 = SHAPE_REPRESENTATION_RELATIONSHIP ( 'NONE' , 'NONE' ,  #7129, #574 ) ;
#19758 = ORIENTED_EDGE ( 'NONE', *, *, #13033, .F. ) ;
#19759 = CARTESIAN_POINT ( 'NONE',  ( -32.62510195252448852, -16.87942069704176618, 27.50000000000000711 ) ) ;
#19760 = CARTESIAN_POINT ( 'NONE',  ( 12.98391214946238037, 11.00790965981589231, 19.66989035740801839 ) ) ;
#19761 = ORIENTED_EDGE ( 'NONE', *, *, #30551, .T. ) ;
#19762 = CARTESIAN_POINT ( 'NONE',  ( -19.71764211798356570, 3.454211555243455578, 6.974106381145714018 ) ) ;
#19763 = DIRECTION ( 'NONE',  ( -1.000000000000000000, -0.000000000000000000, -0.000000000000000000 ) ) ;
#19764 = CIRCLE ( 'NONE', #17773, 10.00000000000000000 ) ;
#19765 = CARTESIAN_POINT ( 'NONE',  ( 8.480328572437745294, -4.608906612435629491, 1.500000000000001332 ) ) ;
#19766 = ORIENTED_EDGE ( 'NONE', *, *, #11998, .F. ) ;
#19767 = DIRECTION ( 'NONE',  ( 1.000000000000000000, 0.000000000000000000, 0.000000000000000000 ) ) ;
#19768 = ORIENTED_EDGE ( 'NONE', *, *, #2285, .T. ) ;
#19769 = CARTESIAN_POINT ( 'NONE',  ( 0.6177220288906448697, 39.50000000000000711, 27.50000000000001066 ) ) ;
#19770 = CIRCLE ( 'NONE', #30721, 45.00000000000000711 ) ;
#19771 = VERTEX_POINT ( 'NONE', #25509 ) ;
#19772 = AXIS2_PLACEMENT_3D ( 'NONE', #14089, #25961, #30788 ) ;
#19773 = DIRECTION ( 'NONE',  ( 0.2817325568414296710, -0.9594929736144973687, 0.000000000000000000 ) ) ;
#19774 = CARTESIAN_POINT ( 'NONE',  ( 19.58625041283695367, 4.133291823432031720, 6.995624166085161910 ) ) ;
#19775 = CARTESIAN_POINT ( 'NONE',  ( -12.70761245252103500, 11.32417831140434217, 19.33715507985239412 ) ) ;
#19776 = CIRCLE ( 'NONE', #23268, 27.70876437800068359 ) ;
#19777 = CARTESIAN_POINT ( 'NONE',  ( -23.21352257770656990, -10.78826658734919519, 49.40206402021038201 ) ) ;
#19778 = CARTESIAN_POINT ( 'NONE',  ( -32.73678307250399655, 23.13608884642247787, 30.76341402026043070 ) ) ;
#19779 = CARTESIAN_POINT ( 'NONE',  ( 3.118309183252346628, -17.14266753270391774, -1.500000000000000000 ) ) ;
#19780 = LINE ( 'NONE', #7953, #2407 ) ;
#19781 = ORIENTED_EDGE ( 'NONE', *, *, #3850, .T. ) ;
#19782 = CIRCLE ( 'NONE', #22354, 4.999999999999997335 ) ;
#19783 = CARTESIAN_POINT ( 'NONE',  ( -17.01654212181477277, 1.203597991882926710, 5.749491821935610147 ) ) ;
#19784 = B_SPLINE_CURVE_WITH_KNOTS ( 'NONE', 3,
 ( #10697, #8210, #24574, #17712, #25045, #22239, #5869, #5709, #20203, #10399, #15369, #13053, #22544 ),
 .UNSPECIFIED., .F., .F.,
 ( 4, 2, 2, 2, 1, 2, 4 ),
 ( 0.2233868814791938606, 0.2366521944267142574, 0.2499175073742346820, 0.2532338356111147881, 0.2565501638479948943, 0.2631828203217550510, 0.2764481332692754756 ),
 .UNSPECIFIED. ) ;
#19785 = AXIS2_PLACEMENT_3D ( 'NONE', #20770, #23110, #6595 ) ;
#19786 = DIRECTION ( 'NONE',  ( 0.000000000000000000, 1.000000000000000000, 0.000000000000000000 ) ) ;
#19787 = CARTESIAN_POINT ( 'NONE',  ( -9.824744466605366711, -8.513189541288717521, 24.50000000000000000 ) ) ;
#19788 = AXIS2_PLACEMENT_3D ( 'NONE', #27168, #24504, #3149 ) ;
#19789 = LINE ( 'NONE', #17299, #27359 ) ;
#19790 = ORIENTED_EDGE ( 'NONE', *, *, #18495, .T. ) ;
#19791 = EDGE_LOOP ( 'NONE', ( #22439, #17766, #14615, #19883, #9047, #5635 ) ) ;
#19792 = CARTESIAN_POINT ( 'NONE',  ( 18.22972622987023783, -8.227512309863355355, 20.32243167357988511 ) ) ;
#19793 = CLOSED_SHELL ( 'NONE', ( #20245, #13276, #9571, #26526, #10896, #24592, #26151, #2943, #3686, #9327, #20061, #14323, #10495, #16559, #8988, #26907, #16711, #19472, #4444, #8979, #3523, #11490, #29558, #21399, #23652, #23895, #22099, #26770, #28035, #20805, #12244, #8641, #597, #2423, #21740, #22123, #14563, #22318, #23854, #26212, #10713, #9807, #12111, #23247, #5928, #1449, #11112, #30389, #1761, #20276, #18559, #4273, #28847, #18556, #21789, #12835, #7572, #20063, #10505, #6349, #751, #21739, #14362, #13205, #17962, #11941, #23399, #22761, #15846, #18524, #791, #18694, #9746, #24061, #26511, #14487, #21232, #9375, #2924, #21135, #3642, #10666, #25733, #27694, #1383, #1177 ) ) ;
#19794 = CARTESIAN_POINT ( 'NONE',  ( -5.544451646083597751, 16.11829163520482666, 7.652108011868850035 ) ) ;
#19795 = ORIENTED_EDGE ( 'NONE', *, *, #6690, .F. ) ;
#19796 = CARTESIAN_POINT ( 'NONE',  ( -6.974883619896829146, -5.687793815610328707, 21.50000000000000000 ) ) ;
#19797 = AXIS2_PLACEMENT_3D ( 'NONE', #21955, #585, #10105 ) ;
#19798 = DIRECTION ( 'NONE',  ( 0.000000000000000000, 1.000000000000000000, 0.000000000000000000 ) ) ;
#19799 = AXIS2_PLACEMENT_3D ( 'NONE', #15671, #3209, #6169 ) ;
#19800 = CARTESIAN_POINT ( 'NONE',  ( -37.16608720827707657, 36.86186943028246787, 12.49999999999999112 ) ) ;
#19801 = ORIENTED_EDGE ( 'NONE', *, *, #17374, .T. ) ;
#19802 = CIRCLE ( 'NONE', #15244, 2.061368542273053883 ) ;
#19803 = CARTESIAN_POINT ( 'NONE',  ( -9.752241470433741455, -17.46128603886499420, 19.85730954408916915 ) ) ;
#19804 = CARTESIAN_POINT ( 'NONE',  ( -17.92585835919032178, -8.870080556897411483, 18.37545668562167478 ) ) ;
#19805 = EDGE_CURVE ( 'NONE', #20793, #4103, #14263, .T. ) ;
#19806 = CARTESIAN_POINT ( 'NONE',  ( 4.049916833591940879, 16.55712665779027049, 7.652108011868850923 ) ) ;
#19807 = ORIENTED_EDGE ( 'NONE', *, *, #22807, .F. ) ;
#19808 = CARTESIAN_POINT ( 'NONE',  ( 13.01739631533119201, 10.96666867565305736, 6.641371103590088865 ) ) ;
#19809 = ORIENTED_EDGE ( 'NONE', *, *, #29614, .T. ) ;
#19810 = VECTOR ( 'NONE', #19993, 1000.000000000000000 ) ;
#19811 = CARTESIAN_POINT ( 'NONE',  ( 18.73275811567551230, -7.056106374802665115, 6.782048567692550378 ) ) ;
#19812 = AXIS2_PLACEMENT_3D ( 'NONE', #6659, #11360, #9014 ) ;
#19813 = DIRECTION ( 'NONE',  ( 0.000000000000000000, 0.000000000000000000, -1.000000000000000000 ) ) ;
#19814 = DIRECTION ( 'NONE',  ( -0.8412535328311884220, -0.5406408174555862312, 0.000000000000000000 ) ) ;
#19815 = AXIS2_PLACEMENT_3D ( 'NONE', #18646, #9444, #18500 ) ;
#19816 = EDGE_LOOP ( 'NONE', ( #20979, #17555, #8462, #6615, #13797 ) ) ;
#19817 = EDGE_CURVE ( 'NONE', #13440, #29598, #30332, .T. ) ;
#19818 = CARTESIAN_POINT ( 'NONE',  ( -4.776122516674677878E-15, -42.50000000000000000, 1.500000000000000000 ) ) ;
#19819 = EDGE_CURVE ( 'NONE', #19699, #2517, #1499, .T. ) ;
#19820 = LINE ( 'NONE', #7986, #29525 ) ;
#19821 = DIRECTION ( 'NONE',  ( 0.000000000000000000, 0.000000000000000000, 1.000000000000000000 ) ) ;
#19822 = CARTESIAN_POINT ( 'NONE',  ( 31.45274955328486399, 26.35877938677919374, -8.166661938643251517 ) ) ;
#19823 = CIRCLE ( 'NONE', #10368, 0.6002263538043648428 ) ;
#19824 = AXIS2_PLACEMENT_3D ( 'NONE', #27851, #18636, #1946 ) ;
#19825 = CARTESIAN_POINT ( 'NONE',  ( -9.268856789657274220, 38.25380398711767072, 27.50000000000000355 ) ) ;
#19826 = CARTESIAN_POINT ( 'NONE',  ( 9.252152043196039344, -14.29436518012014545, 20.05479082170252525 ) ) ;
#19827 = DIRECTION ( 'NONE',  ( -0.000000000000000000, 1.132880637372608986E-16, -1.000000000000000000 ) ) ;
#19828 = VERTEX_POINT ( 'NONE', #27993 ) ;
#19829 = CARTESIAN_POINT ( 'NONE',  ( -24.86084284002701494, -6.930828199065639517, 49.19141369485819126 ) ) ;
#19830 = DIRECTION ( 'NONE',  ( 1.000000000000000000, 0.000000000000000000, 0.000000000000000000 ) ) ;
#19831 = CARTESIAN_POINT ( 'NONE',  ( -15.50193441389835414, 12.66492269502747980, 18.37415474056476938 ) ) ;
#19832 = LINE ( 'NONE', #5491, #2356 ) ;
#19833 = ADVANCED_FACE ( 'NONE', ( #4130 ), #3987, .F. ) ;
#19834 = CARTESIAN_POINT ( 'NONE',  ( 28.84973994773175576, -28.59864475962095653, 10.18777785223225507 ) ) ;
#19835 = AXIS2_PLACEMENT_3D ( 'NONE', #3261, #930, #5619 ) ;
#19836 = DIRECTION ( 'NONE',  ( 1.000000000000000000, 0.000000000000000000, 0.000000000000000000 ) ) ;
#19837 = LINE ( 'NONE', #29361, #26798 ) ;
#19838 = CARTESIAN_POINT ( 'NONE',  ( 0.000000000000000000, 0.000000000000000000, -1.500000000000000000 ) ) ;
#19839 = CIRCLE ( 'NONE', #12887, 7.500000000000013323 ) ;
#19840 = CARTESIAN_POINT ( 'NONE',  ( -2.687479363073305372, 44.39187623477332068, -19.50000000000000355 ) ) ;
#19841 = AXIS2_PLACEMENT_3D ( 'NONE', #26863, #20136, #25278 ) ;
#19842 = CARTESIAN_POINT ( 'NONE',  ( 3.474270935886293987, -15.38174572367601911, 24.50000000000000000 ) ) ;
#19843 = CARTESIAN_POINT ( 'NONE',  ( 16.74250988114178185, 3.198928528055117848, 5.652196082368483587 ) ) ;
#19844 = CARTESIAN_POINT ( 'NONE',  ( 19.58194293052863344, 4.068188588073704537, 6.149077423860700442 ) ) ;
#19845 = ORIENTED_EDGE ( 'NONE', *, *, #20427, .T. ) ;
#19846 = CARTESIAN_POINT ( 'NONE',  ( 27.03074382657074537, 6.449748410230989215, 42.96778633356034760 ) ) ;
#19847 = CIRCLE ( 'NONE', #16356, 11.99999999999998934 ) ;
#19848 = DIRECTION ( 'NONE',  ( 1.000000000000000000, 0.000000000000000000, 0.000000000000000000 ) ) ;
#19849 = PLANE ( 'NONE',  #29408 ) ;
#19850 = VERTEX_POINT ( 'NONE', #6624 ) ;
#19851 = EDGE_CURVE ( 'NONE', #17197, #1661, #25655, .T. ) ;
#19852 = ORIENTED_EDGE ( 'NONE', *, *, #24823, .F. ) ;
#19853 = EDGE_CURVE ( 'NONE', #8048, #8571, #2405, .T. ) ;
#19854 = CARTESIAN_POINT ( 'NONE',  ( -9.752241470433746784, -17.46128603886497643, 7.161525567826878103 ) ) ;
#19855 = EDGE_LOOP ( 'NONE', ( #22591, #11648, #23517, #132 ) ) ;
#19856 = CARTESIAN_POINT ( 'NONE',  ( 0.7070334246189989846, -17.02861022043351724, 18.34969686940295830 ) ) ;
#19857 = AXIS2_PLACEMENT_3D ( 'NONE', #25677, #6645, #11492 ) ;
#19858 = CARTESIAN_POINT ( 'NONE',  ( -21.52174834036059181, 31.67861116925338294, 34.49999999999998579 ) ) ;
#19859 = EDGE_CURVE ( 'NONE', #1364, #1974, #7389, .T. ) ;
#19860 = DIRECTION ( 'NONE',  ( -0.000000000000000000, 0.000000000000000000, 1.000000000000000000 ) ) ;
#19861 = AXIS2_PLACEMENT_3D ( 'NONE', #29182, #15285, #5322 ) ;
#19862 = CARTESIAN_POINT ( 'NONE',  ( -37.16166377660026399, 12.90791798474662500, 10.22883689759567538 ) ) ;
#19863 = DIRECTION ( 'NONE',  ( -0.000000000000000000, 1.132880637372608986E-16, -1.000000000000000000 ) ) ;
#19864 = CIRCLE ( 'NONE', #14380, 0.7499999999999997780 ) ;
#19865 = AXIS2_PLACEMENT_3D ( 'NONE', #19182, #28705, #20073 ) ;
#19866 = VERTEX_POINT ( 'NONE', #14709 ) ;
#19867 = EDGE_CURVE ( 'NONE', #27304, #17934, #12077, .T. ) ;
#19868 = LINE ( 'NONE', #1302, #17872 ) ;
#19869 = CARTESIAN_POINT ( 'NONE',  ( 19.74251403343738076, 3.198927889078825970, 18.34798005863226678 ) ) ;
#19870 = CARTESIAN_POINT ( 'NONE',  ( 12.20938699334972277, 11.90340052968385365, 20.32367522806703874 ) ) ;
#19871 = LINE ( 'NONE', #7717, #4659 ) ;
#19872 = EDGE_CURVE ( 'NONE', #28669, #1242, #12532, .T. ) ;
#19873 = ORIENTED_EDGE ( 'NONE', *, *, #7813, .T. ) ;
#19874 = EDGE_CURVE ( 'NONE', #4888, #4677, #16335, .T. ) ;
#19875 = CARTESIAN_POINT ( 'NONE',  ( -9.321015140911132590, -14.24452793913984294, 19.77662771831109367 ) ) ;
#19876 = DIRECTION ( 'NONE',  ( 0.000000000000000000, 1.000000000000000000, 1.193512090021232842E-16 ) ) ;
#19877 = CARTESIAN_POINT ( 'NONE',  ( -6.300265418930216299, 19.00075578015505684, 5.704143890883081269 ) ) ;
#19878 = EDGE_CURVE ( 'NONE', #19148, #897, #12353, .T. ) ;
#19879 = CYLINDRICAL_SURFACE ( 'NONE', #10798, 2.898871837527149165 ) ;
#19880 = CARTESIAN_POINT ( 'NONE',  ( 19.64114023396890829, 37.13592150528549496, -1.500000000000000000 ) ) ;
#19881=STYLED_ITEM('',(#30900),#13239);
#19882 = CARTESIAN_POINT ( 'NONE',  ( 33.48316501811951440, -9.771059948263138395, 35.87773437053935055 ) ) ;
#19883 = ORIENTED_EDGE ( 'NONE', *, *, #16264, .F. ) ;
#19884 = ORIENTED_EDGE ( 'NONE', *, *, #2506, .F. ) ;
#19885 = SHAPE_REPRESENTATION ( 'MAS-342', ( #12908, #421, #20352, #22350, #19857, #18386, #13397, #2925, #17869, #30321, #1934, #30805, #10895, #29328, #15879 ), #12384 ) ;
#19886 = DIRECTION ( 'NONE',  ( -0.9594929736144975907, 0.2817325568414293380, 0.000000000000000000 ) ) ;
#19887 = CARTESIAN_POINT ( 'NONE',  ( 0.000000000000000000, 0.000000000000000000, 21.50000000000000000 ) ) ;
#19888 = CARTESIAN_POINT ( 'NONE',  ( -12.81506474335657586, 11.20733750501348069, 6.111214848085761986 ) ) ;
#19889 = FACE_OUTER_BOUND ( 'NONE', #15416, .T. ) ;
#19890 = ORIENTED_EDGE ( 'NONE', *, *, #11520, .F. ) ;
#19891 = LINE ( 'NONE', #26607, #25875 ) ;
#19892 = CIRCLE ( 'NONE', #7942, 32.32717498572574755 ) ;
#19893 = DIRECTION ( 'NONE',  ( 0.000000000000000000, 0.000000000000000000, 1.000000000000000000 ) ) ;
#19894 = EDGE_CURVE ( 'NONE', #5002, #13097, #11380, .T. ) ;
#19895 = ORIENTED_EDGE ( 'NONE', *, *, #5801, .T. ) ;
#19896 = CARTESIAN_POINT ( 'NONE',  ( 4.370315982788584463, 16.46653586241585998, 18.39701043959520987 ) ) ;
#19897 = ADVANCED_FACE ( 'NONE', ( #2866 ), #5208, .F. ) ;
#19898 = CIRCLE ( 'NONE', #23866, 0.7499999999999997780 ) ;
#19899 = FACE_OUTER_BOUND ( 'NONE', #23651, .T. ) ;
#19900 = ADVANCED_FACE ( 'NONE', ( #65 ), #16741, .F. ) ;
#19901 = CARTESIAN_POINT ( 'NONE',  ( -29.21234432035051753, -23.52169588460707672, 37.50000000003778666 ) ) ;
#19902 = VERTEX_POINT ( 'NONE', #2564 ) ;
#19903 = CARTESIAN_POINT ( 'NONE',  ( 24.03057240117691862, 26.57182937991349903, -6.500000000000000888 ) ) ;
#19904 = EDGE_CURVE ( 'NONE', #18015, #7211, #7882, .T. ) ;
#19905 = EDGE_CURVE ( 'NONE', #25203, #509, #22811, .T. ) ;
#19906 = CYLINDRICAL_SURFACE ( 'NONE', #22992, 32.32717498572574755 ) ;
#19907 = CIRCLE ( 'NONE', #17930, 0.7499999999999988898 ) ;
#19908 = CARTESIAN_POINT ( 'NONE',  ( 30.31220697679117038, 11.23460505553742550, -1.500000000000000000 ) ) ;
#19909 = CARTESIAN_POINT ( 'NONE',  ( -9.824744466605366711, -8.513189541288717521, 1.500000000000001332 ) ) ;
#19910 = VERTEX_POINT ( 'NONE', #9723 ) ;
#19911 = DIRECTION ( 'NONE',  ( -0.4154150130018973153, -0.9096319953545134451, 0.000000000000000000 ) ) ;
#19912 = CARTESIAN_POINT ( 'NONE',  ( 12.44591117081739817, 11.64178973126078454, 20.34789198813115974 ) ) ;
#19913 = DIRECTION ( 'NONE',  ( 0.000000000000000000, 0.000000000000000000, -1.000000000000000000 ) ) ;
#19914 = EDGE_CURVE ( 'NONE', #8742, #26694, #3970, .T. ) ;
#19915 = CARTESIAN_POINT ( 'NONE',  ( 0.000000000000000000, -2.435693370351110282E-15, 21.50000000000000355 ) ) ;
#19916 = CARTESIAN_POINT ( 'NONE',  ( -7.028330626922778990, 10.93629592680536788, 1.500000000000001332 ) ) ;
#19917 = CARTESIAN_POINT ( 'NONE',  ( -12.72536390617885260, -2.839914339433650348, 1.500000000000001332 ) ) ;
#19918 = CARTESIAN_POINT ( 'NONE',  ( 37.94189864131114120, -9.832916137336869866, 12.30666522825201170 ) ) ;
#19919 = DIRECTION ( 'NONE',  ( 0.000000000000000000, 1.000000000000000000, 1.132880637372608986E-16 ) ) ;
#19920 = ORIENTED_EDGE ( 'NONE', *, *, #4464, .F. ) ;
#19921 = DIRECTION ( 'NONE',  ( 1.000000000000000000, 0.000000000000000000, 0.000000000000000000 ) ) ;
#19922 = CIRCLE ( 'NONE', #4470, 20.00000000000000355 ) ;
#19923 = LINE ( 'NONE', #2930, #14053 ) ;
#19924 = VERTEX_POINT ( 'NONE', #22355 ) ;
#19925 = ORIENTED_EDGE ( 'NONE', *, *, #27287, .F. ) ;
#19926 = DIRECTION ( 'NONE',  ( -0.000000000000000000, 0.000000000000000000, 1.000000000000000000 ) ) ;
#19927 = EDGE_CURVE ( 'NONE', #16535, #29624, #9362, .T. ) ;
#19928 = CARTESIAN_POINT ( 'NONE',  ( -4.225000340904450091E-15, 7.351593252548064505, 5.266666970006215642 ) ) ;
#19929 = ADVANCED_FACE ( 'NONE', ( #12700 ), #15166, .T. ) ;
#19930 = CIRCLE ( 'NONE', #10965, 1.000000000000000888 ) ;
#19931 = CARTESIAN_POINT ( 'NONE',  ( 15.55295851173241672, 12.60248606922869463, 19.45164628100866722 ) ) ;
#19932 = ORIENTED_EDGE ( 'NONE', *, *, #10266, .T. ) ;
#19933 = ORIENTED_EDGE ( 'NONE', *, *, #27507, .T. ) ;
#19934 = FACE_OUTER_BOUND ( 'NONE', #6452, .T. ) ;
#19935 = CARTESIAN_POINT ( 'NONE',  ( 17.96688762764193470, -8.785985129476816979, 6.144783687052512988 ) ) ;
#19936 = CARTESIAN_POINT ( 'NONE',  ( 18.33792385446292528, -7.982495159855863776, 5.652196082369963293 ) ) ;
#19937 = VERTEX_POINT ( 'NONE', #27193 ) ;
#19938 = CYLINDRICAL_SURFACE ( 'NONE', #12352, 11.99999999999998934 ) ;
#19939 = VECTOR ( 'NONE', #3167, 1000.000000000000000 ) ;
#19940 = CARTESIAN_POINT ( 'NONE',  ( -16.82262805705560993, 2.599658093694372063, 19.66962785902261501 ) ) ;
#19941 = ORIENTED_EDGE ( 'NONE', *, *, #19288, .T. ) ;
#19942 = SURFACE_STYLE_USAGE ( .BOTH. , #17598 ) ;
#19943 = CARTESIAN_POINT ( 'NONE',  ( 14.89473990422475680, -17.79239818699420539, -1.500000000000000000 ) ) ;
#19944 = CARTESIAN_POINT ( 'NONE',  ( 42.49999999999998579, -50.00000000000000000, 12.49999999999999112 ) ) ;
#19945 = CARTESIAN_POINT ( 'NONE',  ( -13.38159811102998376, 10.55828946469181773, 18.34798005862930736 ) ) ;
#19946 = VECTOR ( 'NONE', #21870, 1000.000000000000000 ) ;
#19947 = DIRECTION ( 'NONE',  ( -0.000000000000000000, -0.000000000000000000, -1.000000000000000000 ) ) ;
#19948 = CARTESIAN_POINT ( 'NONE',  ( -2.584357522460066559, 42.42979574273064713, 28.84576176055872665 ) ) ;
#19949 = DIRECTION ( 'NONE',  ( 0.000000000000000000, 0.000000000000000000, 1.000000000000000000 ) ) ;
#19950 = CARTESIAN_POINT ( 'NONE',  ( -0.7083562926194498788, 9.056472324687614872, -1.500000000000000666 ) ) ;
#19951 = VERTEX_POINT ( 'NONE', #5513 ) ;
#19952 = CARTESIAN_POINT ( 'NONE',  ( 11.08678458728283189, -16.66722406908985477, 5.651989602109218858 ) ) ;
#19953 = CARTESIAN_POINT ( 'NONE',  ( 0.000000000000000000, 0.000000000000000000, -87.50000000000000000 ) ) ;
#19954 = DIRECTION ( 'NONE',  ( 1.000000000000000000, 0.000000000000000000, 0.000000000000000000 ) ) ;
#19955 = EDGE_LOOP ( 'NONE', ( #12607, #4094 ) ) ;
#19956 = VERTEX_POINT ( 'NONE', #27357 ) ;
#19957 = DIRECTION ( 'NONE',  ( 0.000000000000000000, 0.000000000000000000, -1.000000000000000000 ) ) ;
#19958 = DIRECTION ( 'NONE',  ( -0.7557495743542581579, -0.6548607339452852116, 0.000000000000000000 ) ) ;
#19959 = PLANE ( 'NONE',  #10872 ) ;
#19960 = ORIENTED_EDGE ( 'NONE', *, *, #19457, .F. ) ;
#19961 = CARTESIAN_POINT ( 'NONE',  ( 0.000000000000000000, -2.435693370351110282E-15, 21.50000000000000355 ) ) ;
#19962 = VECTOR ( 'NONE', #6685, 1000.000000000000000 ) ;
#19963 = CARTESIAN_POINT ( 'NONE',  ( -0.6210184355500070197, 9.062880100047294718, 21.50000000000000000 ) ) ;
#19964 = EDGE_CURVE ( 'NONE', #16535, #12192, #15324, .T. ) ;
#19965 = CARTESIAN_POINT ( 'NONE',  ( 8.616279238414451314, -7.781333699927420966, 1.500000000000000000 ) ) ;
#19966 = ORIENTED_EDGE ( 'NONE', *, *, #2882, .T. ) ;
#19967 = CARTESIAN_POINT ( 'NONE',  ( -9.635826629942098265, -17.52571954072712757, 19.21940439362673203 ) ) ;
#19968 = CARTESIAN_POINT ( 'NONE',  ( 12.30438418247799426, 11.79938075381829421, 5.652605728828373977 ) ) ;
#19969 = CARTESIAN_POINT ( 'NONE',  ( 19.89137488457043901, 2.247671665613723668, 6.310736198168394928 ) ) ;
#19970 = ORIENTED_EDGE ( 'NONE', *, *, #12618, .T. ) ;
#19971 = DIRECTION ( 'NONE',  ( -0.000000000000000000, -0.000000000000000000, 1.000000000000000000 ) ) ;
#19972 = ORIENTED_EDGE ( 'NONE', *, *, #6576, .T. ) ;
#19973 = CARTESIAN_POINT ( 'NONE',  ( 3.395021109945021376, 30.50000000000000000, 24.50000000000000000 ) ) ;
#19974 = DIRECTION ( 'NONE',  ( -0.000000000000000000, 1.000000000000000000, -0.000000000000000000 ) ) ;
#19975 = ORIENTED_EDGE ( 'NONE', *, *, #18931, .T. ) ;
#19976 = CARTESIAN_POINT ( 'NONE',  ( 3.338654329031698342, 16.73860904129764648, 5.951255046771932733 ) ) ;
#19977 = AXIS2_PLACEMENT_3D ( 'NONE', #10188, #19550, #12854 ) ;
#19978 = CARTESIAN_POINT ( 'NONE',  ( 23.21352257770656990, 10.78826658734920230, 49.40206402021032517 ) ) ;
#19979 = DIRECTION ( 'NONE',  ( 0.000000000000000000, 0.6368814469962913449, -0.7709617516270896864 ) ) ;
#19980 = FACE_OUTER_BOUND ( 'NONE', #1523, .T. ) ;
#19981 = AXIS2_PLACEMENT_3D ( 'NONE', #5414, #29275, #17423 ) ;
#19982 = CARTESIAN_POINT ( 'NONE',  ( -21.86019681245148405, 31.48592878035298170, 27.50000000000001776 ) ) ;
#19983 = CARTESIAN_POINT ( 'NONE',  ( 9.402326492558371385, -14.20083561530969263, 20.19668224736330941 ) ) ;
#19984 = CARTESIAN_POINT ( 'NONE',  ( 31.22486525274645430, 15.32888848509420043, 40.21560466201665918 ) ) ;
#19985 = ORIENTED_EDGE ( 'NONE', *, *, #11708, .F. ) ;
#19986 = CARTESIAN_POINT ( 'NONE',  ( 26.81368379037234817, 6.366017791192971842, 47.44099319977354412 ) ) ;
#19987 = CARTESIAN_POINT ( 'NONE',  ( -14.01100295375883498, 9.765235586930179679, 19.36813350477385143 ) ) ;
#19988 = CARTESIAN_POINT ( 'NONE',  ( 44.92383873364811819, 68.80441998829734018, 61.21192490580749990 ) ) ;
#19989 = CARTESIAN_POINT ( 'NONE',  ( 0.09318607064769342252, 1.767053008364804167, 9.000000000000000000 ) ) ;
#19990 = VERTEX_POINT ( 'NONE', #24381 ) ;
#19991 = CARTESIAN_POINT ( 'NONE',  ( 31.30722686493686524, -25.34759660530392367, 17.71607651522528570 ) ) ;
#19992 = CARTESIAN_POINT ( 'NONE',  ( 0.000000000000000000, 0.000000000000000000, 21.50000000000000000 ) ) ;
#19993 = DIRECTION ( 'NONE',  ( -0.000000000000000000, -0.000000000000000000, -1.000000000000000000 ) ) ;
#19994 = DIRECTION ( 'NONE',  ( 0.000000000000000000, -1.132880637372608986E-16, 1.000000000000000000 ) ) ;
#19995 = DIRECTION ( 'NONE',  ( 1.000000000000000000, 0.000000000000000000, 0.000000000000000000 ) ) ;
#19996 = DIRECTION ( 'NONE',  ( 0.000000000000000000, 0.000000000000000000, 1.000000000000000000 ) ) ;
#19997 = CARTESIAN_POINT ( 'NONE',  ( 8.838492628486433134, 36.51832121211318594, 37.49999999994788169 ) ) ;
#19998 = EDGE_LOOP ( 'NONE', ( #13343, #12660, #11752, #11028 ) ) ;
#19999 = AXIS2_PLACEMENT_3D ( 'NONE', #10551, #17890, #3691 ) ;
#20000 = CARTESIAN_POINT ( 'NONE',  ( -33.56830061431172396, -10.30497729095454851, 35.64318943580060761 ) ) ;
#20001 = LINE ( 'NONE', #27183, #6245 ) ;
#20002 = CARTESIAN_POINT ( 'NONE',  ( 33.53984941789958896, 24.80927308773734197, -16.50000000000000355 ) ) ;
#20003 = VERTEX_POINT ( 'NONE', #3491 ) ;
#20004 = VERTEX_POINT ( 'NONE', #13006 ) ;
#20005 = DIRECTION ( 'NONE',  ( 1.000000000000000000, 0.000000000000000000, 0.000000000000000000 ) ) ;
#20006 = AXIS2_PLACEMENT_3D ( 'NONE', #5381, #12562, #22055 ) ;
#20007 = ORIENTED_EDGE ( 'NONE', *, *, #23006, .T. ) ;
#20008 = DIRECTION ( 'NONE',  ( -0.000000000000000000, 0.000000000000000000, 1.000000000000000000 ) ) ;
#20009 = DIRECTION ( 'NONE',  ( 0.000000000000000000, 1.000000000000000000, -0.000000000000000000 ) ) ;
#20010 = CIRCLE ( 'NONE', #13550, 9.482273699623480212 ) ;
#20011 = CARTESIAN_POINT ( 'NONE',  ( 19.18576292979354392, -22.55620591602728453, 1.500000000000000000 ) ) ;
#20012 = CARTESIAN_POINT ( 'NONE',  ( 37.99999999999999289, 209.2686044187655909, -75.50000000000001421 ) ) ;
#20013 = CARTESIAN_POINT ( 'NONE',  ( -9.824744466605366711, -8.513189541288717521, 1.500000000000001332 ) ) ;
#20014 = CARTESIAN_POINT ( 'NONE',  ( -10.73812863781237681, -16.87327681817511404, 7.626647697317578078 ) ) ;
#20015 = CARTESIAN_POINT ( 'NONE',  ( 19.91398265452213678, -1.852915226174634444, 1.500000000000001332 ) ) ;
#20016 = DIRECTION ( 'NONE',  ( -0.000000000000000000, -0.000000000000000000, -1.000000000000000000 ) ) ;
#20017 = ORIENTED_EDGE ( 'NONE', *, *, #27745, .F. ) ;
#20018 = AXIS2_PLACEMENT_3D ( 'NONE', #6012, #3361, #15519 ) ;
#20019 = CARTESIAN_POINT ( 'NONE',  ( -11.36561296172221169, -16.47845303048202936, 19.22654678686458141 ) ) ;
#20020 = CARTESIAN_POINT ( 'NONE',  ( -17.67332396526446203, -9.400239829055445639, 7.196036389296800451 ) ) ;
#20021 = CARTESIAN_POINT ( 'NONE',  ( 0.000000000000000000, 0.000000000000000000, 1.500000000000000000 ) ) ;
#20022 = CARTESIAN_POINT ( 'NONE',  ( 11.30587609449920272, -16.51930395566529697, 5.678370764302467677 ) ) ;
#20023 = EDGE_CURVE ( 'NONE', #25701, #27848, #12546, .T. ) ;
#20024 = EDGE_CURVE ( 'NONE', #23909, #23911, #20820, .T. ) ;
#20025 = CARTESIAN_POINT ( 'NONE',  ( -8.159193615868369776, 3.993622308618967498, 21.50000000000000000 ) ) ;
#20026 = CARTESIAN_POINT ( 'NONE',  ( -5.738360882150002062, -7.548823014270625187, 1.500000000000001332 ) ) ;
#20027 = VERTEX_POINT ( 'NONE', #10189 ) ;
#20028 = EDGE_CURVE ( 'NONE', #12636, #11838, #8806, .T. ) ;
#20029 = ORIENTED_EDGE ( 'NONE', *, *, #4404, .F. ) ;
#20030 = CARTESIAN_POINT ( 'NONE',  ( -31.10500197267670330, 15.38309308716405077, 36.05646065676234002 ) ) ;
#20031 = CARTESIAN_POINT ( 'NONE',  ( 39.00000000000000000, 5.563236990218597633, -1.500000000000000000 ) ) ;
#20032 = CARTESIAN_POINT ( 'NONE',  ( -14.83674576813424473, 13.43848929326658315, 6.018569869498933578 ) ) ;
#20033 = EDGE_CURVE ( 'NONE', #29057, #7554, #4807, .T. ) ;
#20034 = FACE_OUTER_BOUND ( 'NONE', #2935, .T. ) ;
#20035 = ORIENTED_EDGE ( 'NONE', *, *, #27893, .F. ) ;
#20036 = CARTESIAN_POINT ( 'NONE',  ( 25.19442432474404470, 35.44676296256560022, -19.50000000000000355 ) ) ;
#20037 = EDGE_CURVE ( 'NONE', #29034, #5009, #4241, .T. ) ;
#20038 = ORIENTED_EDGE ( 'NONE', *, *, #482, .T. ) ;
#20039 = CARTESIAN_POINT ( 'NONE',  ( 5.624045005368206063, 19.21181948662073324, 18.39701043959520987 ) ) ;
#20040 = EDGE_CURVE ( 'NONE', #23603, #26525, #8373, .T. ) ;
#20041 = LINE ( 'NONE', #10847, #11842 ) ;
#20042 = CARTESIAN_POINT ( 'NONE',  ( -32.41727157990033703, -18.89317060219217126, 37.49999999997574918 ) ) ;
#20043 = ORIENTED_EDGE ( 'NONE', *, *, #16434, .T. ) ;
#20044 = PLANE ( 'NONE',  #4905 ) ;
#20045 = ADVANCED_FACE ( 'NONE', ( #11575 ), #30591, .F. ) ;
#20046 = DIRECTION ( 'NONE',  ( 0.000000000000000000, 1.000000000000000000, 0.000000000000000000 ) ) ;
#20047 = FACE_BOUND ( 'NONE', #667, .T. ) ;
#20048 = DIRECTION ( 'NONE',  ( 0.000000000000000000, -0.000000000000000000, -1.000000000000000000 ) ) ;
#20049 = ORIENTED_EDGE ( 'NONE', *, *, #6301, .F. ) ;
#20050 = CARTESIAN_POINT ( 'NONE',  ( 1.687027447297431371, 8.840471615930075799, 21.50000000000000000 ) ) ;
#20051 = VECTOR ( 'NONE', #20709, 1000.000000000000000 ) ;
#20052 = TOROIDAL_SURFACE ( 'NONE', #8622, 7.000000000000000000, 3.000000000000000000 ) ;
#20053 = CARTESIAN_POINT ( 'NONE',  ( 29.81956388892670873, 15.48018185647901923, 37.15911814917521383 ) ) ;
#20054 = CIRCLE ( 'NONE', #24021, 9.000000000000000000 ) ;
#20055 = DIRECTION ( 'NONE',  ( -0.000000000000000000, -0.000000000000000000, 1.000000000000000000 ) ) ;
#20056 = CARTESIAN_POINT ( 'NONE',  ( -0.7083562926194498788, 9.056472324687613096, 13.22130136205108997 ) ) ;
#20057 = SHAPE_REPRESENTATION ( 'Housing End Cover Cap', ( #7396 ), #9395 ) ;
#20058 = CARTESIAN_POINT ( 'NONE',  ( -21.71568325578193637, 0.000000000000000000, -1.500000000000000000 ) ) ;
#20059 = FACE_OUTER_BOUND ( 'NONE', #8627, .T. ) ;
#20060 = ORIENTED_EDGE ( 'NONE', *, *, #30578, .T. ) ;
#20061 = ADVANCED_FACE ( 'NONE', ( #27655 ), #4399, .F. ) ;
#20062 = EDGE_CURVE ( 'NONE', #29776, #3576, #21305, .T. ) ;
#20063 = ADVANCED_FACE ( 'NONE', ( #13630 ), #23260, .F. ) ;
#20064 = CARTESIAN_POINT ( 'NONE',  ( -5.131244434206278626, -6.812559277181949646, 21.50000000000000000 ) ) ;
#20065 = CARTESIAN_POINT ( 'NONE',  ( 4.308942857043136954, 19.53031007734546165, 6.788986777570708675 ) ) ;
#20066 = EDGE_LOOP ( 'NONE', ( #20353, #3830, #3790, #9903 ) ) ;
#20067 = EDGE_CURVE ( 'NONE', #20761, #12360, #15841, .T. ) ;
#20068 = VERTEX_POINT ( 'NONE', #10977 ) ;
#20069 = FACE_BOUND ( 'NONE', #3964, .T. ) ;
#20070 = CARTESIAN_POINT ( 'NONE',  ( 10.64374042650142904, 42.96126232887663576, -19.50000000000000355 ) ) ;
#20071 = CARTESIAN_POINT ( 'NONE',  ( -3.915634928944694781, 49.85588857687934450, -69.51358094991340408 ) ) ;
#20072 = EDGE_CURVE ( 'NONE', #14363, #16328, #27778, .T. ) ;
#20073 = DIRECTION ( 'NONE',  ( -1.000000000000000000, 0.000000000000000000, 0.000000000000000000 ) ) ;
#20074 = DIRECTION ( 'NONE',  ( -1.000000000000000000, 0.000000000000000000, 0.000000000000000000 ) ) ;
#20075 = EDGE_CURVE ( 'NONE', #28626, #4819, #8943, .T. ) ;
#20076 = VECTOR ( 'NONE', #7006, 1000.000000000000000 ) ;
#20077 = EDGE_CURVE ( 'NONE', #19924, #9077, #904, .T. ) ;
#20078 = ORIENTED_EDGE ( 'NONE', *, *, #15070, .F. ) ;
#20079 = VERTEX_POINT ( 'NONE', #1616 ) ;
#20080 = VECTOR ( 'NONE', #11587, 1000.000000000000000 ) ;
#20081 = CYLINDRICAL_SURFACE ( 'NONE', #26250, 0.7500000000000006661 ) ;
#20082 = CARTESIAN_POINT ( 'NONE',  ( 7.392982946727082449, -5.278755796068694828, 21.50000000000000000 ) ) ;
#20083 = CARTESIAN_POINT ( 'NONE',  ( 40.05520497557499482, 7.028746409576331011, -16.50000000000000000 ) ) ;
#20084 = ORIENTED_EDGE ( 'NONE', *, *, #5186, .F. ) ;
#20085 = CARTESIAN_POINT ( 'NONE',  ( 0.000000000000000000, 0.000000000000000000, 1.500000000000000000 ) ) ;
#20087 = ORIENTED_EDGE ( 'NONE', *, *, #23639, .F. ) ;
#20086 = CIRCLE ( 'NONE', #28052, 32.32717498572574755 ) ;
#20088 = CYLINDRICAL_SURFACE ( 'NONE', #387, 9.482273699623480212 ) ;
#20089 = VERTEX_POINT ( 'NONE', #11125 ) ;
#20090 = EDGE_CURVE ( 'NONE', #321, #25215, #6736, .T. ) ;
#20091 = CIRCLE ( 'NONE', #26580, 19.49999999999996447 ) ;
#20092 = DIRECTION ( 'NONE',  ( -0.2972711322815274060, 0.9547931052914335748, 0.000000000000000000 ) ) ;
#20093 = B_SPLINE_SURFACE_WITH_KNOTS ( 'NONE', 3, 1, ( 
 ( #14435, #26124 ),
 ( #16927, #9745 ),
 ( #24400, #19259 ),
 ( #3044, #5230 ),
 ( #12245, #14588 ),
 ( #12564, #2739 ),
 ( #538, #24090 ),
 ( #21444, #2429 ),
 ( #29089, #7574 ),
 ( #22057, #2893 ),
 ( #692, #10060 ),
 ( #28629, #4755 ),
 ( #4917, #28782 ),
 ( #26446, #17077 ),
 ( #24241, #19572 ),
 ( #3196, #13027 ),
 ( #22215, #22515 ),
 ( #1164, #12718 ),
 ( #25021, #13174 ),
 ( #6149, #19888 ),
 ( #20032, #29553 ),
 ( #17863, #10673 ),
 ( #851, #24877 ),
 ( #29875, #8041 ),
 ( #10837, #8187 ),
 ( #3513, #27380 ),
 ( #5847, #17693 ),
 ( #15655, #1014 ),
 ( #29242, #10210 ),
 ( #5687, #15504 ),
 ( #27210, #18017 ) ),
 .UNSPECIFIED., .F., .F., .F.,
 ( 4, 3, 3, 3, 3, 3, 3, 3, 3, 3, 4 ),
 ( 2, 2 ),
 ( 0.000000000000000000, 0.05425176834609633791, 0.1085332949128352958, 0.1623767749169382768, 0.2157504826133063158, 0.2688657508888171455, 0.3218907763505476360, 0.3749548578363336993, 0.4282048033836242107, 0.4818374082110501444, 0.4999999999131655715 ),
 ( 0.000000000000000000, 1.000000000000000000 ),
 .UNSPECIFIED. ) ;
#20094 = CARTESIAN_POINT ( 'NONE',  ( 19.76051936388920893, 3.198927888044585721, 5.652196082364320695 ) ) ;
#20095 = CARTESIAN_POINT ( 'NONE',  ( -15.21204208253569057, 13.01227270423824400, 18.36582235739946611 ) ) ;
#20096 = ADVANCED_FACE ( 'NONE', ( #27818 ), #8772, .F. ) ;
#20097 = CIRCLE ( 'NONE', #14113, 0.7499999999999997780 ) ;
#20098 = CARTESIAN_POINT ( 'NONE',  ( -7.759781818727209846, -15.20954222608248863, 19.79423548914561692 ) ) ;
#20099 = CARTESIAN_POINT ( 'NONE',  ( -1.297549323414336042, 42.50000000000001421, 28.83974596215564290 ) ) ;
#20100 = VECTOR ( 'NONE', #9668, 1000.000000000000000 ) ;
#20101 = CARTESIAN_POINT ( 'NONE',  ( -9.372686588603338365, -14.20906563287599056, 6.385774490351135313 ) ) ;
#20102 = CARTESIAN_POINT ( 'NONE',  ( -4.163336342344337027E-14, 1.387778780781445676E-14, 1.500000000000000000 ) ) ;
#20103 = ORIENTED_EDGE ( 'NONE', *, *, #27340, .T. ) ;
#20104 = TOROIDAL_SURFACE ( 'NONE', #3680, 37.99999999999933920, 3.000000000000000000 ) ;
#20105 = DIRECTION ( 'NONE',  ( 0.000000000000000000, 1.000000000000000000, 0.000000000000000000 ) ) ;
#20106 = CARTESIAN_POINT ( 'NONE',  ( -28.45592497607851712, 29.06316056193650965, 15.12214346831152767 ) ) ;
#20107 = DIRECTION ( 'NONE',  ( -1.000000000000000000, 0.000000000000000000, 0.000000000000000000 ) ) ;
#20108 = VERTEX_POINT ( 'NONE', #16551 ) ;
#20109 = VERTEX_POINT ( 'NONE', #24176 ) ;
#20110 = CARTESIAN_POINT ( 'NONE',  ( 17.92140030663550831, -8.878400182913011918, 19.60917204426169036 ) ) ;
#20111 = CARTESIAN_POINT ( 'NONE',  ( 28.34828976096171971, -29.18752572968383419, 1.500000000000000000 ) ) ;
#20112 = CARTESIAN_POINT ( 'NONE',  ( -5.292761969338719119, 19.30549167878804084, 5.940635272151477686 ) ) ;
#20113 = VERTEX_POINT ( 'NONE', #28568 ) ;
#20114 = CARTESIAN_POINT ( 'NONE',  ( -1.000000000000008438, 13.00000000000001421, 1.500000000000001332 ) ) ;
#20115 = CYLINDRICAL_SURFACE ( 'NONE', #17150, 0.7499999999999997780 ) ;
#20116 = CARTESIAN_POINT ( 'NONE',  ( 6.067212148875111843, 19.05774739413747909, 6.033082186765050814 ) ) ;
#20117 = ORIENTED_EDGE ( 'NONE', *, *, #19459, .T. ) ;
#20118 = CARTESIAN_POINT ( 'NONE',  ( -10.51100883930070040, -17.01524884273342764, 18.34798005863226678 ) ) ;
#20119 = LINE ( 'NONE', #22602, #16210 ) ;
#20120 = CARTESIAN_POINT ( 'NONE',  ( 16.80963242778063815, 2.754998275627142945, 7.557577766377196582 ) ) ;
#20121 = ORIENTED_EDGE ( 'NONE', *, *, #30168, .F. ) ;
#20122 = CARTESIAN_POINT ( 'NONE',  ( 12.38084545251366997, 11.71426794001388494, 5.651989602109218858 ) ) ;
#20123 = AXIS2_PLACEMENT_3D ( 'NONE', #46, #14221, #27835 ) ;
#20124 = VERTEX_POINT ( 'NONE', #9850 ) ;
#20125 = CARTESIAN_POINT ( 'NONE',  ( -3.469446951953614189E-15, -30.50000000000000711, 24.50000000000000000 ) ) ;
#20126 = CIRCLE ( 'NONE', #8111, 1.447898107987198646 ) ;
#20127 = CARTESIAN_POINT ( 'NONE',  ( 0.000000000000000000, 0.000000000000000000, -1.500000000000000000 ) ) ;
#20128 = ORIENTED_EDGE ( 'NONE', *, *, #12996, .T. ) ;
#20129 = EDGE_LOOP ( 'NONE', ( #2373, #7205 ) ) ;
#20130 = CARTESIAN_POINT ( 'NONE',  ( 5.303644920943712648, 19.30240823413181062, 7.652108011868850035 ) ) ;
#20131 = EDGE_CURVE ( 'NONE', #5698, #3354, #855, .T. ) ;
#20132 = CARTESIAN_POINT ( 'NONE',  ( 33.51212652704789008, 9.877957833750135919, 40.06253926477352678 ) ) ;
#20133 = CARTESIAN_POINT ( 'NONE',  ( -39.87350638641265732, -4.706224724266450998, -6.500000000000000888 ) ) ;
#20134 = CARTESIAN_POINT ( 'NONE',  ( -5.524309650260714299, 7.706848733601010082, 1.500000000000001332 ) ) ;
#20135 = FACE_OUTER_BOUND ( 'NONE', #6060, .T. ) ;
#20136 = DIRECTION ( 'NONE',  ( -0.000000000000000000, -0.000000000000000000, 1.000000000000000000 ) ) ;
#20137 = EDGE_LOOP ( 'NONE', ( #6765, #23334, #20159, #23052 ) ) ;
#20138 = DIRECTION ( 'NONE',  ( 0.000000000000000000, 0.000000000000000000, 1.000000000000000000 ) ) ;
#20139 = CARTESIAN_POINT ( 'NONE',  ( -15.45532977000708641, 12.72198496171736259, 18.35718225375110180 ) ) ;
#20140 = CARTESIAN_POINT ( 'NONE',  ( 9.860909914091287476, -13.90333503830274609, 7.652108011868850923 ) ) ;
#20141 = FACE_OUTER_BOUND ( 'NONE', #16379, .T. ) ;
#20142 = EDGE_LOOP ( 'NONE', ( #7067, #10612, #7115, #24640 ) ) ;
#20143 = CIRCLE ( 'NONE', #14161, 6.000000000000005329 ) ;
#20144 = CARTESIAN_POINT ( 'NONE',  ( 27.98775450039519086, -29.59783709014061515, 12.77861256115351196 ) ) ;
#20145 = FACE_OUTER_BOUND ( 'NONE', #9946, .T. ) ;
#20146 = CARTESIAN_POINT ( 'NONE',  ( -14.76380438154529173, 13.49194818783279004, 18.84056766331481825 ) ) ;
#20147 = SURFACE_STYLE_FILL_AREA ( #29044 ) ;
#20148 = DIRECTION ( 'NONE',  ( -0.000000000000000000, -0.000000000000000000, 1.000000000000000000 ) ) ;
#20149 = CARTESIAN_POINT ( 'NONE',  ( -26.83043119477639493, -8.695877139419037505, 1.500000000000000000 ) ) ;
#20150 = CARTESIAN_POINT ( 'NONE',  ( 17.19472854822046060, 38.15486337162199248, 34.52907637737875746 ) ) ;
#20151 = VERTEX_POINT ( 'NONE', #2363 ) ;
#20152 = CARTESIAN_POINT ( 'NONE',  ( 24.03057240117691862, 26.57182937991349903, 26.54355021145563143 ) ) ;
#20153 = CARTESIAN_POINT ( 'NONE',  ( 0.000000000000000000, 0.000000000000000000, -87.50000000000000000 ) ) ;
#20154 = LINE ( 'NONE', #22182, #11973 ) ;
#20155 = EDGE_LOOP ( 'NONE', ( #11927, #12013, #24527, #705, #28221, #2330 ) ) ;
#20156 = EDGE_LOOP ( 'NONE', ( #21425, #15556, #30431, #11949 ) ) ;
#20157 = CARTESIAN_POINT ( 'NONE',  ( 5.130938270761610021, -7.974144905643801629, 13.00000000000000178 ) ) ;
#20158 = DIRECTION ( 'NONE',  ( 0.000000000000000000, 0.000000000000000000, -1.000000000000000000 ) ) ;
#20159 = ORIENTED_EDGE ( 'NONE', *, *, #17163, .F. ) ;
#20160 = CARTESIAN_POINT ( 'NONE',  ( 32.28307784207223108, 8.475829241206289666, -16.55003854064094426 ) ) ;
#20161 = AXIS2_PLACEMENT_3D ( 'NONE', #28297, #6921, #2229 ) ;
#20162 = CARTESIAN_POINT ( 'NONE',  ( 14.90335466576768120, 47.72767136615566130, -53.03506201841181422 ) ) ;
#20163 = CARTESIAN_POINT ( 'NONE',  ( -36.61964531808753520, 14.63326766589592154, 9.551232946053056949 ) ) ;
#20164 = DIRECTION ( 'NONE',  ( 1.000000000000000000, 0.000000000000000000, 0.000000000000000000 ) ) ;
#20165 = CARTESIAN_POINT ( 'NONE',  ( -11.03465445395215028, -16.68068344163646799, 5.849008070840543638 ) ) ;
#20166 = CARTESIAN_POINT ( 'NONE',  ( 3.662523238938590442, -12.47340865698848056, 24.50000000000000000 ) ) ;
#20167 = CARTESIAN_POINT ( 'NONE',  ( 0.7836603910024315667, -17.02734626465442602, 5.652196082364321583 ) ) ;
#20168 = CYLINDRICAL_SURFACE ( 'NONE', #14617, 1.999999999999998224 ) ;
#20169 = VERTEX_POINT ( 'NONE', #5167 ) ;
#20170 = CARTESIAN_POINT ( 'NONE',  ( -14.97070905019798737, -8.177877011708877930, 7.559636331181775581 ) ) ;
#20171 = DIRECTION ( 'NONE',  ( 0.000000000000000000, -1.000000000000000000, 0.000000000000000000 ) ) ;
#20172 = CARTESIAN_POINT ( 'NONE',  ( 11.47892014274828298, -16.39977715623751564, 7.559636331181775581 ) ) ;
#20173 = CARTESIAN_POINT ( 'NONE',  ( -32.74775157610409337, 27.21557300919391054, -19.50000000000000355 ) ) ;
#20174 = CARTESIAN_POINT ( 'NONE',  ( -19.54426622602688113, 37.07991288358297055, 1.499999999999999778 ) ) ;
#20175 = ORIENTED_EDGE ( 'NONE', *, *, #7084, .F. ) ;
#20176 = EDGE_LOOP ( 'NONE', ( #26492, #1582, #18105, #8932 ) ) ;
#20177 = CARTESIAN_POINT ( 'NONE',  ( -31.22647667302023677, 15.32805873036034328, 35.97188228574919577 ) ) ;
#20178 = AXIS2_PLACEMENT_3D ( 'NONE', #20153, #25302, #22342 ) ;
#20179 = DIRECTION ( 'NONE',  ( -0.000000000000000000, -0.000000000000000000, 1.000000000000000000 ) ) ;
#20180 = CARTESIAN_POINT ( 'NONE',  ( -11.40980092660686829, 6.310027164379044429, 24.50000000000000000 ) ) ;
#20181 = ORIENTED_EDGE ( 'NONE', *, *, #27680, .F. ) ;
#20182 = CARTESIAN_POINT ( 'NONE',  ( -70.00000000000000000, 70.00000000000000000, -92.50000000000000000 ) ) ;
#20183 = CARTESIAN_POINT ( 'NONE',  ( -32.74775157610409337, 27.21557300919391054, -19.50000000000000355 ) ) ;
#20184 = CARTESIAN_POINT ( 'NONE',  ( -11.35443157991640994, -16.48616348260577524, 6.420335371522007506 ) ) ;
#20185 = ORIENTED_EDGE ( 'NONE', *, *, #1425, .T. ) ;
#20186 = CARTESIAN_POINT ( 'NONE',  ( 0.000000000000000000, 10.00000000000000888, 117.5000000000000000 ) ) ;
#20187 = CARTESIAN_POINT ( 'NONE',  ( -12.57346322279386364, -40.23757549468835037, 29.03955556716994124 ) ) ;
#20188 = EDGE_CURVE ( 'NONE', #23298, #21957, #11305, .T. ) ;
#20189 = ORIENTED_EDGE ( 'NONE', *, *, #6550, .F. ) ;
#20190 = CARTESIAN_POINT ( 'NONE',  ( -7.730328572437709767, 4.608906612435681005, -1.500000000000001332 ) ) ;
#20191 = PRODUCT_RELATED_PRODUCT_CATEGORY ( 'part', '', ( #22131 ) ) ;
#20192 = DIRECTION ( 'NONE',  ( 0.8910248307962438385, 0.4539545692076743522, 0.000000000000000000 ) ) ;
#20193 = DIRECTION ( 'NONE',  ( -0.000000000000000000, 0.5000000000000005551, 0.8660254037844382635 ) ) ;
#20194 = EDGE_CURVE ( 'NONE', #2008, #21638, #19193, .T. ) ;
#20195 = ORIENTED_EDGE ( 'NONE', *, *, #27534, .F. ) ;
#20196 = LINE ( 'NONE', #17883, #8329 ) ;
#20197 = VECTOR ( 'NONE', #7530, 1000.000000000000000 ) ;
#20198 = CARTESIAN_POINT ( 'NONE',  ( -8.419710366748644148, 7.777014463793872956, -1.500000000000000000 ) ) ;
#20199 = CARTESIAN_POINT ( 'NONE',  ( 0.000000000000000000, 4.336808689942017736E-15, -17.99999999999998224 ) ) ;
#20200 = EDGE_CURVE ( 'NONE', #20533, #30406, #19770, .T. ) ;
#20201 = DIRECTION ( 'NONE',  ( 0.000000000000000000, 0.000000000000000000, 1.000000000000000000 ) ) ;
#20202 = CIRCLE ( 'NONE', #17224, 0.7500000000000006661 ) ;
#20203 = CARTESIAN_POINT ( 'NONE',  ( -40.53864323030092720, 2.051443709366309154, -16.50000000000000355 ) ) ;
#20204 = LINE ( 'NONE', #22545, #4357 ) ;
#20205 = LINE ( 'NONE', #23002, #27492 ) ;
#20206 = CARTESIAN_POINT ( 'NONE',  ( 0.000000000000000000, -1.324687536737320328E-14, 29.43090101791767665 ) ) ;
#20207 = ORIENTED_EDGE ( 'NONE', *, *, #23274, .F. ) ;
#20208 = CARTESIAN_POINT ( 'NONE',  ( 35.13802340819238168, -8.772855875097450351, 34.58409965093443361 ) ) ;
#20209 = CARTESIAN_POINT ( 'NONE',  ( -8.770223337697045096, -14.60814232176939953, 18.37259980046033903 ) ) ;
#20210 = EDGE_CURVE ( 'NONE', #15949, #18536, #30368, .T. ) ;
#20211 = CIRCLE ( 'NONE', #2807, 0.7500000000000006661 ) ;
#20212 = ORIENTED_EDGE ( 'NONE', *, *, #17222, .F. ) ;
#20213 = ORIENTED_EDGE ( 'NONE', *, *, #10902, .F. ) ;
#20214 = ADVANCED_FACE ( 'NONE', ( #14055 ), #9537, .T. ) ;
#20215 = CARTESIAN_POINT ( 'NONE',  ( -1.246245039005721811, -2.728895986063572643, 24.50000000000000000 ) ) ;
#20216 = FACE_OUTER_BOUND ( 'NONE', #1529, .T. ) ;
#20217 = CARTESIAN_POINT ( 'NONE',  ( -32.50000000000000000, 0.000000000000000000, -87.50000000000000000 ) ) ;
#20218 = VERTEX_POINT ( 'NONE', #21852 ) ;
#20219 = SHAPE_REPRESENTATION_RELATIONSHIP ( 'NONE' , 'NONE' ,  #20057, #9148 ) ;
#20220 = CARTESIAN_POINT ( 'NONE',  ( -4.622016212553093695, -12.19167610014704906, 1.500000000000001332 ) ) ;
#20221 = B_SPLINE_CURVE_WITH_KNOTS ( 'NONE', 3,
 ( #22617, #5785, #13442, #3600, #27466, #6089, #20724, #25272, #22770, #1266, #30105, #8597, #18104, #10620, #11082, #1576, #20580, #12969 ),
 .UNSPECIFIED., .F., .F.,
 ( 4, 2, 2, 2, 2, 2, 2, 2, 4 ),
 ( 0.003174295595554306113, 0.003570702171545539743, 0.003967108747536773374, 0.004363515323528007438, 0.004759921899519240635, 0.005156328475510474699, 0.005552735051501708763, 0.005949141627492942827, 0.006345548203484176024 ),
 .UNSPECIFIED. ) ;
#20222 = CARTESIAN_POINT ( 'NONE',  ( 9.007989464659727830, -14.44232047555457932, 19.21496526180055042 ) ) ;
#20223 = CIRCLE ( 'NONE', #27717, 0.7500000000000006661 ) ;
#20224 = ORIENTED_EDGE ( 'NONE', *, *, #30007, .T. ) ;
#20225 = DIRECTION ( 'NONE',  ( 1.000000000000000000, 0.000000000000000000, 0.000000000000000000 ) ) ;
#20226 = LINE ( 'NONE', #17735, #811 ) ;
#20227 = VECTOR ( 'NONE', #25105, 1000.000000000000000 ) ;
#20228 = CARTESIAN_POINT ( 'NONE',  ( 16.74328841314637017, 3.194145055459935545, 7.652108011868850923 ) ) ;
#20229 = DIRECTION ( 'NONE',  ( 0.000000000000000000, 1.000000000000000000, 0.000000000000000000 ) ) ;
#20230 = EDGE_LOOP ( 'NONE', ( #30587, #204 ) ) ;
#20231 = CARTESIAN_POINT ( 'NONE',  ( -9.185733585337896301, 2.352830851074203533, 13.00000000000000178 ) ) ;
#20232 = EDGE_CURVE ( 'NONE', #20433, #1352, #21754, .T. ) ;
#20233 = ORIENTED_EDGE ( 'NONE', *, *, #22241, .T. ) ;
#20234 = ADVANCED_FACE ( 'NONE', ( #2828 ), #23881, .T. ) ;
#20235 = DIRECTION ( 'NONE',  ( -0.000000000000000000, -0.000000000000000000, 1.000000000000000000 ) ) ;
#20236 = AXIS2_PLACEMENT_3D ( 'NONE', #6981, #9476, #9313 ) ;
#20237 = ORIENTED_EDGE ( 'NONE', *, *, #10926, .T. ) ;
#20238 = PRESENTATION_LAYER_ASSIGNMENT (  '', '', ( #26725 ) ) ;
#20239 = CARTESIAN_POINT ( 'NONE',  ( -6.737892368765498574, 18.83108299337146718, 19.96797677718664232 ) ) ;
#20240 = EDGE_CURVE ( 'NONE', #5019, #5438, #14751, .T. ) ;
#20241 = CARTESIAN_POINT ( 'NONE',  ( 30.60812557944273848, -26.34642019089854870, 30.43068197896959504 ) ) ;
#20242 = CARTESIAN_POINT ( 'NONE',  ( 19.57381806301095750, 4.191719245021451101, 6.782048567692550378 ) ) ;
#20243 = LINE ( 'NONE', #22429, #23086 ) ;
#20244 = FACE_OUTER_BOUND ( 'NONE', #16650, .T. ) ;
#20245 = ADVANCED_FACE ( 'NONE', ( #28263 ), #23560, .T. ) ;
#20246 = CIRCLE ( 'NONE', #17266, 5.000000000000004441 ) ;
#20247 = CYLINDRICAL_SURFACE ( 'NONE', #24481, 15.00000000000003375 ) ;
#20248 = CARTESIAN_POINT ( 'NONE',  ( -19.93127403599639536, 1.860458748833900833, 18.56793045041961321 ) ) ;
#20249 = DIRECTION ( 'NONE',  ( 0.000000000000000000, 1.000000000000000000, 0.000000000000000000 ) ) ;
#20250 = ORIENTED_EDGE ( 'NONE', *, *, #8613, .T. ) ;
#20251 = EDGE_CURVE ( 'NONE', #12146, #16132, #28732, .T. ) ;
#20253 = CARTESIAN_POINT ( 'NONE',  ( 3.262081159835028110, 16.75658363658047278, 18.73314399819312115 ) ) ;
#20252 = AXIS2_PLACEMENT_3D ( 'NONE', #6631, #27550, #22854 ) ;
#20254 = CARTESIAN_POINT ( 'NONE',  ( -32.98805937973593672, 22.67054169308932643, 18.00000000000000000 ) ) ;
#20255 = CIRCLE ( 'NONE', #5811, 9.084132297865673777 ) ;
#20256 = CARTESIAN_POINT ( 'NONE',  ( 27.03943647958860552, 26.20092231554394857, 34.80090346875808649 ) ) ;
#20257 = VERTEX_POINT ( 'NONE', #10008 ) ;
#20258 = ORIENTED_EDGE ( 'NONE', *, *, #19905, .T. ) ;
#20259 = EDGE_CURVE ( 'NONE', #17044, #3185, #25540, .T. ) ;
#20260 = DIRECTION ( 'NONE',  ( 1.000000000000000000, 0.000000000000000000, -0.000000000000000000 ) ) ;
#20261 = CARTESIAN_POINT ( 'NONE',  ( 1.112485354161228957E-15, -9.084132297865677330, 27.94260272410217638 ) ) ;
#20262 = CARTESIAN_POINT ( 'NONE',  ( -4.661329110590012981, 16.37253524622245138, 7.080843742048788414 ) ) ;
#20263 = ORIENTED_EDGE ( 'NONE', *, *, #24631, .F. ) ;
#20264 = DIRECTION ( 'NONE',  ( -0.000000000000000000, -0.000000000000000000, 1.000000000000000000 ) ) ;
#20265 = AXIS2_PLACEMENT_3D ( 'NONE', #17178, #5022, #12359 ) ;
#20266 = CARTESIAN_POINT ( 'NONE',  ( -12.71197447203570263, 11.31946111510421105, 6.519181285484529909 ) ) ;
#20267 = VECTOR ( 'NONE', #26307, 1000.000000000000000 ) ;
#20268 = CARTESIAN_POINT ( 'NONE',  ( -6.812559277181930106, 5.881244434206302607, 21.50000000000000000 ) ) ;
#20269 = VERTEX_POINT ( 'NONE', #12814 ) ;
#20270 = DIRECTION ( 'NONE',  ( 1.000000000000000000, 0.000000000000000000, 0.000000000000000000 ) ) ;
#20271 = CARTESIAN_POINT ( 'NONE',  ( -25.48568755041063838, -12.36160011285428517, 1.500000000000000000 ) ) ;
#20272 = CARTESIAN_POINT ( 'NONE',  ( 19.81199842303381686, 2.865066961627992903, 5.701226463332907279 ) ) ;
#20273 = VERTEX_POINT ( 'NONE', #26860 ) ;
#20274 = AXIS2_PLACEMENT_3D ( 'NONE', #3531, #5554, #22537 ) ;
#20275 = CARTESIAN_POINT ( 'NONE',  ( 15.25015041412930827, 12.96756205105604920, 5.796888747622817029 ) ) ;
#20276 = ADVANCED_FACE ( 'NONE', ( #19980 ), #15283, .F. ) ;
#20277 = VERTEX_POINT ( 'NONE', #637 ) ;
#20278 = CARTESIAN_POINT ( 'NONE',  ( 8.606594496258196614, 4.390207617113981442, 1.500000000000001332 ) ) ;
#20279 = EDGE_CURVE ( 'NONE', #27751, #13589, #14284, .T. ) ;
#20280 = CIRCLE ( 'NONE', #6820, 9.084132297865673777 ) ;
#20281 = CARTESIAN_POINT ( 'NONE',  ( 31.57687401261850724, -15.10620312102102680, 35.75338942089695848 ) ) ;
#20282 = AXIS2_PLACEMENT_3D ( 'NONE', #1238, #9279, #28322 ) ;
#20283 = ORIENTED_EDGE ( 'NONE', *, *, #20800, .F. ) ;
#20284 = EDGE_CURVE ( 'NONE', #16393, #6819, #22158, .T. ) ;
#20285 = ORIENTED_EDGE ( 'NONE', *, *, #5216, .T. ) ;
#20286 = CARTESIAN_POINT ( 'NONE',  ( 3.064607854149375754, 16.80099270350295626, 6.782048567692550378 ) ) ;
#20287 = DIRECTION ( 'NONE',  ( -0.000000000000000000, -0.000000000000000000, -1.000000000000000000 ) ) ;
#20288 = CARTESIAN_POINT ( 'NONE',  ( -2.662523238938575343, -12.47340865698848056, 1.500000000000001332 ) ) ;
#20289 = AXIS2_PLACEMENT_3D ( 'NONE', #29824, #7827, #26698 ) ;
#20290 = CARTESIAN_POINT ( 'NONE',  ( -31.18890335284659443, -19.89223002944918051, 27.50000000000000355 ) ) ;
#20291 = CARTESIAN_POINT ( 'NONE',  ( 10.51735345234056673, -17.03234025559531162, 18.63641924841378028 ) ) ;
#20292 = CARTESIAN_POINT ( 'NONE',  ( 19.89739966441223018, 2.193321724558643382, 19.45164628100866722 ) ) ;
#20293 = EDGE_LOOP ( 'NONE', ( #5762, #16161 ) ) ;
#20294 = AXIS2_PLACEMENT_3D ( 'NONE', #10943, #29959, #4202 ) ;
#20295 = DIRECTION ( 'NONE',  ( 0.000000000000000000, -0.000000000000000000, -1.000000000000000000 ) ) ;
#20296 = CARTESIAN_POINT ( 'NONE',  ( 15.48289691231203768, -7.082479268569366049, 6.018569869498933578 ) ) ;
#20297 = CARTESIAN_POINT ( 'NONE',  ( -13.71804704112739870, 10.14464636835443301, 20.19593175699879595 ) ) ;
#20298 = CARTESIAN_POINT ( 'NONE',  ( 39.99999999999998579, 63.74772708486752038, 62.49999999999999289 ) ) ;
#20299 = ORIENTED_EDGE ( 'NONE', *, *, #24422, .T. ) ;
#20300 = ORIENTED_EDGE ( 'NONE', *, *, #13412, .T. ) ;
#20301 = AXIS2_PLACEMENT_3D ( 'NONE', #13045, #22394, #27076 ) ;
#20302 = CARTESIAN_POINT ( 'NONE',  ( 49.99999999999998579, 50.00000000000000000, -92.50000000000000000 ) ) ;
#20303 = CARTESIAN_POINT ( 'NONE',  ( 10.65056555575646158, -13.34799940469215329, 6.329955581934033404 ) ) ;
#20304 = DIRECTION ( 'NONE',  ( 0.000000000000000000, 0.000000000000000000, -1.000000000000000000 ) ) ;
#20305 = CARTESIAN_POINT ( 'NONE',  ( -52.16608720827707657, -51.86186943028246787, 57.49999999999999289 ) ) ;
#20306 = CIRCLE ( 'NONE', #4350, 3.559164065751841743 ) ;
#20307 = CARTESIAN_POINT ( 'NONE',  ( 0.000000000000000000, 0.000000000000000000, 21.50000000000000000 ) ) ;
#20308 = CARTESIAN_POINT ( 'NONE',  ( 9.860909914091285700, -13.90333503830274253, 20.34789198813115263 ) ) ;
#20309 = LINE ( 'NONE', #27342, #6454 ) ;
#20310 = CIRCLE ( 'NONE', #27801, 11.99999999999998934 ) ;
#20311 = EDGE_CURVE ( 'NONE', #4151, #30377, #4311, .T. ) ;
#20312 = ORIENTED_EDGE ( 'NONE', *, *, #20976, .F. ) ;
#20313 = AXIS2_PLACEMENT_3D ( 'NONE', #30749, #11891, #2367 ) ;
#20314 = ADVANCED_FACE ( 'NONE', ( #26024 ), #9645, .T. ) ;
#20315 = CARTESIAN_POINT ( 'NONE',  ( 2.599508007902112006, 14.29059753516471964, 1.500000000000000000 ) ) ;
#20316 = AXIS2_PLACEMENT_3D ( 'NONE', #4140, #3837, #13363 ) ;
#20317 = CYLINDRICAL_SURFACE ( 'NONE', #20178, 12.18947652193948272 ) ;
#20318 = FACE_OUTER_BOUND ( 'NONE', #20737, .T. ) ;
#20319 = VERTEX_POINT ( 'NONE', #11831 ) ;
#20320 = ORIENTED_EDGE ( 'NONE', *, *, #25764, .F. ) ;
#20321 = CARTESIAN_POINT ( 'NONE',  ( -6.778663211761418061, 6.630478080506979843, 21.50000000000000000 ) ) ;
#20322 = CARTESIAN_POINT ( 'NONE',  ( 0.000000000000000000, 0.000000000000000000, 0.000000000000000000 ) ) ;
#20323 = EDGE_LOOP ( 'NONE', ( #1607, #7971, #27165, #4722, #21186, #15908, #18453, #20422, #2006 ) ) ;
#20324 = CARTESIAN_POINT ( 'NONE',  ( 16.58889461517681951, -35.15515261640817357, 27.50000000000000711 ) ) ;
#20325 = AXIS2_PLACEMENT_3D ( 'NONE', #4098, #13764, #15791 ) ;
#20326 = CARTESIAN_POINT ( 'NONE',  ( 14.03875201089029190, 47.98907823057331257, -49.69408436906743987 ) ) ;
#20327 = CARTESIAN_POINT ( 'NONE',  ( -32.98805937973593672, 0.000000000000000000, 8.000000000000003553 ) ) ;
#20328 = CARTESIAN_POINT ( 'NONE',  ( -37.93416654086659889, 9.868537071680707484, 13.74336834489238868 ) ) ;
#20329 = CARTESIAN_POINT ( 'NONE',  ( 32.28307784207223108, -8.475829241206289666, 37.38016955275583086 ) ) ;
#20330 = DIRECTION ( 'NONE',  ( -0.000000000000000000, -0.000000000000000000, 1.000000000000000000 ) ) ;
#20331 = DIRECTION ( 'NONE',  ( 0.000000000000000000, 0.000000000000000000, 1.000000000000000000 ) ) ;
#20332 = CARTESIAN_POINT ( 'NONE',  ( -16.83567995169601161, 2.524450606648186213, 7.156916968540302904 ) ) ;
#20333 = AXIS2_PLACEMENT_3D ( 'NONE', #11864, #28702, #2 ) ;
#20334 = ORIENTED_EDGE ( 'NONE', *, *, #18362, .T. ) ;
#20335 = CARTESIAN_POINT ( 'NONE',  ( 0.000000000000000000, 1.699320956058915452E-16, -1.500000000000001776 ) ) ;
#20336 = CARTESIAN_POINT ( 'NONE',  ( -4.953525029859956241, 16.29343450967639129, 5.848946451764560628 ) ) ;
#20337 = CARTESIAN_POINT ( 'NONE',  ( 10.69412491129097909, -13.31565357151865570, 6.560937769032974209 ) ) ;
#20338 = CARTESIAN_POINT ( 'NONE',  ( -13.22505861668184046, -42.10773672057003125, -19.50000000000000355 ) ) ;
#20339 = CARTESIAN_POINT ( 'NONE',  ( -23.22298176981137274, 35.92225146851140494, -14.83329738373930340 ) ) ;
#20340 = AXIS2_PLACEMENT_3D ( 'NONE', #29886, #8526, #8971 ) ;
#20341 = ORIENTED_EDGE ( 'NONE', *, *, #10148, .T. ) ;
#20342 = ORIENTED_EDGE ( 'NONE', *, *, #16050, .F. ) ;
#20343 = CARTESIAN_POINT ( 'NONE',  ( -7.483314773547907528, 75.00000000000001421, 50.49999999999998579 ) ) ;
#20344 = CARTESIAN_POINT ( 'NONE',  ( -39.00000000000000000, -5.563236990218529243, -1.500000000000000000 ) ) ;
#20345 = CARTESIAN_POINT ( 'NONE',  ( 26.44644203219471379, 9.801837641955973623, -1.500000000000000000 ) ) ;
#20346 = FACE_OUTER_BOUND ( 'NONE', #10510, .T. ) ;
#20347 = EDGE_LOOP ( 'NONE', ( #25136, #17593, #23007, #365 ) ) ;
#20348 = CARTESIAN_POINT ( 'NONE',  ( 3.790840891945185476, 16.62820496708805962, 5.653604225791662330 ) ) ;
#20349 = EDGE_CURVE ( 'NONE', #12825, #15108, #26171, .T. ) ;
#20350 = CARTESIAN_POINT ( 'NONE',  ( 39.83602371821015709, 11.57901747687536265, -19.50000000000000355 ) ) ;
#20351 = CARTESIAN_POINT ( 'NONE',  ( -8.738547258790619665, -14.62818084867463853, 5.670038381137163519 ) ) ;
#20352 = AXIS2_PLACEMENT_3D ( 'NONE', #6499, #13683, #23620 ) ;
#20353 = ORIENTED_EDGE ( 'NONE', *, *, #10703, .F. ) ;
#20354 = B_SPLINE_SURFACE_WITH_KNOTS ( 'NONE', 3, 1, ( 
 ( #1586, #3931 ),
 ( #16077, #6565 ),
 ( #27938, #25737 ),
 ( #13889, #4368 ),
 ( #13452, #30421 ),
 ( #9058, #27629 ),
 ( #18266, #25593 ),
 ( #11096, #8913 ),
 ( #20590, #1881 ),
 ( #27477, #22783 ),
 ( #6704, #4213 ),
 ( #18576, #23076 ),
 ( #30267, #15608 ),
 ( #8746, #13736 ),
 ( #22934, #11404 ),
 ( #1724, #23391 ),
 ( #20451, #30115 ),
 ( #27788, #2028 ),
 ( #20896, #6415 ),
 ( #3769, #15933 ),
 ( #28082, #25447 ),
 ( #16219, #18436 ),
 ( #29970, #11553 ),
 ( #21043, #30565 ),
 ( #17969, #25126 ),
 ( #18114, #4070 ),
 ( #1437, #13288 ),
 ( #10952, #8608 ),
 ( #11239, #6253 ),
 ( #13598, #15764 ),
 ( #25285, #16985 ) ),
 .UNSPECIFIED., .F., .F., .F.,
 ( 4, 3, 3, 3, 3, 3, 3, 3, 3, 3, 4 ),
 ( 2, 2 ),
 ( 0.4999999998345684982, 0.5360336730431939367, 0.5907651151589012883, 0.6456034593241830599, 0.6998270958050434309, 0.7529536536315937223, 0.8052385063053260073, 0.8575343587103997356, 0.9106564858195042023, 0.9648414833209685293, 1.000000006602610236 ),
 ( 0.000000000000000000, 1.000000000000000000 ),
 .UNSPECIFIED. ) ;
#20355 = AXIS2_PLACEMENT_3D ( 'NONE', #22684, #3213, #17884 ) ;
#20356 = VECTOR ( 'NONE', #3885, 1000.000000000000000 ) ;
#20357 = LINE ( 'NONE', #22674, #10851 ) ;
#20358 = AXIS2_PLACEMENT_3D ( 'NONE', #24980, #22793, #3471 ) ;
#20359 = CARTESIAN_POINT ( 'NONE',  ( -8.896251305007044863, -36.43423536520429451, 37.50000000002009415 ) ) ;
#20360 = ORIENTED_EDGE ( 'NONE', *, *, #18398, .T. ) ;
#20361 = CARTESIAN_POINT ( 'NONE',  ( 14.41708049311143469, -17.22181377297010130, 1.500000000000000000 ) ) ;
#20362 = CARTESIAN_POINT ( 'NONE',  ( -10.45807895166738710, -17.06883091098137939, 5.652605728828375753 ) ) ;
#20363 = FACE_BOUND ( 'NONE', #17790, .T. ) ;
#20364 = ORIENTED_EDGE ( 'NONE', *, *, #13503, .F. ) ;
#20365 = CARTESIAN_POINT ( 'NONE',  ( 24.35970437652574105, 13.37404834226503958, 42.96778633356035471 ) ) ;
#20366 = CARTESIAN_POINT ( 'NONE',  ( 12.76513901715592958, 11.27219777357495900, 20.14907003336613300 ) ) ;
#20367 = DIRECTION ( 'NONE',  ( 0.000000000000000000, 0.000000000000000000, -1.000000000000000000 ) ) ;
#20368 = FACE_OUTER_BOUND ( 'NONE', #1611, .T. ) ;
#20369 = DIRECTION ( 'NONE',  ( 1.000000000000000000, 0.000000000000000000, 0.000000000000000000 ) ) ;
#20370 = DIRECTION ( 'NONE',  ( -0.000000000000000000, 0.000000000000000000, 1.000000000000000000 ) ) ;
#20371 = DIRECTION ( 'NONE',  ( 0.9594929736144992560, 0.2817325568414232317, 0.000000000000000000 ) ) ;
#20372 = CARTESIAN_POINT ( 'NONE',  ( -50.00000000000000000, 70.00000000000000000, 12.49999999999999112 ) ) ;
#20373 = DIRECTION ( 'NONE',  ( 0.000000000000000000, -0.000000000000000000, 1.000000000000000000 ) ) ;
#20374 = CARTESIAN_POINT ( 'NONE',  ( 35.97269501643856415, -1.773469557554536502, 34.75180443448059719 ) ) ;
#20375 = CARTESIAN_POINT ( 'NONE',  ( -8.550548372801090480, -14.74545326687210434, 20.34789198813115263 ) ) ;
#20376 = VECTOR ( 'NONE', #11171, 1000.000000000000000 ) ;
#20377 = ORIENTED_EDGE ( 'NONE', *, *, #29964, .T. ) ;
#20378 = VECTOR ( 'NONE', #18325, 1000.000000000000114 ) ;
#20379 = ORIENTED_EDGE ( 'NONE', *, *, #30529, .F. ) ;
#20380 = CARTESIAN_POINT ( 'NONE',  ( 0.000000000000000000, 80.00000000000000000, 50.49999999999998579 ) ) ;
#20381 = CARTESIAN_POINT ( 'NONE',  ( -50.00000000000000000, -50.00000000000000000, 12.49999999999999112 ) ) ;
#20382 = FACE_OUTER_BOUND ( 'NONE', #25907, .T. ) ;
#20383 = ORIENTED_EDGE ( 'NONE', *, *, #26164, .F. ) ;
#20384 =( NAMED_UNIT ( * ) SI_UNIT ( $, .STERADIAN. ) SOLID_ANGLE_UNIT ( ) );
#20385 = VECTOR ( 'NONE', #12644, 1000.000000000000000 ) ;
#20386 = CARTESIAN_POINT ( 'NONE',  ( 8.268028093133366951, 3.763133143576461670, 13.22130136205108819 ) ) ;
#20387 = CARTESIAN_POINT ( 'NONE',  ( 9.752055262432786975, -13.97602916343634583, 20.34789198813115974 ) ) ;
#20388 = ADVANCED_FACE ( 'NONE', ( #28675 ), #3671, .T. ) ;
#20389 = VERTEX_POINT ( 'NONE', #8395 ) ;
#20390 = VERTEX_POINT ( 'NONE', #10418 ) ;
#20391 = EDGE_CURVE ( 'NONE', #13705, #4512, #8230, .T. ) ;
#20392 = CARTESIAN_POINT ( 'NONE',  ( -11.03614041005516277, -16.67970391259860108, 20.14992337338001960 ) ) ;
#20393 = CIRCLE ( 'NONE', #14910, 28.20443790117963800 ) ;
#20394 = CARTESIAN_POINT ( 'NONE',  ( -2.081668171172168513E-14, 90.00000000000001421, 52.49999999999999289 ) ) ;
#20395 = CARTESIAN_POINT ( 'NONE',  ( 15.53710936759972050, 12.59357901975564076, 6.518927109361845496 ) ) ;
#20396 = DIRECTION ( 'NONE',  ( -0.1423148382732850048, -0.9898214418809327952, 0.000000000000000000 ) ) ;
#20397 = ORIENTED_EDGE ( 'NONE', *, *, #7062, .T. ) ;
#20398 = CARTESIAN_POINT ( 'NONE',  ( -4.604861147461548398, 16.38721654675212847, 19.60617949693493500 ) ) ;
#20399 = VERTEX_POINT ( 'NONE', #15078 ) ;
#20400 = CARTESIAN_POINT ( 'NONE',  ( -15.16517293421789070, -7.781889191988407894, 7.652108011868850923 ) ) ;
#20401 = DIRECTION ( 'NONE',  ( 0.000000000000000000, -1.132880637372608986E-16, 1.000000000000000000 ) ) ;
#20402 = ORIENTED_EDGE ( 'NONE', *, *, #13579, .F. ) ;
#20403 = DIRECTION ( 'NONE',  ( 0.2817325568414296710, -0.9594929736144973687, 0.000000000000000000 ) ) ;
#20404 = CARTESIAN_POINT ( 'NONE',  ( 16.61290147319823518, 3.916522693408249545, 5.951255046771932733 ) ) ;
#20405 = DIRECTION ( 'NONE',  ( -1.000000000000000000, 0.000000000000000000, 0.000000000000000000 ) ) ;
#20406 = CARTESIAN_POINT ( 'NONE',  ( 1.795304038745368480, -16.98367057141060599, 6.783738457429051572 ) ) ;
#20407 = DIRECTION ( 'NONE',  ( -9.830099697201897928E-15, 1.000000000000000000, 0.000000000000000000 ) ) ;
#20408 = FACE_OUTER_BOUND ( 'NONE', #26238, .T. ) ;
#20409 = FACE_BOUND ( 'NONE', #10338, .T. ) ;
#20410 = ORIENTED_EDGE ( 'NONE', *, *, #14898, .F. ) ;
#20411 = VECTOR ( 'NONE', #10058, 1000.000000000000000 ) ;
#20412 = CARTESIAN_POINT ( 'NONE',  ( 10.68026781623521515, -13.32599531033823759, 19.14333282897057842 ) ) ;
#20413 = ADVANCED_FACE ( 'NONE', ( #19934 ), #730, .T. ) ;
#20414 = CARTESIAN_POINT ( 'NONE',  ( -4.375757216953428294E-15, -39.50000000000000000, 34.80090346875809360 ) ) ;
#20415 = ORIENTED_EDGE ( 'NONE', *, *, #13635, .F. ) ;
#20416 = ORIENTED_EDGE ( 'NONE', *, *, #9780, .T. ) ;
#20417 = CARTESIAN_POINT ( 'NONE',  ( 41.18405171698749001, 67.96430988548668495, 12.55145055161026058 ) ) ;
#20418 = ADVANCED_FACE ( 'NONE', ( #22418 ), #20081, .F. ) ;
#20419 = DIRECTION ( 'NONE',  ( 1.000000000000000000, 0.000000000000000000, 0.000000000000000000 ) ) ;
#20420 = EDGE_CURVE ( 'NONE', #19716, #2236, #1839, .T. ) ;
#20421 = CARTESIAN_POINT ( 'NONE',  ( -5.031059497539948744, 16.27164807758200027, 5.796888747622817029 ) ) ;
#20422 = ORIENTED_EDGE ( 'NONE', *, *, #22275, .T. ) ;
#20423 = DIRECTION ( 'NONE',  ( -1.000000000000000000, 0.000000000000000000, 0.000000000000000000 ) ) ;
#20424 = CARTESIAN_POINT ( 'NONE',  ( -13.20835299067310409, 10.76336294910227664, 7.626437579292365321 ) ) ;
#20425 = CARTESIAN_POINT ( 'NONE',  ( -7.730328572437709767, 4.608906612435681005, 21.50000000000000000 ) ) ;
#20426 = ORIENTED_EDGE ( 'NONE', *, *, #9051, .F. ) ;
#20427 = EDGE_CURVE ( 'NONE', #15471, #16863, #17734, .T. ) ;
#20428 = PLANE ( 'NONE',  #21707 ) ;
#20429 = AXIS2_PLACEMENT_3D ( 'NONE', #5150, #7349, #26207 ) ;
#20430 = CARTESIAN_POINT ( 'NONE',  ( 14.84329864647545172, 13.43104200419766059, 5.652605728828373977 ) ) ;
#20431 = CARTESIAN_POINT ( 'NONE',  ( -33.37783937289808733, -9.491076832576640143, 40.29910134393502119 ) ) ;
#20432 = ORIENTED_EDGE ( 'NONE', *, *, #23131, .T. ) ;
#20433 = VERTEX_POINT ( 'NONE', #3234 ) ;
#20434 = ADVANCED_FACE ( 'NONE', ( #25065 ), #8149, .T. ) ;
#20435 = FACE_OUTER_BOUND ( 'NONE', #2734, .T. ) ;
#20436 = VERTEX_POINT ( 'NONE', #16166 ) ;
#20437 = EDGE_CURVE ( 'NONE', #18506, #160, #24248, .T. ) ;
#20438 = ORIENTED_EDGE ( 'NONE', *, *, #18721, .T. ) ;
#20439 = EDGE_CURVE ( 'NONE', #950, #30524, #20840, .T. ) ;
#20440 = CARTESIAN_POINT ( 'NONE',  ( 4.523123428450326777, 19.49994255397358600, 6.041646659195333058 ) ) ;
#20441 = CARTESIAN_POINT ( 'NONE',  ( 6.812559277181973627, -5.881244434206257310, 21.50000000000000000 ) ) ;
#20442 = CARTESIAN_POINT ( 'NONE',  ( 13.00999358272542850, -0.8602714556717643291, 24.50000000000000000 ) ) ;
#20443 = ORIENTED_EDGE ( 'NONE', *, *, #17671, .T. ) ;
#20444 = CARTESIAN_POINT ( 'NONE',  ( 9.096230214749073895, -14.38931669386024836, 18.90679857307105749 ) ) ;
#20445 = DIRECTION ( 'NONE',  ( 1.000000000000000000, 0.000000000000000000, 0.000000000000000000 ) ) ;
#20446 = VERTEX_POINT ( 'NONE', #8696 ) ;
#20447 = DIRECTION ( 'NONE',  ( -0.000000000000000000, 1.132880637372608986E-16, -1.000000000000000000 ) ) ;
#20448 = CARTESIAN_POINT ( 'NONE',  ( 18.16954353748349860, -8.401983848419027012, 7.557577766377196582 ) ) ;
#20449 = AXIS2_PLACEMENT_3D ( 'NONE', #26966, #27260, #24918 ) ;
#20450 = DIRECTION ( 'NONE',  ( 0.000000000000000000, 1.000000000000000000, 0.000000000000000000 ) ) ;
#20451 = CARTESIAN_POINT ( 'NONE',  ( 4.318335944327693632, 19.54627428603377126, 19.47783254395485031 ) ) ;
#20452 = ORIENTED_EDGE ( 'NONE', *, *, #28416, .F. ) ;
#20453 = EDGE_LOOP ( 'NONE', ( #21994, #26658, #18516, #2944 ) ) ;
#20454 = CARTESIAN_POINT ( 'NONE',  ( 28.79137815760242702, -9.331429872129930914, 1.500000000000000000 ) ) ;
#20455 = EDGE_CURVE ( 'NONE', #18622, #10066, #8428, .T. ) ;
#20456 = CARTESIAN_POINT ( 'NONE',  ( 64.99999999999998579, -36.86186943028246787, 57.49999999999999289 ) ) ;
#20457 = EDGE_CURVE ( 'NONE', #23101, #7851, #25533, .T. ) ;
#20458 = CARTESIAN_POINT ( 'NONE',  ( 12.88533868980070096, 11.12831076047921286, 7.267659094423561505 ) ) ;
#20459 = DIRECTION ( 'NONE',  ( 1.000000000000000000, 0.000000000000000000, 0.000000000000000000 ) ) ;
#20460 = FACE_BOUND ( 'NONE', #18920, .T. ) ;
#20461 = DIRECTION ( 'NONE',  ( 0.000000000000000000, -0.000000000000000000, -1.000000000000000000 ) ) ;
#20462 = ORIENTED_EDGE ( 'NONE', *, *, #3661, .F. ) ;
#20463 = ADVANCED_FACE ( 'NONE', ( #19121 ), #1351, .T. ) ;
#20464 = CARTESIAN_POINT ( 'NONE',  ( 2.959227181723801170, -8.499586724479446076, 21.50000000000000000 ) ) ;
#20465 = CARTESIAN_POINT ( 'NONE',  ( -33.54113041553378594, 10.01041480049199173, 39.99718304311860351 ) ) ;
#20466 = CARTESIAN_POINT ( 'NONE',  ( 28.78283879316666471, 7.125616703334845425, 45.34931131770219537 ) ) ;
#20467 = ORIENTED_EDGE ( 'NONE', *, *, #29469, .T. ) ;
#20468 = ORIENTED_EDGE ( 'NONE', *, *, #10964, .T. ) ;
#20469 = EDGE_CURVE ( 'NONE', #15101, #14162, #7262, .T. ) ;
#20470 = DIRECTION ( 'NONE',  ( -0.000000000000000000, 1.132880637372608986E-16, -1.000000000000000000 ) ) ;
#20471 = CIRCLE ( 'NONE', #13581, 9.084132297865673777 ) ;
#20472 = CARTESIAN_POINT ( 'NONE',  ( 1.438332125858173605, -8.884323311075778662, 21.50000000000000000 ) ) ;
#20473 = ORIENTED_EDGE ( 'NONE', *, *, #12472, .T. ) ;
#20474 = CARTESIAN_POINT ( 'NONE',  ( -9.454746441592954298, 0.7220001660363462026, 13.00000000000000178 ) ) ;
#20475 = CARTESIAN_POINT ( 'NONE',  ( 10.26717756958418981, 48.93576106897143774, -44.05370344458894039 ) ) ;
#20476 = CARTESIAN_POINT ( 'NONE',  ( -8.773161920692750471, -41.42171262360664485, 20.61303894108385037 ) ) ;
#20477 = DIRECTION ( 'NONE',  ( 1.000000000000000000, 0.000000000000000000, 0.000000000000000000 ) ) ;
#20478 = DIRECTION ( 'NONE',  ( -0.000000000000000000, -0.000000000000000000, -1.000000000000000000 ) ) ;
#20479 = DIRECTION ( 'NONE',  ( -0.000000000000000000, -0.000000000000000000, -1.000000000000000000 ) ) ;
#20480 = CARTESIAN_POINT ( 'NONE',  ( 1.694955473231256393, -16.99033591619069483, 7.098451512883313441 ) ) ;
#20481 = CARTESIAN_POINT ( 'NONE',  ( -16.89565484002363149, 2.154541803859437277, 7.526951045817045660 ) ) ;
#20482 = ORIENTED_EDGE ( 'NONE', *, *, #16543, .F. ) ;
#20483 = EDGE_CURVE ( 'NONE', #15490, #28288, #11805, .T. ) ;
#20484 = ADVANCED_FACE ( 'NONE', ( #28488 ), #1175, .T. ) ;
#20485 = DIRECTION ( 'NONE',  ( 0.000000000000000000, 1.132880637372608986E-16, -1.000000000000000000 ) ) ;
#20486 = DIRECTION ( 'NONE',  ( -0.9329908884337537733, -0.3598999890241659783, 0.000000000000000000 ) ) ;
#20487 = CYLINDRICAL_SURFACE ( 'NONE', #10577, 10.00000000000000178 ) ;
#20488 = CARTESIAN_POINT ( 'NONE',  ( 9.454746441592959627, -0.7220001660362782570, 1.500000000000001332 ) ) ;
#20489 = CIRCLE ( 'NONE', #8553, 0.7500000000000024425 ) ;
#20490 = DIRECTION ( 'NONE',  ( 0.000000000000000000, 0.000000000000000000, -1.000000000000000000 ) ) ;
#20491 = VERTEX_POINT ( 'NONE', #1174 ) ;
#20492 = DIRECTION ( 'NONE',  ( -0.000000000000000000, 1.000000000000000000, -0.000000000000000000 ) ) ;
#20493 = CARTESIAN_POINT ( 'NONE',  ( -10.64374042650306862, 42.96126232887723972, -19.50000000000000355 ) ) ;
#20494 = CARTESIAN_POINT ( 'NONE',  ( 11.91580570916392290, -40.47530258207431331, 34.56547942634522030 ) ) ;
#20495 = DIRECTION ( 'NONE',  ( 0.000000000000000000, 0.000000000000000000, -1.000000000000000000 ) ) ;
#20496 = ORIENTED_EDGE ( 'NONE', *, *, #4074, .T. ) ;
#20497 = DIRECTION ( 'NONE',  ( 1.000000000000000000, 0.000000000000000000, 0.000000000000000000 ) ) ;
#20498 = CARTESIAN_POINT ( 'NONE',  ( 37.98493438989863336, -11.12428508576153341, -1.500000000000000000 ) ) ;
#20499 = CARTESIAN_POINT ( 'NONE',  ( -8.744978663125429819, -14.62407600317563627, 7.632642797338977658 ) ) ;
#20500 = ORIENTED_EDGE ( 'NONE', *, *, #39, .T. ) ;
#20501 = AXIS2_PLACEMENT_3D ( 'NONE', #12370, #17038, #2849 ) ;
#20502 = CARTESIAN_POINT ( 'NONE',  ( -14.89473990422384198, 17.79239818699320708, -1.500000000000000000 ) ) ;
#20503 = CARTESIAN_POINT ( 'NONE',  ( 19.74328841314634886, 3.194145055459934213, 20.34789198813115263 ) ) ;
#20504 = EDGE_LOOP ( 'NONE', ( #9176, #18094, #16374 ) ) ;
#20505 = DIRECTION ( 'NONE',  ( 0.000000000000000000, 0.000000000000000000, -1.000000000000000000 ) ) ;
#20506 = CARTESIAN_POINT ( 'NONE',  ( -1.073881485057887497, 0.9711784013062738641, 1.500000000000000000 ) ) ;
#20507 = AXIS2_PLACEMENT_3D ( 'NONE', #29261, #12894, #13043 ) ;
#20508 = LINE ( 'NONE', #30178, #30293 ) ;
#20509 = FACE_BOUND ( 'NONE', #14852, .T. ) ;
#20510 = ORIENTED_EDGE ( 'NONE', *, *, #16059, .T. ) ;
#20511 = CARTESIAN_POINT ( 'NONE',  ( 12.00212711895368933, 12.12705342280389154, 20.24143955528809258 ) ) ;
#20512 = CYLINDRICAL_SURFACE ( 'NONE', #30783, 12.50000000000000000 ) ;
#20513 = CARTESIAN_POINT ( 'NONE',  ( 1.164358918501135598, -19.96629823696781614, 18.73377938172348323 ) ) ;
#20514 = FACE_OUTER_BOUND ( 'NONE', #21663, .T. ) ;
#20515 = CYLINDRICAL_SURFACE ( 'NONE', #12764, 1.000000000000004441 ) ;
#20517 = EDGE_CURVE ( 'NONE', #21638, #1882, #17239, .T. ) ;
#20516 = LINE ( 'NONE', #30038, #14825 ) ;
#20518 = DIRECTION ( 'NONE',  ( 0.000000000000000000, 0.000000000000000000, 1.000000000000000000 ) ) ;
#20519 = FACE_OUTER_BOUND ( 'NONE', #12673, .T. ) ;
#20520 = CARTESIAN_POINT ( 'NONE',  ( -5.393256883115301825, -14.81828060999315433, 1.500000000000001332 ) ) ;
#20521 = CARTESIAN_POINT ( 'NONE',  ( -3.763133143576374628, 8.268028093133407808, 21.50000000000000000 ) ) ;
#20522 = DIRECTION ( 'NONE',  ( 0.000000000000000000, -1.132880637372608986E-16, 1.000000000000000000 ) ) ;
#20523 = VERTEX_POINT ( 'NONE', #1022 ) ;
#20524 = EDGE_LOOP ( 'NONE', ( #20688, #7523, #20708 ) ) ;
#20525 = LINE ( 'NONE', #22701, #14933 ) ;
#20526 = CARTESIAN_POINT ( 'NONE',  ( 2.687479363073301819, 44.39187623479102740, -19.50000000000000355 ) ) ;
#20527 = CARTESIAN_POINT ( 'NONE',  ( -4.163336342344337027E-14, 1.387778780781445676E-14, 1.500000000000000000 ) ) ;
#20528 = ORIENTED_EDGE ( 'NONE', *, *, #8916, .T. ) ;
#20529 =( NAMED_UNIT ( * ) PLANE_ANGLE_UNIT ( ) SI_UNIT ( $, .RADIAN. ) );
#20530 = CIRCLE ( 'NONE', #26962, 0.7441270634457163302 ) ;
#20531 = CYLINDRICAL_SURFACE ( 'NONE', #27360, 7.500000000000000000 ) ;
#20532 = CARTESIAN_POINT ( 'NONE',  ( 9.755266891893601411, -13.97392213636465108, 18.34727598691067740 ) ) ;
#20533 = VERTEX_POINT ( 'NONE', #21916 ) ;
#20534 = ORIENTED_EDGE ( 'NONE', *, *, #26162, .T. ) ;
#20535 = CARTESIAN_POINT ( 'NONE',  ( -10.73477556097085994, -16.87541441043898161, 18.37250658438899009 ) ) ;
#20536 = LINE ( 'NONE', #26097, #28199 ) ;
#20537 = CARTESIAN_POINT ( 'NONE',  ( 5.204170427930421283E-15, -44.07656352898514740, -16.50000000000000000 ) ) ;
#20538 = CARTESIAN_POINT ( 'NONE',  ( -8.884323311075783991, -1.438332125858144295, 21.50000000000000000 ) ) ;
#20539 = ORIENTED_EDGE ( 'NONE', *, *, #27685, .T. ) ;
#20540 = DIRECTION ( 'NONE',  ( -1.000000000000000000, 0.000000000000000000, -1.982541115402065356E-16 ) ) ;
#20541 = AXIS2_PLACEMENT_3D ( 'NONE', #19961, #5621, #8116 ) ;
#20542 = ORIENTED_EDGE ( 'NONE', *, *, #17461, .F. ) ;
#20543 = AXIS2_PLACEMENT_3D ( 'NONE', #23770, #1961, #13819 ) ;
#20544 = LINE ( 'NONE', #13545, #21493 ) ;
#20545 = CARTESIAN_POINT ( 'NONE',  ( -16.81483160676717503, 2.643882879105585726, 19.47784884541372108 ) ) ;
#20546 = ORIENTED_EDGE ( 'NONE', *, *, #6521, .F. ) ;
#20547 = CARTESIAN_POINT ( 'NONE',  ( 33.42925964089141644, -11.06161099612213228, 39.78814634291933316 ) ) ;
#20548 = CARTESIAN_POINT ( 'NONE',  ( 26.47682648895289503, -31.23348282226190165, 29.92111261860823745 ) ) ;
#20549 = CARTESIAN_POINT ( 'NONE',  ( 16.73141127408300477, 3.267558643021993170, 7.652108011868850035 ) ) ;
#20550 = CARTESIAN_POINT ( 'NONE',  ( -10.52692686119061882, -17.02631563033163076, 20.34789198813115263 ) ) ;
#20551 = PLANE ( 'NONE',  #26491 ) ;
#20552 = CARTESIAN_POINT ( 'NONE',  ( -9.288552932799431616, -14.26664216879983371, 6.143977687428008316 ) ) ;
#20553 = LINE ( 'NONE', #25238, #20356 ) ;
#20554 = ORIENTED_EDGE ( 'NONE', *, *, #6330, .F. ) ;
#20555 = CARTESIAN_POINT ( 'NONE',  ( -31.31139399731532080, 25.34153631408518592, 17.71763994997926162 ) ) ;
#20556 = CARTESIAN_POINT ( 'NONE',  ( 15.85884089648733131, 35.55173462727347555, 34.80090346875810070 ) ) ;
#20557 = VERTEX_POINT ( 'NONE', #3355 ) ;
#20558 = EDGE_LOOP ( 'NONE', ( #11448, #29809, #6479, #16008 ) ) ;
#20559 = CARTESIAN_POINT ( 'NONE',  ( 43.30651650232057648, 68.84932239039000024, 13.05702333277023719 ) ) ;
#20560 = AXIS2_PLACEMENT_3D ( 'NONE', #26819, #17451, #5281 ) ;
#20561 = CARTESIAN_POINT ( 'NONE',  ( -15.73693831436012402, 12.34332084443491873, 5.853797745100182581 ) ) ;
#20562 = AXIS2_PLACEMENT_3D ( 'NONE', #27338, #18124, #19995 ) ;
#20563 = B_SPLINE_CURVE_WITH_KNOTS ( 'NONE', 3,
 ( #25077, #8562, #24607, #27582, #10729, #13396, #10428, #3876, #5740, #11045, #29302, #13085, #20239, #29763, #5595, #22574, #8405, #17450 ),
 .UNSPECIFIED., .F., .F.,
 ( 4, 2, 2, 2, 2, 2, 2, 2, 4 ),
 ( 0.000000000000000000, 0.0003967869494442892398, 0.0007935738988885784797, 0.001190360848332867611, 0.001587147797777156959, 0.001983934747221446308, 0.002380721696665735222, 0.002777508646110024570, 0.003174295595554313919 ),
 .UNSPECIFIED. ) ;
#20564 = CARTESIAN_POINT ( 'NONE',  ( -5.090837523869514492, 19.35983187734362687, 7.080843742048788414 ) ) ;
#20565 = EDGE_LOOP ( 'NONE', ( #17716, #28096, #14207, #18379, #10983, #12377, #3737, #23293 ) ) ;
#20566 = CYLINDRICAL_SURFACE ( 'NONE', #2619, 9.482273699623480212 ) ;
#20567 = CARTESIAN_POINT ( 'NONE',  ( 0.1262659238204208167, 8.999114229549594057, 1.500000000000001332 ) ) ;
#20568 = ORIENTED_EDGE ( 'NONE', *, *, #23523, .F. ) ;
#20569 = DIRECTION ( 'NONE',  ( 1.000000000000000000, 0.000000000000000000, 0.000000000000000000 ) ) ;
#20570 = CARTESIAN_POINT ( 'NONE',  ( -29.61203839202723032, 15.40012917324033204, -16.55003854064094426 ) ) ;
#20571 = ORIENTED_EDGE ( 'NONE', *, *, #25937, .T. ) ;
#20572 = ORIENTED_EDGE ( 'NONE', *, *, #11520, .T. ) ;
#20573 = CARTESIAN_POINT ( 'NONE',  ( 0.000000000000000000, 5.590849009245238754, 1.500000000000000000 ) ) ;
#20574 = VERTEX_POINT ( 'NONE', #5853 ) ;
#20575 = ORIENTED_EDGE ( 'NONE', *, *, #25059, .T. ) ;
#20576 = AXIS2_PLACEMENT_3D ( 'NONE', #21322, #30535, #30840 ) ;
#20577 = CARTESIAN_POINT ( 'NONE',  ( 3.436936369909017408, 16.71530215271316422, 7.441806358946449151 ) ) ;
#20578 = VECTOR ( 'NONE', #9066, 1000.000000000000000 ) ;
#20579 = CARTESIAN_POINT ( 'NONE',  ( 49.99999999999998579, 90.00000000000001421, -75.50000000000001421 ) ) ;
#20580 = CARTESIAN_POINT ( 'NONE',  ( 5.419676874198347427, 19.25213680916389691, 18.34726407865098707 ) ) ;
#20581 = EDGE_LOOP ( 'NONE', ( #10028, #19845, #22482, #7767 ) ) ;
#20582 = CARTESIAN_POINT ( 'NONE',  ( -4.375757216953428294E-15, -39.50000000000000000, 27.50000000000000355 ) ) ;
#20583 = DIRECTION ( 'NONE',  ( 0.000000000000000000, 0.000000000000000000, 1.000000000000000000 ) ) ;
#20584 = CARTESIAN_POINT ( 'NONE',  ( 16.87674189766844890, 2.217009531549523960, 19.56050940960062690 ) ) ;
#20585 = VERTEX_POINT ( 'NONE', #10217 ) ;
#20586 = EDGE_CURVE ( 'NONE', #25466, #9598, #12303, .T. ) ;
#20587 = CARTESIAN_POINT ( 'NONE',  ( 20.71335220384823117, -27.86167394782616213, -6.500000000000000888 ) ) ;
#20588 = CARTESIAN_POINT ( 'NONE',  ( 18.02181326450768140, -8.714141732420078057, 6.018569869498933578 ) ) ;
#20589 = CARTESIAN_POINT ( 'NONE',  ( -15.35797660355606453, 12.83915183367558299, 5.652196082364323360 ) ) ;
#20590 = CARTESIAN_POINT ( 'NONE',  ( 4.592382419210019329, 19.48389062382846504, 18.64703902303423178 ) ) ;
#20591 = VERTEX_POINT ( 'NONE', #29252 ) ;
#20592 = ORIENTED_EDGE ( 'NONE', *, *, #14508, .T. ) ;
#20593 = CARTESIAN_POINT ( 'NONE',  ( 0.000000000000000000, 0.000000000000000000, 0.000000000000000000 ) ) ;
#20594 = CARTESIAN_POINT ( 'NONE',  ( 10.69247012765649174, -13.31688477309528018, 6.588756557121050683 ) ) ;
#20595 = B_SPLINE_SURFACE_WITH_KNOTS ( 'NONE', 3, 1, ( 
 ( #7404, #16913 ),
 ( #7557, #369 ),
 ( #11764, #12395 ),
 ( #2871, #2722 ),
 ( #9728, #17057 ),
 ( #23601, #23757 ),
 ( #28464, #4739 ),
 ( #21261, #26429 ),
 ( #21729, #2411 ),
 ( #26590, #24072 ),
 ( #5213, #24223 ),
 ( #29073, #5058 ),
 ( #21895, #14715 ),
 ( #30790, #7090 ),
 ( #28612, #7234 ),
 ( #524, #10047 ),
 ( #11937, #16450 ),
 ( #4591, #19240 ),
 ( #71, #14092 ),
 ( #16595, #16746 ),
 ( #14241, #9584 ),
 ( #26262, #4902 ),
 ( #14420, #23922 ),
 ( #2569, #12083 ),
 ( #28764, #3497 ),
 ( #5985, #25005 ),
 ( #29536, #22501 ),
 ( #679, #19870 ),
 ( #22652, #24859 ),
 ( #1145, #3645 ),
 ( #12551, #834 ) ),
 .UNSPECIFIED., .F., .F., .F.,
 ( 4, 3, 3, 3, 3, 3, 3, 3, 3, 3, 4 ),
 ( 2, 2 ),
 ( 0.4999999998345686647, 0.5360336730431939367, 0.5907651151589012883, 0.6456034593241830599, 0.6998270958050434309, 0.7529536536315937223, 0.8052385063053260073, 0.8575343587103997356, 0.9106564858195042023, 0.9648414833209685293, 1.000000006602610014 ),
 ( 0.000000000000000000, 1.000000000000000000 ),
 .UNSPECIFIED. ) ;
#20596 = CARTESIAN_POINT ( 'NONE',  ( -4.581181804672374014, 16.39335237280001323, 19.22654678686458141 ) ) ;
#20597 = CARTESIAN_POINT ( 'NONE',  ( -8.840471615930058036, 1.687027447297517080, 1.500000000000001332 ) ) ;
#20598 = CARTESIAN_POINT ( 'NONE',  ( 20.46975788395958418, -26.57181885929544407, -16.50000600000000262 ) ) ;
#20599 = EDGE_CURVE ( 'NONE', #30087, #17934, #29247, .T. ) ;
#20600 = FACE_OUTER_BOUND ( 'NONE', #6255, .T. ) ;
#20601 = ADVANCED_FACE ( 'NONE', ( #29560, #5695 ), #15190, .T. ) ;
#20602 = AXIS2_PLACEMENT_3D ( 'NONE', #430, #9948, #24285 ) ;
#20603 = ITEM_DEFINED_TRANSFORMATION ( 'NONE', 'NONE', #29328,  #7396 ) ;
#20604 = DIRECTION ( 'NONE',  ( 0.000000000000000000, -1.132880637372608986E-16, 1.000000000000000000 ) ) ;
#20605 = VECTOR ( 'NONE', #10524, 1000.000000000000114 ) ;
#20606 = B_SPLINE_CURVE_WITH_KNOTS ( 'NONE', 3,
 ( #2050, #23879, #14052, #11572, #16707, #18601 ),
 .UNSPECIFIED., .F., .F.,
 ( 4, 2, 4 ),
 ( 1.408367944312347353, 1.570796326794896558, 1.733224709277445763 ),
 .UNSPECIFIED. ) ;
#20607 = CARTESIAN_POINT ( 'NONE',  ( -19.87893182697125027, 2.354587536660440961, 7.643931100913408550 ) ) ;
#20608 = FACE_OUTER_BOUND ( 'NONE', #13300, .T. ) ;
#20609 = DIRECTION ( 'NONE',  ( 0.000000000000000000, -0.000000000000000000, -1.000000000000000000 ) ) ;
#20610 = ORIENTED_EDGE ( 'NONE', *, *, #23080, .T. ) ;
#20611 = CARTESIAN_POINT ( 'NONE',  ( 0.000000000000000000, -2.435693370351110282E-15, 21.50000000000000355 ) ) ;
#20612 = EDGE_LOOP ( 'NONE', ( #14147, #27422 ) ) ;
#20613 = CARTESIAN_POINT ( 'NONE',  ( 9.590471615930072247, -1.687027447297460236, 1.500000000000001332 ) ) ;
#20614 = CARTESIAN_POINT ( 'NONE',  ( -19.90131041440201187, 1.988107338454508932, 18.47531940416305929 ) ) ;
#20615 = EDGE_LOOP ( 'NONE', ( #22000, #24525, #269, #7881 ) ) ;
#20616 = DIRECTION ( 'NONE',  ( 1.000000000000000000, 0.000000000000000000, 0.000000000000000000 ) ) ;
#20617 = EDGE_CURVE ( 'NONE', #21731, #14945, #12573, .T. ) ;
#20618 = DIRECTION ( 'NONE',  ( 0.000000000000000000, 1.000000000000000000, 0.000000000000000000 ) ) ;
#20619 = EDGE_CURVE ( 'NONE', #13589, #22306, #15353, .T. ) ;
#20620 = CARTESIAN_POINT ( 'NONE',  ( -1.803040912908196569, -42.50000000000000000, 19.72227980406325898 ) ) ;
#20621 = EDGE_CURVE ( 'NONE', #16043, #1665, #8762, .T. ) ;
#20622 = CARTESIAN_POINT ( 'NONE',  ( 4.622016212553096359, -12.19167610014704906, 1.500000000000001332 ) ) ;
#20623 = DIRECTION ( 'NONE',  ( -0.000000000000000000, -1.000000000000000000, -0.000000000000000000 ) ) ;
#20624 = EDGE_CURVE ( 'NONE', #19902, #13000, #224, .T. ) ;
#20625 = CIRCLE ( 'NONE', #24584, 0.7500000000000006661 ) ;
#20626 = DIRECTION ( 'NONE',  ( 1.000000000000000000, 0.000000000000000000, 0.000000000000000000 ) ) ;
#20627 = CARTESIAN_POINT ( 'NONE',  ( 1.000541756189969433, -17.02230863066393596, 7.627891251804737927 ) ) ;
#20628 = CARTESIAN_POINT ( 'NONE',  ( -32.14097302481091134, 14.40131566728161161, 39.78047203870814741 ) ) ;
#20629 = ORIENTED_EDGE ( 'NONE', *, *, #13760, .T. ) ;
#20630 = EDGE_CURVE ( 'NONE', #3823, #24787, #14900, .T. ) ;
#20631 = CYLINDRICAL_SURFACE ( 'NONE', #6873, 9.482273699623480212 ) ;
#20632 = DIRECTION ( 'NONE',  ( 0.000000000000000000, 0.000000000000000000, 1.000000000000000000 ) ) ;
#20633 = EDGE_CURVE ( 'NONE', #13391, #27228, #26924, .T. ) ;
#20634 = CARTESIAN_POINT ( 'NONE',  ( -4.580173031741206380, 16.39361746661401043, 6.782064869129509788 ) ) ;
#20635 = DIRECTION ( 'NONE',  ( 0.000000000000000000, 0.000000000000000000, 1.000000000000000000 ) ) ;
#20636 = EDGE_CURVE ( 'NONE', #15437, #27015, #23235, .T. ) ;
#20637 = SURFACE_SIDE_STYLE ('',( #25786 ) ) ;
#20638 = DIRECTION ( 'NONE',  ( 0.000000000000000000, 0.000000000000000000, 1.000000000000000000 ) ) ;
#20639 = EDGE_LOOP ( 'NONE', ( #19047, #21629, #13047, #30408, #19391, #3971, #9945, #24435, #5393, #22264, #24197, #12988, #8527 ) ) ;
#20640 = CARTESIAN_POINT ( 'NONE',  ( -0.5297379638125987444, -19.99304770284714650, 19.85261563089511228 ) ) ;
#20641 = CARTESIAN_POINT ( 'NONE',  ( 13.22505861668195237, -42.10773672056998862, -19.50000000000000355 ) ) ;
#20642 = CARTESIAN_POINT ( 'NONE',  ( 8.636617860055906704, -41.55279347581889482, 34.58763896935784032 ) ) ;
#20643 = DIRECTION ( 'NONE',  ( 0.000000000000000000, 0.000000000000000000, 1.000000000000000000 ) ) ;
#20644 = VERTEX_POINT ( 'NONE', #14194 ) ;
#20645 = CARTESIAN_POINT ( 'NONE',  ( 26.11179934312166395, 14.04991663536889490, 41.10667063058291859 ) ) ;
#20646 = CARTESIAN_POINT ( 'NONE',  ( -25.19442432475474902, -35.44676296258422354, -19.50000000000000355 ) ) ;
#20647 = CARTESIAN_POINT ( 'NONE',  ( 26.80246859415415273, 7.028748154183637631, -1.499999999999999556 ) ) ;
#20648 = CIRCLE ( 'NONE', #24115, 2.898871837527149609 ) ;
#20649 = EDGE_CURVE ( 'NONE', #28858, #25523, #20913, .T. ) ;
#20650 = ORIENTED_EDGE ( 'NONE', *, *, #23486, .T. ) ;
#20651 = CARTESIAN_POINT ( 'NONE',  ( 49.99999999999998579, 70.00000000000000000, -75.50000000000001421 ) ) ;
#20652 = CARTESIAN_POINT ( 'NONE',  ( -5.029589720568788280, -42.14523135962111411, 34.60377126736915443 ) ) ;
#20653 = EDGE_LOOP ( 'NONE', ( #13805, #24347, #18267, #27285 ) ) ;
#20654 = CARTESIAN_POINT ( 'NONE',  ( 11.52514311384750911, -16.34582042812247238, 7.528076282304598799 ) ) ;
#20655 = EDGE_CURVE ( 'NONE', #25535, #16170, #25743, .T. ) ;
#20656 = EDGE_CURVE ( 'NONE', #21977, #3976, #2835, .T. ) ;
#20657 = CARTESIAN_POINT ( 'NONE',  ( -8.481700458822091448, -14.78796854237962677, 5.652605728828375753 ) ) ;
#20658 = CARTESIAN_POINT ( 'NONE',  ( 30.03865005752671280, -15.52610542268209848, 41.18623755349090487 ) ) ;
#20659 = ORIENTED_EDGE ( 'NONE', *, *, #983, .T. ) ;
#20660 = DIRECTION ( 'NONE',  ( 0.000000000000000000, 0.000000000000000000, 1.000000000000000000 ) ) ;
#20661 = CARTESIAN_POINT ( 'NONE',  ( 12.69001473637742983, 11.36098604102020460, 18.47056384035244037 ) ) ;
#20662 = CARTESIAN_POINT ( 'NONE',  ( -33.01877980957529957, -12.12572312222180315, 39.84356070656659909 ) ) ;
#20663 = CARTESIAN_POINT ( 'NONE',  ( -48.93034346171027238, 69.97313033977476948, 17.95007235832140324 ) ) ;
#20664 = LINE ( 'NONE', #23605, #3318 ) ;
#20665 = DIRECTION ( 'NONE',  ( -0.1423148382732850048, -0.9898214418809327952, 0.000000000000000000 ) ) ;
#20666 = AXIS2_PLACEMENT_3D ( 'NONE', #12570, #10065, #5692 ) ;
#20667 = DIRECTION ( 'NONE',  ( 0.000000000000000000, 0.000000000000000000, 1.000000000000000000 ) ) ;
#20668 = DIRECTION ( 'NONE',  ( 0.000000000000000000, 1.000000000000000000, 1.193512090021232842E-16 ) ) ;
#20669 = CARTESIAN_POINT ( 'NONE',  ( -15.35255149521179519, -7.379222211227441264, 20.25336174263950184 ) ) ;
#20670 = LINE ( 'NONE', #6491, #7099 ) ;
#20671 = ORIENTED_EDGE ( 'NONE', *, *, #2489, .F. ) ;
#20672 = VERTEX_POINT ( 'NONE', #13906 ) ;
#20673 = PLANE ( 'NONE',  #23403 ) ;
#20674 = CARTESIAN_POINT ( 'NONE',  ( -2.687479362164884034, -44.39187623478217404, -19.50000000000000355 ) ) ;
#20675 = DIRECTION ( 'NONE',  ( -1.224646799147353207E-16, 1.000000000000000000, 0.000000000000000000 ) ) ;
#20676 = EDGE_LOOP ( 'NONE', ( #9748, #1158, #26324, #22167, #7680, #2042 ) ) ;
#20677 = CARTESIAN_POINT ( 'NONE',  ( -32.98805937973593672, 0.000000000000000000, 13.00000000000000178 ) ) ;
#20678 = CARTESIAN_POINT ( 'NONE',  ( 9.035144332690526525, -14.42607982873371952, 19.60617949693493856 ) ) ;
#20679 = EDGE_CURVE ( 'NONE', #30078, #3647, #23702, .T. ) ;
#20680 = ORIENTED_EDGE ( 'NONE', *, *, #4963, .F. ) ;
#20681 = CARTESIAN_POINT ( 'NONE',  ( -16.96078254943347829, 1.685604580053745361, 5.651989602109218858 ) ) ;
#20682 = EDGE_CURVE ( 'NONE', #1222, #21772, #11424, .T. ) ;
#20683 = CARTESIAN_POINT ( 'NONE',  ( -40.00000000000002842, 80.00000000000001421, 22.49999999999983302 ) ) ;
#20684 = CARTESIAN_POINT ( 'NONE',  ( -7.404849586872397360, 36.78056030116736963, 37.49999999995792166 ) ) ;
#20685 = ORIENTED_EDGE ( 'NONE', *, *, #13613, .T. ) ;
#20686 = CARTESIAN_POINT ( 'NONE',  ( -24.35970437652574105, 13.37404834226503247, -16.55003854064094426 ) ) ;
#20687 = CIRCLE ( 'NONE', #17692, 32.32717498572581860 ) ;
#20688 = ORIENTED_EDGE ( 'NONE', *, *, #28055, .F. ) ;
#20689 = PLANE ( 'NONE',  #24491 ) ;
#20690 = CARTESIAN_POINT ( 'NONE',  ( 5.687793815610356241, -6.974883619896809606, 21.50000000000000000 ) ) ;
#20691 = ORIENTED_EDGE ( 'NONE', *, *, #20971, .T. ) ;
#20692 = CYLINDRICAL_SURFACE ( 'NONE', #17321, 0.7499999999999988898 ) ;
#20693 = CARTESIAN_POINT ( 'NONE',  ( 25.18466322232232457, -6.657711795334226856, 44.70772167919919582 ) ) ;
#20694 = CARTESIAN_POINT ( 'NONE',  ( -7.667077102831937552, 13.77986170986486592, 24.50000000000000000 ) ) ;
#20695 = DIRECTION ( 'NONE',  ( 1.000000000000000000, 0.000000000000000000, 0.000000000000000000 ) ) ;
#20696 = AXIS2_PLACEMENT_3D ( 'NONE', #6283, #22818, #15961 ) ;
#20697 = PLANE ( 'NONE',  #9772 ) ;
#20698 = CARTESIAN_POINT ( 'NONE',  ( -13.89991139849285773, 7.447222512978775022, 24.50000000000000000 ) ) ;
#20699 = CARTESIAN_POINT ( 'NONE',  ( -9.169883732660077058, -9.268939115642981008, 1.500000000000001332 ) ) ;
#20700 = DIRECTION ( 'NONE',  ( 0.000000000000000000, -0.000000000000000000, -1.000000000000000000 ) ) ;
#20701 = ORIENTED_EDGE ( 'NONE', *, *, #17756, .T. ) ;
#20702 = CARTESIAN_POINT ( 'NONE',  ( -28.84291104180498522, 28.60802559109908216, 15.82428390531839035 ) ) ;
#20703 = CARTESIAN_POINT ( 'NONE',  ( 35.76481447503399380, 5.202797454133643917, 27.50000000000001066 ) ) ;
#20704 = EDGE_LOOP ( 'NONE', ( #25722, #14111, #5657, #11041 ) ) ;
#20705 = ORIENTED_EDGE ( 'NONE', *, *, #13192, .T. ) ;
#20706 = CARTESIAN_POINT ( 'NONE',  ( 23.27838112219106392, 36.10018657900367600, -16.50000600000000262 ) ) ;
#20707 = CARTESIAN_POINT ( 'NONE',  ( -5.905415913170756426, 19.12693415355692750, 5.653912893140659257 ) ) ;
#20708 = ORIENTED_EDGE ( 'NONE', *, *, #6966, .F. ) ;
#20709 = DIRECTION ( 'NONE',  ( -0.000000000000000000, 1.132880637372608986E-16, -1.000000000000000000 ) ) ;
#20710 = VECTOR ( 'NONE', #24329, 1000.000000000000000 ) ;
#20711 = DIRECTION ( 'NONE',  ( 0.000000000000000000, 1.000000000000000000, 0.000000000000000000 ) ) ;
#20712 = FACE_BOUND ( 'NONE', #30098, .T. ) ;
#20713 = ORIENTED_EDGE ( 'NONE', *, *, #7968, .T. ) ;
#20714 = CARTESIAN_POINT ( 'NONE',  ( -32.28307784207223108, -8.475829241206282560, 37.38016955275590902 ) ) ;
#20715 = VECTOR ( 'NONE', #878, 1000.000000000000000 ) ;
#20716 = CARTESIAN_POINT ( 'NONE',  ( 5.524309650260767590, -7.706848733600972778, 21.50000000000000000 ) ) ;
#20717 = EDGE_LOOP ( 'NONE', ( #17905, #3040, #9675, #1411 ) ) ;
#20718 = VERTEX_POINT ( 'NONE', #28557 ) ;
#20719 = CARTESIAN_POINT ( 'NONE',  ( 1.000000000000008438, 16.48749217771910125, 24.50000000000000000 ) ) ;
#20720 = ORIENTED_EDGE ( 'NONE', *, *, #27366, .T. ) ;
#20721 = ORIENTED_EDGE ( 'NONE', *, *, #10693, .F. ) ;
#20722 = CIRCLE ( 'NONE', #7293, 0.5999999999999998668 ) ;
#20723 = CARTESIAN_POINT ( 'NONE',  ( -8.413215745754975217, 3.196529495465474380, 21.50000000000000000 ) ) ;
#20724 = CARTESIAN_POINT ( 'NONE',  ( 6.140972302510984804, 19.03394436102036380, 19.85261563089512293 ) ) ;
#20725 = VERTEX_POINT ( 'NONE', #8933 ) ;
#20726 = VECTOR ( 'NONE', #15079, 1000.000000000000000 ) ;
#20727 = CARTESIAN_POINT ( 'NONE',  ( 4.622016212553096359, -12.19167610014704906, 24.50000000000000000 ) ) ;
#20728 = CARTESIAN_POINT ( 'NONE',  ( -24.44496207165490276, 7.595930209050158588, 45.15942333309111945 ) ) ;
#20729 = CARTESIAN_POINT ( 'NONE',  ( 16.76146518920503325, 3.081792779576177033, 20.34789198813115263 ) ) ;
#20730 = EDGE_LOOP ( 'NONE', ( #18403, #7704, #11928, #25861 ) ) ;
#20731 = FACE_OUTER_BOUND ( 'NONE', #17209, .T. ) ;
#20732 = CARTESIAN_POINT ( 'NONE',  ( 17.92455701194924700, -8.912206770388248600, 6.755862304746362845 ) ) ;
#20733 = CARTESIAN_POINT ( 'NONE',  ( -15.93537878762121807, 12.11488692681952806, 6.233981582756856987 ) ) ;
#20734 = CIRCLE ( 'NONE', #4799, 0.7500000000000015543 ) ;
#20735 = CARTESIAN_POINT ( 'NONE',  ( 33.56327786402390245, 10.34181101807379299, 35.63689980405264635 ) ) ;
#20736 = VERTEX_POINT ( 'NONE', #9381 ) ;
#20737 = EDGE_LOOP ( 'NONE', ( #16175, #27039, #11679, #4393 ) ) ;
#20738 = FACE_OUTER_BOUND ( 'NONE', #15870, .T. ) ;
#20739 = VECTOR ( 'NONE', #23896, 1000.000000000000000 ) ;
#20740 = DIRECTION ( 'NONE',  ( -1.000000000000000000, 0.000000000000000000, 0.000000000000000000 ) ) ;
#20741 = CARTESIAN_POINT ( 'NONE',  ( -5.090837523869514492, 19.35983187734363042, 19.77662771831109367 ) ) ;
#20742 = FACE_OUTER_BOUND ( 'NONE', #30179, .T. ) ;
#20743 = AXIS2_PLACEMENT_3D ( 'NONE', #12351, #9688, #2524 ) ;
#20744 = ADVANCED_FACE ( 'NONE', ( #18593 ), #30733, .F. ) ;
#20745 = DIRECTION ( 'NONE',  ( -0.000000000000000000, -0.000000000000000000, -1.000000000000000000 ) ) ;
#20746 = VECTOR ( 'NONE', #17486, 1000.000000000000000 ) ;
#20747 = ITEM_DEFINED_TRANSFORMATION ( 'NONE', 'NONE', #18386,  #7396 ) ;
#20748 = DIRECTION ( 'NONE',  ( 0.000000000000000000, 0.000000000000000000, 1.000000000000000000 ) ) ;
#20749 = ORIENTED_EDGE ( 'NONE', *, *, #13398, .T. ) ;
#20750 = VECTOR ( 'NONE', #27441, 1000.000000000000227 ) ;
#20751 = CARTESIAN_POINT ( 'NONE',  ( -17.04208893090348909, 0.9369385374313049519, 7.366751648393900176 ) ) ;
#20752 = CARTESIAN_POINT ( 'NONE',  ( 14.32702845807336267, 13.95510847468388249, 18.73377938172349033 ) ) ;
#20753 = CARTESIAN_POINT ( 'NONE',  ( 19.87632233081032496, 2.221350112303686508, 19.08232364404840453 ) ) ;
#20754 = ORIENTED_EDGE ( 'NONE', *, *, #1025, .T. ) ;
#20755 = CARTESIAN_POINT ( 'NONE',  ( -37.99999999999999289, 90.00000000000001421, -87.50000000000000000 ) ) ;
#20756 = ORIENTED_EDGE ( 'NONE', *, *, #3465, .T. ) ;
#20757 = CARTESIAN_POINT ( 'NONE',  ( 15.94669506555478122, -6.049764716652520136, 5.704143890883081269 ) ) ;
#20758 = ADVANCED_FACE ( 'NONE', ( #23408 ), #1742, .F. ) ;
#20759 = FACE_OUTER_BOUND ( 'NONE', #11251, .T. ) ;
#20760 = VECTOR ( 'NONE', #14382, 1000.000000000000000 ) ;
#20761 = VERTEX_POINT ( 'NONE', #28408 ) ;
#20762 = CARTESIAN_POINT ( 'NONE',  ( -0.1550506074450035132, -19.99977091204053536, 7.526993102356323462 ) ) ;
#20763 = CARTESIAN_POINT ( 'NONE',  ( -6.974883619896829146, -5.687793815610328707, -3.621320343559650379 ) ) ;
#20764 = DIRECTION ( 'NONE',  ( 0.000000000000000000, 0.000000000000000000, -1.000000000000000000 ) ) ;
#20765 = CARTESIAN_POINT ( 'NONE',  ( 0.000000000000000000, -2.435693370351110282E-15, 21.50000000000000355 ) ) ;
#20766 = AXIS2_PLACEMENT_3D ( 'NONE', #26175, #282, #12147 ) ;
#20767 = DIRECTION ( 'NONE',  ( -0.000000000000000000, -0.000000000000000000, -1.000000000000000000 ) ) ;
#20769 = ADVANCED_FACE ( 'NONE', ( #2043 ), #2349, .T. ) ;
#20768 = CIRCLE ( 'NONE', #23750, 34.99999999999933920 ) ;
#20770 = CARTESIAN_POINT ( 'NONE',  ( 8.840471615930072247, -1.687027447297460236, 1.500000000000001332 ) ) ;
#20771 = CARTESIAN_POINT ( 'NONE',  ( 1.111517487559786632, -17.01912455222412390, 7.603368798681074736 ) ) ;
#20772 = CARTESIAN_POINT ( 'NONE',  ( -16.81483160676645383, 2.643882879109654915, 6.782064869129509788 ) ) ;
#20773 = EDGE_LOOP ( 'NONE', ( #4836, #18286, #20452, #248 ) ) ;
#20774 = CIRCLE ( 'NONE', #18304, 12.50000000000000000 ) ;
#20775 = DIRECTION ( 'NONE',  ( -0.000000000000000000, 1.132880637372608986E-16, -1.000000000000000000 ) ) ;
#20776 = CARTESIAN_POINT ( 'NONE',  ( -13.37849590498012908, 10.56201291617988147, 7.652108011868850923 ) ) ;
#20777 = ORIENTED_EDGE ( 'NONE', *, *, #30029, .T. ) ;
#20778 = FACE_OUTER_BOUND ( 'NONE', #30704, .T. ) ;
#20779 = CARTESIAN_POINT ( 'NONE',  ( -17.59781475975454157, -9.540531696329384914, 19.25672174529527325 ) ) ;
#20780 = AXIS2_PLACEMENT_3D ( 'NONE', #12513, #24814, #29651 ) ;
#20781 = VECTOR ( 'NONE', #28268, 1000.000000000000000 ) ;
#20782 = EDGE_CURVE ( 'NONE', #27491, #18015, #21057, .T. ) ;
#20783 = CARTESIAN_POINT ( 'NONE',  ( 32.74775157612609178, -27.21557300919356948, -19.50000000000000355 ) ) ;
#20784 = VECTOR ( 'NONE', #14097, 1000.000000000000227 ) ;
#20785 = EDGE_LOOP ( 'NONE', ( #13576, #4302, #13578, #16953 ) ) ;
#20786 = DIRECTION ( 'NONE',  ( -0.000000000000000000, -0.000000000000000000, 1.000000000000000000 ) ) ;
#20787 = CYLINDRICAL_SURFACE ( 'NONE', #20123, 1.447898107987198646 ) ;
#20788 = EDGE_CURVE ( 'NONE', #5755, #9461, #17307, .T. ) ;
#20789 = CARTESIAN_POINT ( 'NONE',  ( 38.51154267803796927, -7.181154427913921445, 32.07953739683074446 ) ) ;
#20790 = VECTOR ( 'NONE', #17642, 1000.000000000000000 ) ;
#20791 = ADVANCED_FACE ( 'NONE', ( #16095 ), #13618, .F. ) ;
#20792 = CARTESIAN_POINT ( 'NONE',  ( 11.10715495309693601, -16.63223102436629830, 7.652108011868850035 ) ) ;
#20793 = VERTEX_POINT ( 'NONE', #20755 ) ;
#20794 = DIRECTION ( 'NONE',  ( -1.000000000000000000, -0.000000000000000000, -0.000000000000000000 ) ) ;
#20795 = AXIS2_PLACEMENT_3D ( 'NONE', #20085, #15396, #15227 ) ;
#20796 = DIRECTION ( 'NONE',  ( 0.000000000000000000, -0.000000000000000000, -1.000000000000000000 ) ) ;
#20797 = CYLINDRICAL_SURFACE ( 'NONE', #1991, 0.7499999999999988898 ) ;
#20798 = AXIS2_PLACEMENT_3D ( 'NONE', #3560, #13083, #22572 ) ;
#20799 = VERTEX_POINT ( 'NONE', #1897 ) ;
#20800 = EDGE_CURVE ( 'NONE', #13440, #1001, #30265, .T. ) ;
#20801 = CARTESIAN_POINT ( 'NONE',  ( -10.40135423173695273, -40.96791945951391511, 34.57567134912213191 ) ) ;
#20802 = VERTEX_POINT ( 'NONE', #25617 ) ;
#20803 = CARTESIAN_POINT ( 'NONE',  ( -31.92585768991387951, 26.59981599196575175, -13.16665969541612036 ) ) ;
#20804 = CIRCLE ( 'NONE', #13350, 7.500000000000000000 ) ;
#20805 = ADVANCED_FACE ( 'NONE', ( #4232 ), #16238, .F. ) ;
#20806 = CARTESIAN_POINT ( 'NONE',  ( 7.724883619896791842, 5.687793815610376669, 1.500000000000001332 ) ) ;
#20807 = VECTOR ( 'NONE', #4248, 1000.000000000000000 ) ;
#20808 = CARTESIAN_POINT ( 'NONE',  ( 0.7083562926195156040, -9.056472324687613096, 13.22130136205108641 ) ) ;
#20809 = EDGE_CURVE ( 'NONE', #10117, #15581, #4538, .T. ) ;
#20810 = LINE ( 'NONE', #18182, #23781 ) ;
#20811 = AXIS2_PLACEMENT_3D ( 'NONE', #21498, #12157, #14644 ) ;
#20812 = VERTEX_POINT ( 'NONE', #12027 ) ;
#20813 = CARTESIAN_POINT ( 'NONE',  ( 24.03057240117691862, 26.57182937991349903, 1.500000000000001332 ) ) ;
#20814 = EDGE_CURVE ( 'NONE', #1364, #21915, #29016, .T. ) ;
#20815 = CARTESIAN_POINT ( 'NONE',  ( 8.817355867515813017, 2.185336383880231548, 13.22130136205108819 ) ) ;
#20816 = FACE_BOUND ( 'NONE', #18826, .T. ) ;
#20817 = CARTESIAN_POINT ( 'NONE',  ( -48.03319056991080771, 69.90398198426727561, 16.53503636252214193 ) ) ;
#20818 = AXIS2_PLACEMENT_3D ( 'NONE', #20686, #6805, #25686 ) ;
#20819 = CARTESIAN_POINT ( 'NONE',  ( -15.55757656138296419, -6.908027829044470103, 19.66962785902261501 ) ) ;
#20820 = CIRCLE ( 'NONE', #4886, 9.482273699623480212 ) ;
#20821 = DIRECTION ( 'NONE',  ( 0.000000000000000000, 1.000000000000000000, 0.000000000000000000 ) ) ;
#20822 = CARTESIAN_POINT ( 'NONE',  ( -32.32717498572578307, -1.387778780781445676E-14, 1.500000000000000000 ) ) ;
#20823 = CARTESIAN_POINT ( 'NONE',  ( 7.103144483462522807, 41.83363135865116789, 20.27275824691663431 ) ) ;
#20824 = PLANE ( 'NONE',  #18414 ) ;
#20825 = CARTESIAN_POINT ( 'NONE',  ( -15.55925901137641709, -6.904021205104065473, 19.66989035740801839 ) ) ;
#20826 = LINE ( 'NONE', #8991, #17070 ) ;
#20827 = ORIENTED_EDGE ( 'NONE', *, *, #5417, .T. ) ;
#20828 = ORIENTED_EDGE ( 'NONE', *, *, #207, .F. ) ;
#20829 = CARTESIAN_POINT ( 'NONE',  ( 33.25198511596216377, 23.59839678289867493, -8.166573069426201315 ) ) ;
#20830 = CARTESIAN_POINT ( 'NONE',  ( 10.11202017158463917, -41.14070756921186955, -1.500000000000000000 ) ) ;
#20831 = ADVANCED_FACE ( 'NONE', ( #24334 ), #9837, .T. ) ;
#20832 = DIRECTION ( 'NONE',  ( -0.8412535328311810945, -0.5406408174555976665, 0.000000000000000000 ) ) ;
#20833 = ADVANCED_FACE ( 'NONE', ( #7189 ), #12498, .F. ) ;
#20834 = ORIENTED_EDGE ( 'NONE', *, *, #10197, .F. ) ;
#20835 = AXIS2_PLACEMENT_3D ( 'NONE', #1143, #12703, #17844 ) ;
#20836 = CARTESIAN_POINT ( 'NONE',  ( 17.94577521512061580, -8.869393445417760091, 19.66989035740801839 ) ) ;
#20837 = AXIS2_PLACEMENT_3D ( 'NONE', #17260, #19747, #28963 ) ;
#20838 = DIRECTION ( 'NONE',  ( 1.000000000000000000, 0.000000000000000000, 0.000000000000000000 ) ) ;
#20839 = ORIENTED_EDGE ( 'NONE', *, *, #29610, .T. ) ;
#20840 = LINE ( 'NONE', #11498, #6813 ) ;
#20841 = EDGE_CURVE ( 'NONE', #9598, #10553, #28264, .T. ) ;
#20842 = CIRCLE ( 'NONE', #6408, 7.500000000000013323 ) ;
#20843 = CARTESIAN_POINT ( 'NONE',  ( 15.53731853391908402, 12.59332096006128943, 6.781503518395071595 ) ) ;
#20844 = CARTESIAN_POINT ( 'NONE',  ( -13.84835643114477577, 39.75824490312070481, 34.55175125678480441 ) ) ;
#20845 = VERTEX_POINT ( 'NONE', #14818 ) ;
#20846 = CARTESIAN_POINT ( 'NONE',  ( 26.11179934312167461, -14.04991663536889313, 45.34931131770218116 ) ) ;
#20847 = ORIENTED_EDGE ( 'NONE', *, *, #24263, .T. ) ;
#20848 = ADVANCED_FACE ( 'NONE', ( #24165 ), #3408, .T. ) ;
#20849 = LINE ( 'NONE', #30375, #11563 ) ;
#20850 = CARTESIAN_POINT ( 'NONE',  ( -47.14142842854255377, 69.79466010243307039, 59.50000000000029843 ) ) ;
#20851 = ORIENTED_EDGE ( 'NONE', *, *, #18369, .F. ) ;
#20852 = CARTESIAN_POINT ( 'NONE',  ( 16.76419345870816002, 3.064929150530655733, 20.34789198813115974 ) ) ;
#20853 = CARTESIAN_POINT ( 'NONE',  ( 24.75800239156184546, -7.045788922043120017, 45.01673140503397974 ) ) ;
#20854 = CARTESIAN_POINT ( 'NONE',  ( -32.32717498572578307, -1.387778780781445676E-14, -1.500000000000000000 ) ) ;
#20855 = CARTESIAN_POINT ( 'NONE',  ( 0.2321890030833198282, -17.02978461145532307, 7.500898271101006820 ) ) ;
#20856 = AXIS2_PLACEMENT_3D ( 'NONE', #2036, #21050, #13462 ) ;
#20857 = CYLINDRICAL_SURFACE ( 'NONE', #16736, 0.7500000000000006661 ) ;
#20858 = CARTESIAN_POINT ( 'NONE',  ( -17.06629969734983021, 0.6399978984115078928, 19.47952243369110548 ) ) ;
#20859 = CARTESIAN_POINT ( 'NONE',  ( -17.06456206750264215, 0.6636403356599821501, 19.58863275299554019 ) ) ;
#20860 = DIRECTION ( 'NONE',  ( -0.000000000000000000, -0.000000000000000000, -1.000000000000000000 ) ) ;
#20861 = ORIENTED_EDGE ( 'NONE', *, *, #27715, .F. ) ;
#20862 = EDGE_CURVE ( 'NONE', #10409, #12881, #25109, .T. ) ;
#20863 = EDGE_CURVE ( 'NONE', #984, #5348, #4858, .T. ) ;
#20864 = CARTESIAN_POINT ( 'NONE',  ( 9.860909911264737815, -13.90333503211346766, 20.34789198813115263 ) ) ;
#20865 = VECTOR ( 'NONE', #10413, 1000.000000000000000 ) ;
#20866 = CARTESIAN_POINT ( 'NONE',  ( 34.13832859401787800, -12.80067323710190053, 34.80090346875810781 ) ) ;
#20867 = EDGE_LOOP ( 'NONE', ( #28536, #11264, #24388, #27386 ) ) ;
#20868 = ORIENTED_EDGE ( 'NONE', *, *, #5164, .F. ) ;
#20869 = DIRECTION ( 'NONE',  ( 0.000000000000000000, 0.000000000000000000, -1.000000000000000000 ) ) ;
#20870 = CARTESIAN_POINT ( 'NONE',  ( 7.706848733600955903, 5.524309650260792459, 13.00000000000000178 ) ) ;
#20871 = ORIENTED_EDGE ( 'NONE', *, *, #12317, .F. ) ;
#20872 = CIRCLE ( 'NONE', #9925, 27.70876437800068359 ) ;
#20873 = DIRECTION ( 'NONE',  ( 0.000000000000000000, -1.132880637372608986E-16, 1.000000000000000000 ) ) ;
#20874 = DIRECTION ( 'NONE',  ( 0.000000000000000000, 0.000000000000000000, 1.000000000000000000 ) ) ;
#20875 = ORIENTED_EDGE ( 'NONE', *, *, #9017, .T. ) ;
#20876 = CARTESIAN_POINT ( 'NONE',  ( -37.16608720827707657, 36.86186943028246787, 57.49999999999999289 ) ) ;
#20877 = AXIS2_PLACEMENT_3D ( 'NONE', #24734, #30040, #19919 ) ;
#20878 = CARTESIAN_POINT ( 'NONE',  ( 16.74864137134696662, 3.161078882829541747, 5.651989602109218858 ) ) ;
#20879 = ORIENTED_EDGE ( 'NONE', *, *, #12798, .T. ) ;
#20880 = DIRECTION ( 'NONE',  ( -0.000000000000000000, 0.5000000000000005551, 0.8660254037844382635 ) ) ;
#20881 = ORIENTED_EDGE ( 'NONE', *, *, #19318, .F. ) ;
#20882 = CARTESIAN_POINT ( 'NONE',  ( -70.00000000000000000, 65.00000000000000000, 12.49999999999999112 ) ) ;
#20883 = ORIENTED_EDGE ( 'NONE', *, *, #8308, .F. ) ;
#20884 = VECTOR ( 'NONE', #25135, 1000.000000000000000 ) ;
#20885 = ORIENTED_EDGE ( 'NONE', *, *, #25615, .T. ) ;
#20886 = CYLINDRICAL_SURFACE ( 'NONE', #27090, 4.999999999999997335 ) ;
#20887 = VECTOR ( 'NONE', #13721, 1000.000000000000000 ) ;
#20888 = CARTESIAN_POINT ( 'NONE',  ( -36.00000000000000000, -2.601438916704193360, 27.50000000000001066 ) ) ;
#20889 = CARTESIAN_POINT ( 'NONE',  ( 9.195964344571798676, -14.32884674914071610, 18.71435384576123440 ) ) ;
#20890 = FACE_BOUND ( 'NONE', #4246, .T. ) ;
#20891 = ORIENTED_EDGE ( 'NONE', *, *, #24013, .T. ) ;
#20892 = CARTESIAN_POINT ( 'NONE',  ( -19.86072707285307715, 2.502642989097795478, 20.34789198813115263 ) ) ;
#20893 = CYLINDRICAL_SURFACE ( 'NONE', #24193, 7.500000000000013323 ) ;
#20894 = EDGE_CURVE ( 'NONE', #12321, #25145, #1416, .T. ) ;
#20895 = CARTESIAN_POINT ( 'NONE',  ( -15.94999985682713906, 12.09556989559485274, 6.995624166085161910 ) ) ;
#20896 = CARTESIAN_POINT ( 'NONE',  ( 4.376647981176106761, 19.53331152111370272, 19.69140814234746273 ) ) ;
#20897 = VERTEX_POINT ( 'NONE', #5774 ) ;
#20898 = ORIENTED_EDGE ( 'NONE', *, *, #21996, .F. ) ;
#20899 = EDGE_CURVE ( 'NONE', #18134, #4256, #22290, .T. ) ;
#20900 = DIRECTION ( 'NONE',  ( 0.000000000000000000, 0.000000000000000000, -1.000000000000000000 ) ) ;
#20901 = CARTESIAN_POINT ( 'NONE',  ( 32.28307784207223108, -8.475829241206289666, -16.55003854064094426 ) ) ;
#20902 = CARTESIAN_POINT ( 'NONE',  ( -5.325396069054046500, 16.18574704710536949, 20.32842677360128292 ) ) ;
#20903 = DIRECTION ( 'NONE',  ( 0.000000000000000000, 0.000000000000000000, -1.000000000000000000 ) ) ;
#20904 = AXIS2_PLACEMENT_3D ( 'NONE', #3014, #54, #11921 ) ;
#20905 = CARTESIAN_POINT ( 'NONE',  ( 9.436481611552753890, 0.9307681286968855217, 21.50000000000000000 ) ) ;
#20906 = CARTESIAN_POINT ( 'NONE',  ( -26.80246859415415273, -7.028748154183637631, -6.500000000000000888 ) ) ;
#20907 = ORIENTED_EDGE ( 'NONE', *, *, #11263, .F. ) ;
#20908 = VECTOR ( 'NONE', #18968, 1000.000000000000000 ) ;
#20909 = CARTESIAN_POINT ( 'NONE',  ( 1.367923798957373593, -19.95316478012375683, 6.788986777570696241 ) ) ;
#20910 = DIRECTION ( 'NONE',  ( 0.000000000000000000, 1.000000000000000000, 0.000000000000000000 ) ) ;
#20911 = CARTESIAN_POINT ( 'NONE',  ( 19.87928744571102513, 2.194067154482766124, 19.47728749465736797 ) ) ;
#20912 = ORIENTED_EDGE ( 'NONE', *, *, #25196, .T. ) ;
#20913 = LINE ( 'NONE', #9525, #17783 ) ;
#20914 = EDGE_LOOP ( 'NONE', ( #23059, #21418, #13454, #20482 ) ) ;
#20915 = CARTESIAN_POINT ( 'NONE',  ( 18.56338958360293745, -7.490577753534551242, 5.810767894563978686 ) ) ;
#20916 = FACE_OUTER_BOUND ( 'NONE', #16479, .T. ) ;
#20917 = ORIENTED_EDGE ( 'NONE', *, *, #26014, .F. ) ;
#20918 = CARTESIAN_POINT ( 'NONE',  ( -4.375757216953428294E-15, -39.50000000000000000, 27.50000000000000355 ) ) ;
#20919 = LINE ( 'NONE', #21, #8810 ) ;
#20920 = CARTESIAN_POINT ( 'NONE',  ( -20.58367780861512841, -27.52817754551177742, -16.50001200000000168 ) ) ;
#20921 = CIRCLE ( 'NONE', #4994, 12.50000000000000000 ) ;
#20922 = CARTESIAN_POINT ( 'NONE',  ( 8.549050687778164459, 4.102102735472485939, 13.00000000000000178 ) ) ;
#20923 = DIRECTION ( 'NONE',  ( 0.000000000000000000, 0.000000000000000000, -1.000000000000000000 ) ) ;
#20924 = CARTESIAN_POINT ( 'NONE',  ( -16.96496224101209194, 1.652369717150044659, 7.652108011868850923 ) ) ;
#20925 = ORIENTED_EDGE ( 'NONE', *, *, #18731, .T. ) ;
#20926 = CARTESIAN_POINT ( 'NONE',  ( 10.64374042650142904, 42.96126232887663576, -19.50000000000000355 ) ) ;
#20927 = DIRECTION ( 'NONE',  ( -0.000000000000000000, -0.000000000000000000, 1.000000000000000000 ) ) ;
#20928 = VERTEX_POINT ( 'NONE', #3274 ) ;
#20929 = DIRECTION ( 'NONE',  ( 1.000000000000000000, 0.000000000000000000, 0.000000000000000000 ) ) ;
#20930 = CARTESIAN_POINT ( 'NONE',  ( 11.17648341053133798, -16.60731568869664443, 7.652108011868850035 ) ) ;
#20931 = CARTESIAN_POINT ( 'NONE',  ( -5.105024945675580739, -42.22604126506273303, -1.500000000000000000 ) ) ;
#20932 = DIRECTION ( 'NONE',  ( 0.4495526574063634095, -0.8932538319083086487, 0.000000000000000000 ) ) ;
#20933 = ORIENTED_EDGE ( 'NONE', *, *, #1597, .F. ) ;
#20934 = CYLINDRICAL_SURFACE ( 'NONE', #11981, 20.00000000000000000 ) ;
#20935 = CARTESIAN_POINT ( 'NONE',  ( 16.17735844207722806, -3.336236224685152685, -0.6213203435596476032 ) ) ;
#20936 = CARTESIAN_POINT ( 'NONE',  ( 7.360936444143488799, -36.84655860943143324, 37.49999999987780086 ) ) ;
#20937 = LINE ( 'NONE', #7214, #18081 ) ;
#20938 = VERTEX_POINT ( 'NONE', #29640 ) ;
#20939 = CIRCLE ( 'NONE', #20449, 9.482273699623480212 ) ;
#20940 = CARTESIAN_POINT ( 'NONE',  ( 31.18700685317022803, -26.11823559933272421, -1.500000000000000000 ) ) ;
#20941 = DIRECTION ( 'NONE',  ( 1.000000000000000000, 0.000000000000000000, 0.000000000000000000 ) ) ;
#20942 = EDGE_LOOP ( 'NONE', ( #1372, #27679, #20949, #18404 ) ) ;
#20943 = CARTESIAN_POINT ( 'NONE',  ( 16.56213591300004850, 4.162091996074188671, 19.08844262864049313 ) ) ;
#20944 = ORIENTED_EDGE ( 'NONE', *, *, #29217, .T. ) ;
#20945 = CARTESIAN_POINT ( 'NONE',  ( -31.22486525274646851, -15.32888848509419510, 40.21560466201672313 ) ) ;
#20946 = FACE_OUTER_BOUND ( 'NONE', #8700, .T. ) ;
#20947 = DIRECTION ( 'NONE',  ( -0.000000000000000000, -0.000000000000000000, 1.000000000000000000 ) ) ;
#20948 = CARTESIAN_POINT ( 'NONE',  ( -23.62400240902268322, 9.724154461249517212, 45.23564988763775574 ) ) ;
#20949 = ORIENTED_EDGE ( 'NONE', *, *, #9543, .T. ) ;
#20950 = CARTESIAN_POINT ( 'NONE',  ( 23.26155266345719141, 12.35118985415807025, 44.42018155111519917 ) ) ;
#20951 = LINE ( 'NONE', #18640, #15857 ) ;
#20952 = EDGE_CURVE ( 'NONE', #12536, #29572, #12804, .T. ) ;
#20953 = DIRECTION ( 'NONE',  ( -0.000000000000000000, -1.000000000000000000, -0.000000000000000000 ) ) ;
#20954 = CYLINDRICAL_SURFACE ( 'NONE', #15118, 15.00000000000000000 ) ;
#20955 = ADVANCED_FACE ( 'NONE', ( #15431 ), #6080, .F. ) ;
#20956 = DIRECTION ( 'NONE',  ( -1.000000000000000000, 0.000000000000000000, 0.000000000000000000 ) ) ;
#20957 = AXIS2_PLACEMENT_3D ( 'NONE', #6983, #4638, #14141 ) ;
#20958 = EDGE_CURVE ( 'NONE', #3050, #26039, #29335, .T. ) ;
#20959 = CARTESIAN_POINT ( 'NONE',  ( 2.168404344971008868E-16, 30.50000000000000000, 24.50000000000000000 ) ) ;
#20960 = CARTESIAN_POINT ( 'NONE',  ( -12.71180423606277365, 11.31964500333551271, 19.41069149716888020 ) ) ;
#20961 = CARTESIAN_POINT ( 'NONE',  ( -14.89473990422384198, 17.79239818699320708, 1.500000000000000000 ) ) ;
#20962 = CARTESIAN_POINT ( 'NONE',  ( 3.190007960684840160, 16.77295862814622751, 19.85459532544248162 ) ) ;
#20963 = DIRECTION ( 'NONE',  ( 0.000000000000000000, 0.000000000000000000, 1.000000000000000000 ) ) ;
#20964 = EDGE_CURVE ( 'NONE', #15944, #19119, #22606, .T. ) ;
#20965 = CARTESIAN_POINT ( 'NONE',  ( -15.16517292768934055, -7.781889190071453299, 20.34789198813115263 ) ) ;
#20966 = LINE ( 'NONE', #9282, #17091 ) ;
#20967 = EDGE_LOOP ( 'NONE', ( #616, #18704, #227, #30757 ) ) ;
#20968 = ORIENTED_EDGE ( 'NONE', *, *, #25839, .T. ) ;
#20969 = LINE ( 'NONE', #28010, #16422 ) ;
#20970 = CARTESIAN_POINT ( 'NONE',  ( -22.50000000000000711, 1.387778780781445676E-14, 62.49999999999999289 ) ) ;
#20971 = EDGE_CURVE ( 'NONE', #21504, #18859, #21878, .T. ) ;
#20972 = CYLINDRICAL_SURFACE ( 'NONE', #24338, 1.000000000000010436 ) ;
#20973 = ORIENTED_EDGE ( 'NONE', *, *, #16786, .T. ) ;
#20974 = DIRECTION ( 'NONE',  ( 0.000000000000000000, 0.000000000000000000, 1.000000000000000000 ) ) ;
#20975 = CARTESIAN_POINT ( 'NONE',  ( -6.481689221575673621, 15.79948487156523207, 19.61324152429827450 ) ) ;
#20976 = EDGE_CURVE ( 'NONE', #21169, #4121, #27266, .T. ) ;
#20977 = CARTESIAN_POINT ( 'NONE',  ( 6.225165711324285311, 19.02535939286849498, 6.974106381145714018 ) ) ;
#20978 = EDGE_CURVE ( 'NONE', #24015, #8550, #16793, .T. ) ;
#20979 = ORIENTED_EDGE ( 'NONE', *, *, #7849, .F. ) ;
#20980 = CARTESIAN_POINT ( 'NONE',  ( -16.82311188420106518, 2.597149461308116081, 6.310736198168394928 ) ) ;
#20981 = B_SPLINE_CURVE_WITH_KNOTS ( 'NONE', 3,
 ( #27963, #6590, #17326, #779, #14523, #14670, #28722, #26856, #29176, #7664, #7985, #2669 ),
 .UNSPECIFIED., .F., .F.,
 ( 4, 2, 2, 2, 2, 4 ),
 ( 0.000000000000000000, 0.001930342444571962182, 0.002895513666857931455, 0.003860684889143900511, 0.005791027333715810868, 0.007721369778287722092 ),
 .UNSPECIFIED. ) ;
#20982 = DIRECTION ( 'NONE',  ( 1.000000000000000000, 0.000000000000000000, 0.000000000000000000 ) ) ;
#20983 = VECTOR ( 'NONE', #11477, 1000.000000000000114 ) ;
#20984 = DIRECTION ( 'NONE',  ( -0.000000000000000000, -0.000000000000000000, 1.000000000000000000 ) ) ;
#20985 = CARTESIAN_POINT ( 'NONE',  ( -27.32656920039229220, 30.33072541150529844, 30.01477169192959238 ) ) ;
#20986 = VERTEX_POINT ( 'NONE', #29490 ) ;
#20987 = CARTESIAN_POINT ( 'NONE',  ( 6.899999999999999467, -5.196152422706639129, -9.000000000000000000 ) ) ;
#20988 = DIRECTION ( 'NONE',  ( 0.6707505147970024284, 0.7416830501633134842, 0.000000000000000000 ) ) ;
#20989 = DIRECTION ( 'NONE',  ( 0.000000000000000000, 0.000000000000000000, 1.000000000000000000 ) ) ;
#20990 = VERTEX_POINT ( 'NONE', #15269 ) ;
#20991 = CARTESIAN_POINT ( 'NONE',  ( -39.87350638641186862, -4.706224724276806270, -6.500000000000000888 ) ) ;
#20992 = EDGE_CURVE ( 'NONE', #1147, #20089, #12959, .T. ) ;
#20993 = DIRECTION ( 'NONE',  ( -0.000000000000000000, -0.000000000000000000, 1.000000000000000000 ) ) ;
#20994 = EDGE_CURVE ( 'NONE', #28062, #18437, #14808, .T. ) ;
#20995 = CIRCLE ( 'NONE', #21489, 0.7499999999999988898 ) ;
#20996 = CARTESIAN_POINT ( 'NONE',  ( 12.08030320849306527, -42.07844615544671996, -16.50000000000000355 ) ) ;
#20997 = CARTESIAN_POINT ( 'NONE',  ( 19.72466756933792453, 3.412884783584984927, 7.627891251804737927 ) ) ;
#20998 = EDGE_CURVE ( 'NONE', #17105, #2982, #16056, .T. ) ;
#20999 = EDGE_CURVE ( 'NONE', #11391, #1364, #24272, .T. ) ;
#21000 = DIRECTION ( 'NONE',  ( 1.000000000000000000, 0.000000000000000000, 0.000000000000000000 ) ) ;
#21001 = CARTESIAN_POINT ( 'NONE',  ( 12.24063095261064404, 4.490763173670002217, 24.50000000000000000 ) ) ;
#21002 = CARTESIAN_POINT ( 'NONE',  ( -19.96032475228487968, 1.513912977174403984, 19.58863275299554019 ) ) ;
#21003 = DIRECTION ( 'NONE',  ( -1.000000000000000000, 0.000000000000000000, 0.000000000000000000 ) ) ;
#21004 = ORIENTED_EDGE ( 'NONE', *, *, #15663, .T. ) ;
#21005 = EDGE_CURVE ( 'NONE', #2231, #23836, #4657, .T. ) ;
#21006 = CARTESIAN_POINT ( 'NONE',  ( -6.384540597206719958, 15.83495921350553459, 7.158811349119587497 ) ) ;
#21007 = CIRCLE ( 'NONE', #14543, 47.00000000000000000 ) ;
#21008 = FACE_OUTER_BOUND ( 'NONE', #15073, .T. ) ;
#21009 = ORIENTED_EDGE ( 'NONE', *, *, #27487, .F. ) ;
#21010 = ORIENTED_EDGE ( 'NONE', *, *, #22370, .F. ) ;
#21011 = EDGE_CURVE ( 'NONE', #21045, #8550, #15913, .T. ) ;
#21012 = CARTESIAN_POINT ( 'NONE',  ( -48.71096830872563999, 69.96160472130995345, 57.45356189401062608 ) ) ;
#21013 = EDGE_CURVE ( 'NONE', #11068, #12149, #22781, .T. ) ;
#21014 = DIRECTION ( 'NONE',  ( 1.000000000000000000, 0.000000000000000000, 0.000000000000000000 ) ) ;
#21015 = ORIENTED_EDGE ( 'NONE', *, *, #13975, .T. ) ;
#21016 = CARTESIAN_POINT ( 'NONE',  ( 12.43449883826692215, 11.65450130491726455, 20.34789198813115263 ) ) ;
#21017 = DIRECTION ( 'NONE',  ( -1.000000000000000000, 0.000000000000000000, 0.000000000000000000 ) ) ;
#21018 = ORIENTED_EDGE ( 'NONE', *, *, #5401, .T. ) ;
#21019 = VECTOR ( 'NONE', #26744, 1000.000000000000000 ) ;
#21020 = CARTESIAN_POINT ( 'NONE',  ( -15.57266529552203416, 38.96488032230103471, -1.500000000000000000 ) ) ;
#21021 = CARTESIAN_POINT ( 'NONE',  ( -33.48610676296128474, -10.91424270342314529, 39.78047203871652471 ) ) ;
#21022 = EDGE_CURVE ( 'NONE', #7139, #20003, #9185, .T. ) ;
#21023 = VERTEX_POINT ( 'NONE', #25878 ) ;
#21024 = VERTEX_POINT ( 'NONE', #28206 ) ;
#21025 = EDGE_CURVE ( 'NONE', #17954, #23193, #4509, .T. ) ;
#21026 = DIRECTION ( 'NONE',  ( 0.000000000000000000, -0.000000000000000000, -1.000000000000000000 ) ) ;
#21027 = EDGE_CURVE ( 'NONE', #17876, #1692, #23771, .T. ) ;
#21028 = VERTEX_POINT ( 'NONE', #6687 ) ;
#21029 = VERTEX_POINT ( 'NONE', #25717 ) ;
#21030 = DIRECTION ( 'NONE',  ( 0.000000000000000000, 0.000000000000000000, -1.000000000000000000 ) ) ;
#21031 = CARTESIAN_POINT ( 'NONE',  ( 0.000000000000000000, 0.000000000000000000, 1.500000000000001332 ) ) ;
#21032 = AXIS2_PLACEMENT_3D ( 'NONE', #20464, #15780, #29841 ) ;
#21033 = EDGE_CURVE ( 'NONE', #29154, #28301, #356, .T. ) ;
#21035 = AXIS2_PLACEMENT_3D ( 'NONE', #23434, #28293, #9707 ) ;
#21034 = CARTESIAN_POINT ( 'NONE',  ( -14.93131746134411308, -8.256826158467614363, 18.45571264222804331 ) ) ;
#21036 = VECTOR ( 'NONE', #20287, 1000.000000000000000 ) ;
#21037 = CARTESIAN_POINT ( 'NONE',  ( -24.18487066411278619, 13.30660647122584983, 47.39613942427950377 ) ) ;
#21038 = CARTESIAN_POINT ( 'NONE',  ( 16.86769344895231271, 2.296683858978088466, 18.90679857307105749 ) ) ;
#21039 = ORIENTED_EDGE ( 'NONE', *, *, #5986, .F. ) ;
#21040 = CARTESIAN_POINT ( 'NONE',  ( -16.83986259902029659, 2.499865191129257092, 18.80699882434806369 ) ) ;
#21041 = CARTESIAN_POINT ( 'NONE',  ( 7.044370898287875882, -38.75167233872380734, 34.49999999999997868 ) ) ;
#21042 = CARTESIAN_POINT ( 'NONE',  ( -15.49619650379777269, 12.67194488555738019, 20.32367522806703874 ) ) ;
#21043 = CARTESIAN_POINT ( 'NONE',  ( 4.690664460087335286, 19.46058373524397922, 20.13759033520874908 ) ) ;
#21044 = VERTEX_POINT ( 'NONE', #13577 ) ;
#21045 = VERTEX_POINT ( 'NONE', #13719 ) ;
#21046 = CARTESIAN_POINT ( 'NONE',  ( -77.99999999999998579, 42.50000000000000711, 24.50000000000000000 ) ) ;
#21047 = FACE_OUTER_BOUND ( 'NONE', #17731, .T. ) ;
#21048 = LINE ( 'NONE', #18581, #30278 ) ;
#21049 = LINE ( 'NONE', #9211, #7660 ) ;
#21050 = DIRECTION ( 'NONE',  ( -0.000000000000000000, -0.000000000000000000, 1.000000000000000000 ) ) ;
#21051 = DIRECTION ( 'NONE',  ( 0.9594929736144992560, 0.2817325568414232317, 0.000000000000000000 ) ) ;
#21052 = ORIENTED_EDGE ( 'NONE', *, *, #16213, .F. ) ;
#21053 = CARTESIAN_POINT ( 'NONE',  ( 0.4897477184365106040, -19.99444548460947146, 5.652912763329819512 ) ) ;
#21054 = DIRECTION ( 'NONE',  ( 1.000000000000000000, 0.000000000000000000, 0.000000000000000000 ) ) ;
#21055 = DIRECTION ( 'NONE',  ( 1.000000000000000000, 0.000000000000000000, 0.000000000000000000 ) ) ;
#21056 = ORIENTED_EDGE ( 'NONE', *, *, #24795, .F. ) ;
#21057 = LINE ( 'NONE', #21204, #15290 ) ;
#21058 = ORIENTED_EDGE ( 'NONE', *, *, #30517, .F. ) ;
#21059 = EDGE_CURVE ( 'NONE', #16129, #27888, #23207, .T. ) ;
#21060 = CARTESIAN_POINT ( 'NONE',  ( 16.11883921216213267, -5.620554474281632906, 6.041646659195333058 ) ) ;
#21061 = CIRCLE ( 'NONE', #24544, 6.000000000000005329 ) ;
#21062 = B_SPLINE_CURVE_WITH_KNOTS ( 'NONE', 3,
 ( #215, #7555, #19239, #11763 ),
 .UNSPECIFIED., .F., .F.,
 ( 4, 4 ),
 ( 3.018024802580205417E-07, 0.007932103453629116285 ),
 .UNSPECIFIED. ) ;
#21063 = CARTESIAN_POINT ( 'NONE',  ( -8.049211243008397076, 43.20179514148429689, -16.50000000000000000 ) ) ;
#21064 = ORIENTED_EDGE ( 'NONE', *, *, #4227, .F. ) ;
#21065 = CARTESIAN_POINT ( 'NONE',  ( 17.09326798506966938, 34.76714281734690815, 27.50000000000000355 ) ) ;
#21066 = AXIS2_PLACEMENT_3D ( 'NONE', #51, #11748, #2390 ) ;
#21067 = DIRECTION ( 'NONE',  ( 0.000000000000000000, 0.000000000000000000, 1.000000000000000000 ) ) ;
#21068 = LINE ( 'NONE', #16246, #5527 ) ;
#21069 = CARTESIAN_POINT ( 'NONE',  ( -22.21046885174908070, -23.49239644259612447, -16.50001200000000523 ) ) ;
#21070 = CARTESIAN_POINT ( 'NONE',  ( -5.973959739936659297, 19.10558604466630683, 20.34789198813115263 ) ) ;
#21071 = CARTESIAN_POINT ( 'NONE',  ( 7.562559277181973627, -5.881244434206257310, 1.500000000000001332 ) ) ;
#21072 = ORIENTED_EDGE ( 'NONE', *, *, #29471, .F. ) ;
#21073 = CARTESIAN_POINT ( 'NONE',  ( 15.60593903839432706, -6.823719261784717993, 5.774779864094944593 ) ) ;
#21074 = AXIS2_PLACEMENT_3D ( 'NONE', #17528, #525, #5214 ) ;
#21075 = LINE ( 'NONE', #9238, #16347 ) ;
#21076 = FACE_OUTER_BOUND ( 'NONE', #7001, .T. ) ;
#21077 = VERTEX_POINT ( 'NONE', #30405 ) ;
#21078 = FACE_OUTER_BOUND ( 'NONE', #2061, .T. ) ;
#21079 = AXIS2_PLACEMENT_3D ( 'NONE', #8262, #15110, #26990 ) ;
#21080 = CARTESIAN_POINT ( 'NONE',  ( 39.99999999999998579, -0.000000000000000000, 22.49999999999999289 ) ) ;
#21081 = CIRCLE ( 'NONE', #24567, 0.7500000000000006661 ) ;
#21082 = CARTESIAN_POINT ( 'NONE',  ( -34.07766914599908148, -21.40380666528021081, -1.500000000000000000 ) ) ;
#21083 = LINE ( 'NONE', #9553, #10100 ) ;
#21084 = ORIENTED_EDGE ( 'NONE', *, *, #5777, .T. ) ;
#21085 = DIRECTION ( 'NONE',  ( -0.000000000000000000, -0.000000000000000000, -1.000000000000000000 ) ) ;
#21086 = DIRECTION ( 'NONE',  ( -1.000000000000000000, 0.000000000000000000, 0.000000000000000000 ) ) ;
#21087 = CARTESIAN_POINT ( 'NONE',  ( 32.88898149417357075, -18.05935166304826822, 37.50000000004457945 ) ) ;
#21088 = CARTESIAN_POINT ( 'NONE',  ( -5.971396161871753705, 19.08775596758252391, 7.652108011868850035 ) ) ;
#21089 = VERTEX_POINT ( 'NONE', #5439 ) ;
#21090 = ORIENTED_EDGE ( 'NONE', *, *, #23526, .F. ) ;
#21091 = DIRECTION ( 'NONE',  ( -1.000000000000000000, 0.000000000000000000, 0.000000000000000000 ) ) ;
#21092 = CARTESIAN_POINT ( 'NONE',  ( -4.163336342344337027E-14, -1.387778780781445676E-14, 1.500000000000000000 ) ) ;
#21093 = ORIENTED_EDGE ( 'NONE', *, *, #27873, .F. ) ;
#21094 = VERTEX_POINT ( 'NONE', #4802 ) ;
#21095 = CARTESIAN_POINT ( 'NONE',  ( -31.57476163834523675, -15.10795358447669301, 35.75454235600954433 ) ) ;
#21096 = B_SPLINE_SURFACE_WITH_KNOTS ( 'NONE', 3, 1, ( 
 ( #22630, #8472 ),
 ( #1281, #11103 ),
 ( #17976, #20902 ),
 ( #15459, #4220 ),
 ( #8302, #18121 ),
 ( #27796, #6571 ),
 ( #10790, #17819 ),
 ( #27335, #27484 ),
 ( #25291, #25602 ),
 ( #6103, #15938 ),
 ( #20741, #25131 ),
 ( #22789, #16083 ),
 ( #5962, #3615 ),
 ( #3938, #10957 ),
 ( #13458, #22941 ),
 ( #29977, #20596 ),
 ( #1594, #30120 ),
 ( #8752, #4076 ),
 ( #13605, #1730 ),
 ( #11245, #8921 ),
 ( #18442, #24001 ),
 ( #2034, #12169 ),
 ( #19180, #25897 ),
 ( #2186, #11558 ),
 ( #13894, #4992 ),
 ( #23396, #16691 ),
 ( #30427, #28089 ),
 ( #9065, #30570 ),
 ( #7023, #14504 ),
 ( #26199, #9366 ),
 ( #16532, #11704 ) ),
 .UNSPECIFIED., .F., .F., .F.,
 ( 4, 3, 3, 3, 3, 3, 3, 3, 3, 3, 4 ),
 ( 2, 2 ),
 ( 0.000000000000000000, 0.05425176834609614362, 0.1085332949128348518, 0.1623767749169379715, 0.2157504826133058717, 0.2688657508888169789, 0.3218907763505471364, 0.3749548578363334772, 0.4282048033836237666, 0.4818374082110496448, 0.4999999999131651274 ),
 ( 0.000000000000000000, 1.000000000000000000 ),
 .UNSPECIFIED. ) ;
#21097 = ORIENTED_EDGE ( 'NONE', *, *, #18141, .F. ) ;
#21098 = CARTESIAN_POINT ( 'NONE',  ( -0.3742200966386520222, -20.01457288233325116, 20.05479082170252525 ) ) ;
#21099 = EDGE_CURVE ( 'NONE', #4518, #3697, #1671, .T. ) ;
#21100 = VECTOR ( 'NONE', #11178, 1000.000000000000000 ) ;
#21101 = CARTESIAN_POINT ( 'NONE',  ( -9.646222981487627024, -17.54010295177084089, 6.560937769032974209 ) ) ;
#21102 = DIRECTION ( 'NONE',  ( -0.2817325568414296710, 0.9594929736144973687, -0.000000000000000000 ) ) ;
#21103 = CARTESIAN_POINT ( 'NONE',  ( 1.733314906354235241, -16.98782497260185664, 19.69140814234746273 ) ) ;
#21104 = EDGE_LOOP ( 'NONE', ( #20432, #23078, #11628, #1849, #7703, #11216, #25244 ) ) ;
#21105 = CARTESIAN_POINT ( 'NONE',  ( 18.67144399175156977, -7.167977615171047923, 7.161525567826885208 ) ) ;
#21106 = CARTESIAN_POINT ( 'NONE',  ( 16.56617216130305437, 4.143135851887535637, 6.329955581934031628 ) ) ;
#21107 = CARTESIAN_POINT ( 'NONE',  ( 33.78553873773097393, 24.40792641592722134, -16.50000000000000000 ) ) ;
#21108 = CARTESIAN_POINT ( 'NONE',  ( 23.17581250239727808, -34.50630206824671831, 1.499999999999999778 ) ) ;
#21109 = ORIENTED_EDGE ( 'NONE', *, *, #5951, .F. ) ;
#21110 = LINE ( 'NONE', #1800, #10797 ) ;
#21111 = CARTESIAN_POINT ( 'NONE',  ( -15.57492749417079736, -6.866608492821396403, 19.47784884541372463 ) ) ;
#21112 = CARTESIAN_POINT ( 'NONE',  ( -13.38160118231794371, 10.55829203257429860, 18.34798005863078885 ) ) ;
#21113 = CARTESIAN_POINT ( 'NONE',  ( -35.78163722268750746, 27.43648963448195133, -1.500000000000000000 ) ) ;
#21114 = CARTESIAN_POINT ( 'NONE',  ( 3.089102459976073689, 16.79563822436285747, 19.61324152429827095 ) ) ;
#21115 = CARTESIAN_POINT ( 'NONE',  ( -18.44536497093016436, -7.731176935556636209, 19.08232364404839743 ) ) ;
#21116 = DIRECTION ( 'NONE',  ( -0.000000000000000000, -1.000000000000000000, -0.000000000000000000 ) ) ;
#21117 = CARTESIAN_POINT ( 'NONE',  ( 33.42925964089141644, -11.06161099612213228, 35.54550565580004928 ) ) ;
#21118 = VERTEX_POINT ( 'NONE', #23829 ) ;
#21119 = VERTEX_POINT ( 'NONE', #16668 ) ;
#21120 = LINE ( 'NONE', #16005, #9972 ) ;
#21121 = VECTOR ( 'NONE', #24747, 1000.000000000000000 ) ;
#21122 = CARTESIAN_POINT ( 'NONE',  ( 19.64114023396890829, 37.13592150528549496, -1.500000000000000000 ) ) ;
#21123 = CYLINDRICAL_SURFACE ( 'NONE', #6431, 0.7500000000000024425 ) ;
#21124 = ORIENTED_EDGE ( 'NONE', *, *, #7435, .F. ) ;
#21125 = CARTESIAN_POINT ( 'NONE',  ( 15.63062718528784956, -6.770321384568312340, 20.25336174263950184 ) ) ;
#21126 = CARTESIAN_POINT ( 'NONE',  ( 4.930301257365633738, 16.29355789806661647, 7.080843742048788414 ) ) ;
#21127 = EDGE_CURVE ( 'NONE', #18437, #8048, #4968, .T. ) ;
#21128 = ORIENTED_EDGE ( 'NONE', *, *, #7912, .F. ) ;
#21129 = CARTESIAN_POINT ( 'NONE',  ( 4.373786442354534287, 16.46525014965065026, 20.29090034784956131 ) ) ;
#21130 = DIRECTION ( 'NONE',  ( 0.1423148382732889461, 0.9898214418809321291, 0.000000000000000000 ) ) ;
#21131 = CARTESIAN_POINT ( 'NONE',  ( -7.256763913191261572, -43.38079396975989965, -16.50000000000000000 ) ) ;
#21132 = CARTESIAN_POINT ( 'NONE',  ( -20.48943103728710469, 31.49987920171448508, 37.49999999989595523 ) ) ;
#21133 = ORIENTED_EDGE ( 'NONE', *, *, #25501, .T. ) ;
#21134 = PLANE ( 'NONE',  #13845 ) ;
#21135 = ADVANCED_FACE ( 'NONE', ( #7471 ), #30850, .T. ) ;
#21136 = CARTESIAN_POINT ( 'NONE',  ( -4.340342926365016396, -8.430595340551244377, 21.50000000000000000 ) ) ;
#21137 = CARTESIAN_POINT ( 'NONE',  ( -15.17333614897415828, 13.03014763290140721, 7.626647697317578078 ) ) ;
#21138 = ORIENTED_EDGE ( 'NONE', *, *, #23671, .F. ) ;
#21139 = CARTESIAN_POINT ( 'NONE',  ( -15.30782679199506546, -7.476958555467158263, 7.595116371587256054 ) ) ;
#21140 = AXIS2_PLACEMENT_3D ( 'NONE', #23475, #2437, #23333 ) ;
#21141 = CARTESIAN_POINT ( 'NONE',  ( 16.81773250897601812, 2.696729702855533262, 18.47056384035244037 ) ) ;
#21142 = CYLINDRICAL_SURFACE ( 'NONE', #6262, 9.482273699623480212 ) ;
#21143 = CARTESIAN_POINT ( 'NONE',  ( 1.048387430112781127, -44.07656352898515451, -16.50000000000000355 ) ) ;
#21144 = FACE_OUTER_BOUND ( 'NONE', #20704, .T. ) ;
#21145 = CARTESIAN_POINT ( 'NONE',  ( 25.88604317058895532, -6.345278376181630264, 48.34797144667699342 ) ) ;
#21146 = EDGE_CURVE ( 'NONE', #22916, #24186, #7341, .T. ) ;
#21147 = CARTESIAN_POINT ( 'NONE',  ( -47.00000000000000000, 87.00000000000001421, 0.000000000000000000 ) ) ;
#21148 = LINE ( 'NONE', #30668, #7016 ) ;
#21149 = FACE_OUTER_BOUND ( 'NONE', #4809, .T. ) ;
#21150 = ORIENTED_EDGE ( 'NONE', *, *, #1930, .T. ) ;
#21151 = CARTESIAN_POINT ( 'NONE',  ( 10.04466414020356524, -13.77914355952371928, 20.32367522806703874 ) ) ;
#21152 = CARTESIAN_POINT ( 'NONE',  ( -39.52380524535562500, 7.028748154183637631, -11.49999999999999645 ) ) ;
#21153 = ORIENTED_EDGE ( 'NONE', *, *, #7895, .F. ) ;
#21154 = VERTEX_POINT ( 'NONE', #21335 ) ;
#21155 = CARTESIAN_POINT ( 'NONE',  ( 8.099999999999999645, 8.082668874372532992E-16, 6.600000000000001421 ) ) ;
#21156 = CARTESIAN_POINT ( 'NONE',  ( 18.33599632111990019, -7.986941774664177096, 7.652108011868850035 ) ) ;
#21157 = VERTEX_POINT ( 'NONE', #19315 ) ;
#21158 = CARTESIAN_POINT ( 'NONE',  ( -1.000000000000016875, 29.50000000000000000, 43.10779406592839536 ) ) ;
#21159 = AXIS2_PLACEMENT_3D ( 'NONE', #7503, #28709, #24007 ) ;
#21160 = EDGE_CURVE ( 'NONE', #23060, #9483, #13226, .T. ) ;
#21161 = ORIENTED_EDGE ( 'NONE', *, *, #63, .T. ) ;
#21162 = ADVANCED_FACE ( 'NONE', ( #2786 ), #9649, .T. ) ;
#21163 = DIRECTION ( 'NONE',  ( 0.000000000000000000, 0.000000000000000000, -1.000000000000000000 ) ) ;
#21164 = CARTESIAN_POINT ( 'NONE',  ( -25.07174449839133601, 6.739288358966155634, 49.03857552305944267 ) ) ;
#21165 = ORIENTED_EDGE ( 'NONE', *, *, #1487, .F. ) ;
#21166 = ORIENTED_EDGE ( 'NONE', *, *, #21494, .F. ) ;
#21167 = EDGE_CURVE ( 'NONE', #22347, #22720, #12300, .T. ) ;
#21168 = B_SPLINE_CURVE_WITH_KNOTS ( 'NONE', 3,
 ( #954, #17488, #21850, #19978 ),
 .UNSPECIFIED., .F., .F.,
 ( 4, 4 ),
 ( 2.143643656977390230E-07, 0.003421830178490238052 ),
 .UNSPECIFIED. ) ;
#21169 = VERTEX_POINT ( 'NONE', #12467 ) ;
#21170 = CIRCLE ( 'NONE', #29728, 0.7500000000000006661 ) ;
#21171 = ORIENTED_EDGE ( 'NONE', *, *, #18976, .T. ) ;
#21172 = EDGE_CURVE ( 'NONE', #11969, #7300, #13339, .T. ) ;
#21173 = ADVANCED_FACE ( 'NONE', ( #29138 ), #19938, .T. ) ;
#21174 = DIRECTION ( 'NONE',  ( 0.000000000000000000, 0.000000000000000000, 1.000000000000000000 ) ) ;
#21175 = CARTESIAN_POINT ( 'NONE',  ( -17.92585835919031823, -8.870080556897411483, 5.679672709359372185 ) ) ;
#21177 = EDGE_CURVE ( 'NONE', #1188, #22820, #15555, .T. ) ;
#21176 = AXIS2_PLACEMENT_3D ( 'NONE', #21917, #12574, #17405 ) ;
#21178 = CARTESIAN_POINT ( 'NONE',  ( -70.00000000000000000, -50.00000000000000000, 12.49999999999999112 ) ) ;
#21179 = DIRECTION ( 'NONE',  ( 0.000000000000000000, 1.000000000000000000, 1.193512090021232842E-16 ) ) ;
#21180 = CARTESIAN_POINT ( 'NONE',  ( 19.88003893156456670, 2.345734461008496474, 18.80699882434806369 ) ) ;
#21181 = ORIENTED_EDGE ( 'NONE', *, *, #293, .F. ) ;
#21182 = FACE_OUTER_BOUND ( 'NONE', #9241, .T. ) ;
#21183 = CARTESIAN_POINT ( 'NONE',  ( 26.80246859415415273, -7.028748154183637631, -1.499999999999999556 ) ) ;
#21184 = VECTOR ( 'NONE', #8269, 1000.000000000000000 ) ;
#21185 = DIRECTION ( 'NONE',  ( 1.000000000000000000, 0.000000000000000000, 0.000000000000000000 ) ) ;
#21186 = ORIENTED_EDGE ( 'NONE', *, *, #24407, .T. ) ;
#21187 = ORIENTED_EDGE ( 'NONE', *, *, #20862, .F. ) ;
#21188 = PLANE ( 'NONE',  #7834 ) ;
#21189 = CARTESIAN_POINT ( 'NONE',  ( -5.881244434206279514, -6.812559277181949646, 21.50000000000000000 ) ) ;
#21190 = FACE_OUTER_BOUND ( 'NONE', #29714, .T. ) ;
#21191 = CARTESIAN_POINT ( 'NONE',  ( 0.000000000000000000, 80.00000000000000000, 0.000000000000000000 ) ) ;
#21192 = CARTESIAN_POINT ( 'NONE',  ( -23.16735716920977950, 10.90794401664034652, 45.15085036613763236 ) ) ;
#21193 =( GEOMETRIC_REPRESENTATION_CONTEXT ( 3 ) GLOBAL_UNCERTAINTY_ASSIGNED_CONTEXT ( ( #2353 ) ) GLOBAL_UNIT_ASSIGNED_CONTEXT ( ( #10820, #10508, #22198 ) ) REPRESENTATION_CONTEXT ( 'NONE', 'WORKASPACE' ) );
#21194 = EDGE_CURVE ( 'NONE', #14945, #16254, #1879, .T. ) ;
#21195 = CARTESIAN_POINT ( 'NONE',  ( -5.380257496407077511, 19.26296000801971786, 5.849008070840540974 ) ) ;
#21196 = VERTEX_POINT ( 'NONE', #25071 ) ;
#21197 = EDGE_CURVE ( 'NONE', #6692, #2256, #22719, .T. ) ;
#21198 = CARTESIAN_POINT ( 'NONE',  ( -17.04337418722500530, 0.9225192032720770374, 5.951255046771932733 ) ) ;
#21199 = DIRECTION ( 'NONE',  ( -1.000000000000000000, 0.000000000000000000, 0.000000000000000000 ) ) ;
#21200 = EDGE_CURVE ( 'NONE', #21892, #15430, #24600, .T. ) ;
#21201 = DIRECTION ( 'NONE',  ( -1.000000000000000000, 0.000000000000000000, 0.000000000000000000 ) ) ;
#21202 = ORIENTED_EDGE ( 'NONE', *, *, #15723, .T. ) ;
#21203 = VECTOR ( 'NONE', #9508, 1000.000000000000000 ) ;
#21204 = CARTESIAN_POINT ( 'NONE',  ( -5.131244434206278626, -6.812559277181949646, -3.621320343559650379 ) ) ;
#21205 = ORIENTED_EDGE ( 'NONE', *, *, #28277, .T. ) ;
#21206 = CARTESIAN_POINT ( 'NONE',  ( 15.81416324982726884, -6.360572704771158214, 5.652196082364320695 ) ) ;
#21207 = AXIS2_PLACEMENT_3D ( 'NONE', #11434, #20623, #27819 ) ;
#21208 = AXIS2_PLACEMENT_3D ( 'NONE', #7223, #30057, #18781 ) ;
#21209 = DIRECTION ( 'NONE',  ( 1.000000000000000000, 0.000000000000000000, 0.000000000000000000 ) ) ;
#21210 = ORIENTED_EDGE ( 'NONE', *, *, #22538, .T. ) ;
#21211 = CARTESIAN_POINT ( 'NONE',  ( 36.00220402031282418, -2.441524372556627132, 27.50000000000000355 ) ) ;
#21212 = ADVANCED_FACE ( 'NONE', ( #15082 ), #13231, .F. ) ;
#21213 = CARTESIAN_POINT ( 'NONE',  ( 0.07568653364412146478, -1.751902528157389893, 9.000000000000000000 ) ) ;
#21214 = CARTESIAN_POINT ( 'NONE',  ( 10.08428597779237457, -13.75408489919876587, 18.34938820207545263 ) ) ;
#21215 = CARTESIAN_POINT ( 'NONE',  ( -18.40637697828373476, -7.823545570387639536, 7.156831654632813233 ) ) ;
#21216 = CARTESIAN_POINT ( 'NONE',  ( -5.755751318732965416, 16.05090033862148502, 20.32367522806703874 ) ) ;
#21217 = VECTOR ( 'NONE', #14918, 1000.000000000000000 ) ;
#21218 = CIRCLE ( 'NONE', #4803, 0.7500000000000006661 ) ;
#21219 = CYLINDRICAL_SURFACE ( 'NONE', #21338, 9.482273699623480212 ) ;
#21220 = DIRECTION ( 'NONE',  ( 1.000000000000000000, 0.000000000000000000, 0.000000000000000000 ) ) ;
#21221 = CARTESIAN_POINT ( 'NONE',  ( 6.301234758012599357, -6.543385983536367689, -1.500000000000002442 ) ) ;
#21222 = ORIENTED_EDGE ( 'NONE', *, *, #13635, .T. ) ;
#21223 = CARTESIAN_POINT ( 'NONE',  ( 15.39831020855742594, -7.255125275872136292, 6.385774490351132648 ) ) ;
#21224 = CARTESIAN_POINT ( 'NONE',  ( 19.64114023396890829, 37.13592150528549496, -1.500000000000000000 ) ) ;
#21225 = CARTESIAN_POINT ( 'NONE',  ( 26.36764545593179676, 31.31467416275351923, 1.500000000000000000 ) ) ;
#21226 = ORIENTED_EDGE ( 'NONE', *, *, #27289, .F. ) ;
#21227 = FACE_OUTER_BOUND ( 'NONE', #18205, .T. ) ;
#21228 = VECTOR ( 'NONE', #19694, 1000.000000000000000 ) ;
#21229 = CARTESIAN_POINT ( 'NONE',  ( -14.97070905019798026, -8.177877011708881483, 20.25542030744407640 ) ) ;
#21230 = LINE ( 'NONE', #2686, #18708 ) ;
#21231 = EDGE_CURVE ( 'NONE', #2392, #5492, #17296, .T. ) ;
#21232 = ADVANCED_FACE ( 'NONE', ( #29919 ), #12929, .T. ) ;
#21233 = CIRCLE ( 'NONE', #30700, 20.00000000000000000 ) ;
#21234 = CARTESIAN_POINT ( 'NONE',  ( -2.516121109503243414, -8.728722367416576589, -1.500000000000002887 ) ) ;
#21235 = EDGE_LOOP ( 'NONE', ( #28577, #3194, #4479, #11540 ) ) ;
#21236 = CARTESIAN_POINT ( 'NONE',  ( 1.750000000000008660, 16.48749217771910125, 24.50000000000000000 ) ) ;
#21237 = CYLINDRICAL_SURFACE ( 'NONE', #26102, 0.7500000000000006661 ) ;
#21238 = CARTESIAN_POINT ( 'NONE',  ( 39.00145586610816650, 0.5332248899570756207, 32.23263252817133662 ) ) ;
#21239 = DIRECTION ( 'NONE',  ( -1.000000000000000000, 0.000000000000000000, 0.000000000000000000 ) ) ;
#21240 = EDGE_LOOP ( 'NONE', ( #6644, #14899, #23538, #10184 ) ) ;
#21241 = CARTESIAN_POINT ( 'NONE',  ( -50.00000000000000000, 50.00000000000000000, 12.49999999999999112 ) ) ;
#21242 = AXIS2_PLACEMENT_3D ( 'NONE', #11768, #21268, #11168 ) ;
#21243 = CARTESIAN_POINT ( 'NONE',  ( -34.07766914599911701, 21.40380666528009002, -1.500000000000000000 ) ) ;
#21244 = DIRECTION ( 'NONE',  ( -1.000000000000000000, 0.000000000000000000, 0.000000000000000000 ) ) ;
#21245 = ORIENTED_EDGE ( 'NONE', *, *, #26838, .T. ) ;
#21246 = VECTOR ( 'NONE', #15233, 1000.000000000000000 ) ;
#21247 = EDGE_LOOP ( 'NONE', ( #10140, #6963, #3272, #21018 ) ) ;
#21248 = CARTESIAN_POINT ( 'NONE',  ( 6.812559277181973627, -5.881244434206257310, -3.621320343559650379 ) ) ;
#21249 = VECTOR ( 'NONE', #29180, 1000.000000000000000 ) ;
#21250 = VERTEX_POINT ( 'NONE', #6202 ) ;
#21251 = B_SPLINE_CURVE_WITH_KNOTS ( 'NONE', 3,
 ( #11706, #23400, #18445, #25455, #27947, #30572, #18125, #11415, #16086, #9212, #23236, #23543, #18277, #6573, #18583, #27639, #16386, #4531, #25606, #15774, #4222, #28091, #18728, #6717, #28239, #6868, #19036, #28550, #18890, #16851, #2337, #3390, #27101, #9368, #26957, #3230, #7342, #29444, #23861, #17582, #12752, #2504, #12603, #12019, #5580, #19759, #14506, #21367, #26366, #17438, #29288, #15074, #28401, #3084, #7181, #24590, #14348, #26202, #5, #4833, #5722, #24442, #4995, #22256, #22096, #15216, #11868, #14186, #727, #22413 ),
 .UNSPECIFIED., .F., .F.,
 ( 4, 2, 2, 2, 2, 2, 2, 2, 2, 2, 2, 2, 2, 2, 2, 2, 2, 2, 2, 2, 2, 2, 2, 2, 2, 2, 2, 2, 2, 2, 2, 2, 2, 2, 4 ),
 ( 0.1181738554856288231, 0.1255522872445846982, 0.1273968951843236774, 0.1292415031240626566, 0.1329307190035405872, 0.1366199348830185178, 0.1384645428227574970, 0.1403091507624964485, 0.1476875825214522819, 0.1495321904611912334, 0.1513767984009302126, 0.1550660142804081154, 0.1587552301598860460, 0.1605998380996250252, 0.1624444460393639766, 0.1698228777983198101, 0.1735120936777977130, 0.1753567016175366922, 0.1772013095572756436, 0.1845797413162314771, 0.1882689571957093799, 0.1901135651354483314, 0.1919581730751873105, 0.1993366048341431163, 0.2030258207136210746, 0.2048704286533600261, 0.2067150365930989775, 0.2140934683520547832, 0.2159380762917937346, 0.2177826842315326861, 0.2214719001110106167, 0.2288503318699664502, 0.2306949398097054016, 0.2325395477494443530, 0.2362287636289222559 ),
 .UNSPECIFIED. ) ;
#21252 = CARTESIAN_POINT ( 'NONE',  ( 0.5572578986459487682, -17.03042415120789954, 18.36582235739946611 ) ) ;
#21253 = AXIS2_PLACEMENT_3D ( 'NONE', #1034, #3212, #14914 ) ;
#21254 = CARTESIAN_POINT ( 'NONE',  ( -9.668922248712510381, -17.52764785324846741, 6.892848776733236704 ) ) ;
#21255 = AXIS2_PLACEMENT_3D ( 'NONE', #20454, #29973, #11242 ) ;
#21256 = CARTESIAN_POINT ( 'NONE',  ( 4.985742441158911298, 16.27537970825794389, 19.60617949693493500 ) ) ;
#21257 = CARTESIAN_POINT ( 'NONE',  ( 0.8531715179115267889, -17.02613171184587770, 20.34789198813115263 ) ) ;
#21258 = ORIENTED_EDGE ( 'NONE', *, *, #30198, .F. ) ;
#21259 = CARTESIAN_POINT ( 'NONE',  ( 23.96732207937828463, 33.98584080152456011, -1.500000000000003997 ) ) ;
#21260 = DIRECTION ( 'NONE',  ( -1.000000000000000000, 0.000000000000000000, 0.000000000000000000 ) ) ;
#21261 = CARTESIAN_POINT ( 'NONE',  ( 14.45824965121216366, 13.84471048730597786, 18.56793045041961321 ) ) ;
#21262 = DIRECTION ( 'NONE',  ( 1.000000000000000000, 0.000000000000000000, 0.000000000000000000 ) ) ;
#21263 = CIRCLE ( 'NONE', #14296, 6.000000000000005329 ) ;
#21264 = ORIENTED_EDGE ( 'NONE', *, *, #29414, .F. ) ;
#21265 = B_SPLINE_CURVE_WITH_KNOTS ( 'NONE', 3,
 ( #3625, #13146, #27805, #6110 ),
 .UNSPECIFIED., .F., .F.,
 ( 4, 4 ),
 ( 2.143643656964904170E-07, 0.003421830178490233715 ),
 .UNSPECIFIED. ) ;
#21266 = AXIS2_PLACEMENT_3D ( 'NONE', #7199, #16712, #327 ) ;
#21267 = VECTOR ( 'NONE', #19027, 1000.000000000000000 ) ;
#21268 = DIRECTION ( 'NONE',  ( 0.000000000000000000, 0.000000000000000000, 1.000000000000000000 ) ) ;
#21269 = DIRECTION ( 'NONE',  ( -0.000000000000000000, 1.132880637372608986E-16, -1.000000000000000000 ) ) ;
#21270 = CARTESIAN_POINT ( 'NONE',  ( 25.64627119138473432, 23.40052582045089480, -16.50001200000000168 ) ) ;
#21271 = CARTESIAN_POINT ( 'NONE',  ( 20.71335220384823117, -27.86167394782616213, -6.500000000000000888 ) ) ;
#21272 = LINE ( 'NONE', #25519, #20376 ) ;
#21273 = CIRCLE ( 'NONE', #24784, 1.447898107987198646 ) ;
#21274 = CARTESIAN_POINT ( 'NONE',  ( -18.45502384974596310, -7.754294478968729365, 19.66989035740801839 ) ) ;
#21275 = CARTESIAN_POINT ( 'NONE',  ( 33.21329855679436349, -9.207353758468071803, 36.29150586549661028 ) ) ;
#21276 = AXIS2_PLACEMENT_3D ( 'NONE', #19353, #9998, #21676 ) ;
#21277 = EDGE_CURVE ( 'NONE', #15068, #25416, #29790, .T. ) ;
#21278 = VERTEX_POINT ( 'NONE', #29298 ) ;
#21279 = ORIENTED_EDGE ( 'NONE', *, *, #8765, .T. ) ;
#21280 = AXIS2_PLACEMENT_3D ( 'NONE', #7695, #2851, #7540 ) ;
#21281 = ADVANCED_FACE ( 'NONE', ( #3558 ), #8401, .F. ) ;
#21282 = DIRECTION ( 'NONE',  ( -0.000000000000000000, -0.000000000000000000, 1.000000000000000000 ) ) ;
#21283 = CARTESIAN_POINT ( 'NONE',  ( -5.105024945673440229, 42.22604126506271172, -1.500000000000000000 ) ) ;
#21284 = LINE ( 'NONE', #15855, #30333 ) ;
#21285 = LINE ( 'NONE', #7109, #1688 ) ;
#21286 = ORIENTED_EDGE ( 'NONE', *, *, #6448, .F. ) ;
#21287 = DIRECTION ( 'NONE',  ( 1.000000000000000000, 0.000000000000000000, 0.000000000000000000 ) ) ;
#21288 = VECTOR ( 'NONE', #22038, 1000.000000000000000 ) ;
#21289 = CARTESIAN_POINT ( 'NONE',  ( 17.99082164042340537, -8.777603813954270251, 19.87181966307587544 ) ) ;
#21290 = CARTESIAN_POINT ( 'NONE',  ( 5.721595087358980258, 19.18273663903466542, 5.749228751562096562 ) ) ;
#21291 = CONICAL_SURFACE ( 'NONE', #24287, 9.000000000000000000, 1.047197551196600296 ) ;
#21292 = EDGE_LOOP ( 'NONE', ( #20121, #24622, #13395, #1027 ) ) ;
#21293 = CARTESIAN_POINT ( 'NONE',  ( 5.524396280439210827, 19.24072699314231727, 20.32842677360128292 ) ) ;
#21294 = VECTOR ( 'NONE', #28397, 1000.000000000000000 ) ;
#21295 = DIRECTION ( 'NONE',  ( 0.000000000000000000, 0.000000000000000000, -1.000000000000000000 ) ) ;
#21296 = AXIS2_PLACEMENT_3D ( 'NONE', #10550, #20370, #13520 ) ;
#21297 = DIRECTION ( 'NONE',  ( 1.000000000000000000, 0.000000000000000000, 0.000000000000000000 ) ) ;
#21298 = CARTESIAN_POINT ( 'NONE',  ( -33.48680455852475291, 16.92615973923613737, 37.49999999998726707 ) ) ;
#21299 = VERTEX_POINT ( 'NONE', #10422 ) ;
#21300 = DIRECTION ( 'NONE',  ( -0.000000000000000000, -1.000000000000000000, -0.000000000000000000 ) ) ;
#21301 = DIRECTION ( 'NONE',  ( -0.000000000000000000, 1.132880637372608986E-16, -1.000000000000000000 ) ) ;
#21302 = CARTESIAN_POINT ( 'NONE',  ( -1.438332125858111432, 8.884323311075791096, 21.50000000000000000 ) ) ;
#21303 = AXIS2_PLACEMENT_3D ( 'NONE', #8557, #22570, #24921 ) ;
#21304 = ORIENTED_EDGE ( 'NONE', *, *, #21611, .F. ) ;
#21305 = CIRCLE ( 'NONE', #29296, 1.447898107987198646 ) ;
#21306 = CARTESIAN_POINT ( 'NONE',  ( -18.45239215198388294, -7.760673075470066351, 6.310736198168394928 ) ) ;
#21307 = CARTESIAN_POINT ( 'NONE',  ( -39.52380524535562500, 7.028748154183637631, -11.49999999999999645 ) ) ;
#21308 = CARTESIAN_POINT ( 'NONE',  ( -26.36764545593177544, 31.31467416275353344, 1.500000000000000000 ) ) ;
#21309 = FACE_OUTER_BOUND ( 'NONE', #24839, .T. ) ;
#21310 = DIRECTION ( 'NONE',  ( -0.000000000000000000, -0.000000000000000000, -1.000000000000000000 ) ) ;
#21311 = LINE ( 'NONE', #4637, #19016 ) ;
#21312 = CARTESIAN_POINT ( 'NONE',  ( -17.00407983531364309, 1.321870115990432248, 20.29915277494337644 ) ) ;
#21313 = CARTESIAN_POINT ( 'NONE',  ( 4.510281037539698445E-13, -4.926614671774132148E-13, 65.49999999999998579 ) ) ;
#21314 = ORIENTED_EDGE ( 'NONE', *, *, #620, .F. ) ;
#21315 = AXIS2_PLACEMENT_3D ( 'NONE', #150, #4374, #4682 ) ;
#21316 = VECTOR ( 'NONE', #13808, 999.9999999999998863 ) ;
#21317 = CARTESIAN_POINT ( 'NONE',  ( 11.63559590357233553, -16.28893981701509830, 20.13759033520874908 ) ) ;
#21318 = CARTESIAN_POINT ( 'NONE',  ( -5.278755796068719697, -7.392982946727062021, -1.500000000000002665 ) ) ;
#21319 = AXIS2_PLACEMENT_3D ( 'NONE', #17457, #26657, #2795 ) ;
#21320 = ORIENTED_EDGE ( 'NONE', *, *, #96, .T. ) ;
#21321 = EDGE_LOOP ( 'NONE', ( #7506, #22864, #19354, #25261 ) ) ;
#21322 = CARTESIAN_POINT ( 'NONE',  ( -37.99999999999933920, 4.653657836759860688E-15, 85.49999999999998579 ) ) ;
#21323 = ADVANCED_FACE ( 'NONE', ( #27428 ), #17594, .F. ) ;
#21324 = ORIENTED_EDGE ( 'NONE', *, *, #14766, .T. ) ;
#21325 = VECTOR ( 'NONE', #29377, 1000.000000000000000 ) ;
#21326 = CARTESIAN_POINT ( 'NONE',  ( 12.71820101047898532, 11.32761398983758383, 20.19668224736330941 ) ) ;
#21327 = FACE_BOUND ( 'NONE', #15018, .T. ) ;
#21328 = ORIENTED_EDGE ( 'NONE', *, *, #14707, .T. ) ;
#21329 = B_SPLINE_CURVE_WITH_KNOTS ( 'NONE', 3,
 ( #1550, #27754, #3895, #22902, #20561, #9326, #19150, #2005, #19001, #12135, #28512, #23815, #6676, #11817, #28195, #26163, #23508, #4499 ),
 .UNSPECIFIED., .F., .F.,
 ( 4, 2, 2, 2, 2, 2, 2, 2, 4 ),
 ( 0.000000000000000000, 0.0003967869494442920588, 0.0007935738988885811902, 0.001190360848332870213, 0.001587147797777159128, 0.001983934747221448476, 0.002380721696665736957, 0.002777508646110026305, 0.003174295595554314786 ),
 .UNSPECIFIED. ) ;
#21330 = CARTESIAN_POINT ( 'NONE',  ( 15.94669506555476701, -6.049764716652515695, 18.39992786714538298 ) ) ;
#21331 = B_SPLINE_CURVE_WITH_KNOTS ( 'NONE', 3,
 ( #26118, #4144, #4749, #16152, #14103 ),
 .UNSPECIFIED., .F., .F.,
 ( 4, 1, 4 ),
 ( 6.145237473689745305E-19, 0.002536462521843869077, 0.005072925043687738153 ),
 .UNSPECIFIED. ) ;
#21332 = CARTESIAN_POINT ( 'NONE',  ( 16.55580462840119438, 4.191719245021452878, 19.47783254395485031 ) ) ;
#21333 = CARTESIAN_POINT ( 'NONE',  ( -8.884323311075783991, -1.438332125858144295, 1.500000000000001332 ) ) ;
#21334 = ORIENTED_EDGE ( 'NONE', *, *, #17564, .F. ) ;
#21335 = CARTESIAN_POINT ( 'NONE',  ( 6.437793815610357129, -6.974883619896809606, 1.500000000000001332 ) ) ;
#21336 = EDGE_LOOP ( 'NONE', ( #26092, #2003, #23189, #26884 ) ) ;
#21337 = CARTESIAN_POINT ( 'NONE',  ( 3.221450758838616757, -1.621276839356792454, 1.500000000000000000 ) ) ;
#21338 = AXIS2_PLACEMENT_3D ( 'NONE', #24025, #2526, #23717 ) ;
#21339 = VECTOR ( 'NONE', #16649, 1000.000000000000000 ) ;
#21340 = CIRCLE ( 'NONE', #26846, 0.7500000000000007772 ) ;
#21341 = ORIENTED_EDGE ( 'NONE', *, *, #823, .T. ) ;
#21342 = CARTESIAN_POINT ( 'NONE',  ( 0.000000000000000000, 1.699320956058915452E-16, -1.500000000000001776 ) ) ;
#21343 = CARTESIAN_POINT ( 'NONE',  ( -0.1790877314264358866, -17.02136788083136310, 19.66962785902261501 ) ) ;
#21344 = CARTESIAN_POINT ( 'NONE',  ( 1.208994807697890916, -19.98122169387826830, 7.196036389296800451 ) ) ;
#21345 = CARTESIAN_POINT ( 'NONE',  ( 0.000000000000000000, 1.699320956058915452E-16, -1.500000000000001776 ) ) ;
#21346 = CARTESIAN_POINT ( 'NONE',  ( -32.81350286003733885, 0.000000000000000000, -6.500000000000000888 ) ) ;
#21347 = CARTESIAN_POINT ( 'NONE',  ( 19.85228648261877282, 2.570616772381428383, 18.55820869691756769 ) ) ;
#21348 = EDGE_CURVE ( 'NONE', #28044, #2431, #5868, .T. ) ;
#21349 = ORIENTED_EDGE ( 'NONE', *, *, #985, .F. ) ;
#21350 = EDGE_CURVE ( 'NONE', #17431, #8898, #18212, .T. ) ;
#21351 = CARTESIAN_POINT ( 'NONE',  ( 9.402326492558371385, -14.20083561530969973, 7.500898271101006820 ) ) ;
#21352 = COLOUR_RGB ( '',0.7921568627450980005, 0.8196078431372548767, 0.9333333333333333481 ) ;
#21353 = CARTESIAN_POINT ( 'NONE',  ( 20.71901075410115922, -32.31713536268975417, 34.50000000000000000 ) ) ;
#21354 = CARTESIAN_POINT ( 'NONE',  ( -13.83017030316319840, 10.00185174541443978, 7.366751648393900176 ) ) ;
#21355 = CARTESIAN_POINT ( 'NONE',  ( -19.91398265452221850, -1.852915226174651986, 1.500000000000001332 ) ) ;
#21356 = EDGE_CURVE ( 'NONE', #23071, #24333, #11643, .T. ) ;
#21357 = ORIENTED_EDGE ( 'NONE', *, *, #25163, .T. ) ;
#21358 = ORIENTED_EDGE ( 'NONE', *, *, #9534, .T. ) ;
#21359 = CYLINDRICAL_SURFACE ( 'NONE', #1865, 1.447898107987198646 ) ;
#21360 = CARTESIAN_POINT ( 'NONE',  ( -2.552544031601109875, 42.50000000001772804, -1.500000000000009992 ) ) ;
#21361 = EDGE_CURVE ( 'NONE', #1033, #19689, #18378, .T. ) ;
#21362 = PLANE ( 'NONE',  #26291 ) ;
#21363 = PRODUCT ( 'Cartridge Outer Retaining Cylinder', 'Cartridge Outer Retaining Cylinder', '', ( #19575 ) ) ;
#21364 = DIRECTION ( 'NONE',  ( 0.000000000000000000, -0.000000000000000000, -1.000000000000000000 ) ) ;
#21365 = DIRECTION ( 'NONE',  ( 1.000000000000000000, 0.000000000000000000, 0.000000000000000000 ) ) ;
#21366 = CIRCLE ( 'NONE', #7424, 1.000000000000010436 ) ;
#21367 = CARTESIAN_POINT ( 'NONE',  ( -29.73518274310997356, -22.29727607186046967, 27.50000000000001421 ) ) ;
#21368 = CARTESIAN_POINT ( 'NONE',  ( -25.48568755041063838, -12.36160011285428517, 24.50000000000000000 ) ) ;
#21369 = EDGE_CURVE ( 'NONE', #7440, #2660, #25388, .T. ) ;
#21370 = ORIENTED_EDGE ( 'NONE', *, *, #18180, .T. ) ;
#21371 = CARTESIAN_POINT ( 'NONE',  ( -4.163336342344337027E-14, 1.387778780781445676E-14, 1.500000000000000000 ) ) ;
#21372 = CIRCLE ( 'NONE', #2461, 9.084132297865673777 ) ;
#21373 = EDGE_CURVE ( 'NONE', #5348, #30675, #11357, .T. ) ;
#21374 = CARTESIAN_POINT ( 'NONE',  ( -4.163336342344337027E-14, 1.387778780781445676E-14, 62.49999999999999289 ) ) ;
#21375 = CARTESIAN_POINT ( 'NONE',  ( 7.856594496258195726, 4.390207617113981442, 21.50000000000000000 ) ) ;
#21376 = EDGE_LOOP ( 'NONE', ( #13720, #14034, #18848, #26289 ) ) ;
#21377 = ADVANCED_FACE ( 'NONE', ( #1982 ), #28172, .F. ) ;
#21378 = VERTEX_POINT ( 'NONE', #27887 ) ;
#21379 = CARTESIAN_POINT ( 'NONE',  ( 16.02447511960551552, -5.858916503155154665, 5.810767894563978686 ) ) ;
#21380 = CARTESIAN_POINT ( 'NONE',  ( -14.26810496549984997, 41.32347559458636255, -16.50000000000000355 ) ) ;
#21381 = EDGE_LOOP ( 'NONE', ( #12735, #9456, #3846, #17282 ) ) ;
#21382 = CARTESIAN_POINT ( 'NONE',  ( 35.93079460107085055, 2.525230334074545890, 27.50000000000000355 ) ) ;
#21383 = DIRECTION ( 'NONE',  ( -0.000000000000000000, 1.132880637372608986E-16, -1.000000000000000000 ) ) ;
#21384 = CARTESIAN_POINT ( 'NONE',  ( 10.69237140622465887, -13.31695822555149178, 19.47952243369110548 ) ) ;
#21385 = CARTESIAN_POINT ( 'NONE',  ( -18.10021843967230737, -8.508777197197414210, 7.652108011868850923 ) ) ;
#21386 = CARTESIAN_POINT ( 'NONE',  ( -4.608906612435655248, -7.730328572437724866, 21.50000000000000000 ) ) ;
#21387 = LINE ( 'NONE', #6740, #25321 ) ;
#21388 = EDGE_CURVE ( 'NONE', #9030, #2587, #7879, .T. ) ;
#21389 = ORIENTED_EDGE ( 'NONE', *, *, #30393, .T. ) ;
#21390 = EDGE_CURVE ( 'NONE', #8048, #23566, #1408, .T. ) ;
#21391 =( GEOMETRIC_REPRESENTATION_CONTEXT ( 3 ) GLOBAL_UNCERTAINTY_ASSIGNED_CONTEXT ( ( #25469 ) ) GLOBAL_UNIT_ASSIGNED_CONTEXT ( ( #30684, #26329, #25871 ) ) REPRESENTATION_CONTEXT ( 'NONE', 'WORKASPACE' ) );
#21392 = CARTESIAN_POINT ( 'NONE',  ( 37.98493438987956949, 11.12428508576150143, -1.500000000000000000 ) ) ;
#21393 = CARTESIAN_POINT ( 'NONE',  ( 0.000000000000000000, 0.000000000000000000, 0.000000000000000000 ) ) ;
#21394 = ADVANCED_FACE ( 'NONE', ( #9009 ), #16020, .T. ) ;
#21395 = ORIENTED_EDGE ( 'NONE', *, *, #29042, .F. ) ;
#21396 = CARTESIAN_POINT ( 'NONE',  ( -7.856594496258223259, -4.390207617113929039, -3.621320343559650379 ) ) ;
#21397 = DIRECTION ( 'NONE',  ( 0.000000000000000000, 0.000000000000000000, 1.000000000000000000 ) ) ;
#21398 = DIRECTION ( 'NONE',  ( -0.000000000000000000, 0.000000000000000000, 1.000000000000000000 ) ) ;
#21399 = ADVANCED_FACE ( 'NONE', ( #1675 ), #21134, .T. ) ;
#21400 = CARTESIAN_POINT ( 'NONE',  ( 4.537114060968175266, 16.41705816690543784, 7.526951045817044772 ) ) ;
#21401 = DIRECTION ( 'NONE',  ( 0.000000000000000000, 0.000000000000000000, 1.000000000000000000 ) ) ;
#21402 = ORIENTED_EDGE ( 'NONE', *, *, #20971, .F. ) ;
#21403 =( LENGTH_UNIT ( ) NAMED_UNIT ( * ) SI_UNIT ( .MILLI., .METRE. ) );
#21404 = DIRECTION ( 'NONE',  ( -0.000000000000000000, -0.000000000000000000, 1.000000000000000000 ) ) ;
#21405 = CARTESIAN_POINT ( 'NONE',  ( 37.36706805913578222, 12.24402983531209621, 34.92319840363951045 ) ) ;
#21406 = ADVANCED_FACE ( 'NONE', ( #13988 ), #23342, .T. ) ;
#21407 = FACE_OUTER_BOUND ( 'NONE', #7603, .T. ) ;
#21408 = ORIENTED_EDGE ( 'NONE', *, *, #28232, .F. ) ;
#21409 = CARTESIAN_POINT ( 'NONE',  ( -13.99459037269021344, 9.787106705890307623, 6.917457548096559883 ) ) ;
#21410 = VERTEX_POINT ( 'NONE', #25536 ) ;
#21411 = CARTESIAN_POINT ( 'NONE',  ( -37.98493438988125348, -11.12428508575252728, -1.500000000000000000 ) ) ;
#21412 = LINE ( 'NONE', #19686, #14925 ) ;
#21413 = ORIENTED_EDGE ( 'NONE', *, *, #30153, .F. ) ;
#21414 = ORIENTED_EDGE ( 'NONE', *, *, #12862, .F. ) ;
#21415 = CARTESIAN_POINT ( 'NONE',  ( -40.00000000000002842, 90.00000000000001421, 17.49999999999982947 ) ) ;
#21416 = CIRCLE ( 'NONE', #1017, 14.52510309069108807 ) ;
#21417 = EDGE_LOOP ( 'NONE', ( #7954, #24780, #3515, #3585 ) ) ;
#21418 = ORIENTED_EDGE ( 'NONE', *, *, #5741, .T. ) ;
#21419 = CARTESIAN_POINT ( 'NONE',  ( -0.4401303402703798384, -20.01320326077420830, 18.71435384576123440 ) ) ;
#21420 = ADVANCED_FACE ( 'NONE', ( #30653 ), #9301, .F. ) ;
#21421 = CARTESIAN_POINT ( 'NONE',  ( -9.648244442396759268, -17.53899143774386005, 6.672349528511551497 ) ) ;
#21422 = EDGE_CURVE ( 'NONE', #11315, #4164, #27755, .T. ) ;
#21423 = CARTESIAN_POINT ( 'NONE',  ( 4.049916833591939103, 16.55712665779026693, 20.34789198813115263 ) ) ;
#21424 = CARTESIAN_POINT ( 'NONE',  ( 0.6820093937066836753, -20.00641896168560052, 20.29915277494337644 ) ) ;
#21425 = ORIENTED_EDGE ( 'NONE', *, *, #9795, .F. ) ;
#21426 = AXIS2_PLACEMENT_3D ( 'NONE', #19533, #4718, #26408 ) ;
#21427 = CARTESIAN_POINT ( 'NONE',  ( 18.33599632111990019, -7.986941774664177096, 7.652108011868850035 ) ) ;
#21428 = CARTESIAN_POINT ( 'NONE',  ( -4.622016212553093695, -12.19167610014704906, 1.500000000000001332 ) ) ;
#21429 = CARTESIAN_POINT ( 'NONE',  ( 1.368946144808714793, -19.95309466511746166, 19.21940439362674624 ) ) ;
#21430 = DIRECTION ( 'NONE',  ( 0.000000000000000000, -0.5000000000000005551, -0.8660254037844382635 ) ) ;
#21431 = ORIENTED_EDGE ( 'NONE', *, *, #27895, .F. ) ;
#21432 = B_SPLINE_CURVE_WITH_KNOTS ( 'NONE', 3,
 ( #24981, #12684, #8156, #17659, #27177, #29839, #5808, #15000, #3008, #24363, #13142, #10328, #22634, #17349, #17981, #27490, #12526, #12987, #15305, #19843 ),
 .UNSPECIFIED., .F., .F.,
 ( 4, 2, 2, 2, 2, 2, 2, 2, 2, 4 ),
 ( 0.000000000000000000, 0.06249999999999968081, 0.1249999999999993616, 0.1874999999999990286, 0.2187499999999989453, 0.2499999999999988343, 0.3124999999999991118, 0.3749999999999992784, 0.4374999999999995559, 0.4999999999999997780 ),
 .UNSPECIFIED. ) ;
#21433 = CARTESIAN_POINT ( 'NONE',  ( -52.16608720827707657, -51.86186943028246787, 97.07879600563551037 ) ) ;
#21434 = CARTESIAN_POINT ( 'NONE',  ( -14.70205207497230582, -8.690259054815006934, 6.560937769032974209 ) ) ;
#21435 = DIRECTION ( 'NONE',  ( 0.000000000000000000, 0.000000000000000000, -1.000000000000000000 ) ) ;
#21436 = CARTESIAN_POINT ( 'NONE',  ( 24.03057240117690441, -26.57182937991349903, -6.499999999999999112 ) ) ;
#21437 = LINE ( 'NONE', #79, #15378 ) ;
#21438 = CARTESIAN_POINT ( 'NONE',  ( -7.106594496258223259, -4.390207617113929039, -3.621320343559650379 ) ) ;
#21439 = CARTESIAN_POINT ( 'NONE',  ( -37.99999999999999289, 90.00000000000001421, -34.49999999999999289 ) ) ;
#21440 = ORIENTED_EDGE ( 'NONE', *, *, #21422, .F. ) ;
#21441 = ORIENTED_EDGE ( 'NONE', *, *, #9162, .F. ) ;
#21442 = CARTESIAN_POINT ( 'NONE',  ( 33.57242512142757818, 24.08458161877725701, -13.16663720014176775 ) ) ;
#21443 = CARTESIAN_POINT ( 'NONE',  ( -12.56641067637752229, 40.32935944495016400, -1.500000000000000000 ) ) ;
#21444 = CARTESIAN_POINT ( 'NONE',  ( -14.88094288956370548, 13.38957456607570506, 7.359006845440219102 ) ) ;
#21445 = LINE ( 'NONE', #16766, #24587 ) ;
#21446 = ORIENTED_EDGE ( 'NONE', *, *, #18130, .T. ) ;
#21447 = DIRECTION ( 'NONE',  ( 1.000000000000000000, 0.000000000000000000, 0.000000000000000000 ) ) ;
#21448 = DIRECTION ( 'NONE',  ( 1.000000000000000000, 0.000000000000000000, 0.000000000000000000 ) ) ;
#21449 = CARTESIAN_POINT ( 'NONE',  ( 5.730668117466259481, 19.18033075515274888, 7.557577766377196582 ) ) ;
#21450 = ORIENTED_EDGE ( 'NONE', *, *, #17433, .F. ) ;
#21451 = CARTESIAN_POINT ( 'NONE',  ( 5.913643690471324987, 19.12442985200254597, 20.12545155307891065 ) ) ;
#21452 = CARTESIAN_POINT ( 'NONE',  ( -33.46566279634666330, -23.92259740141309976, -11.50000000000000000 ) ) ;
#21453 = DIRECTION ( 'NONE',  ( 0.8910248307962433945, -0.4539545692076750738, 0.000000000000000000 ) ) ;
#21454 = CARTESIAN_POINT ( 'NONE',  ( -36.92102040520508410, 13.75791949449672380, 34.88729987039940994 ) ) ;
#21455 = EDGE_LOOP ( 'NONE', ( #3950, #26929, #8861, #5306 ) ) ;
#21456 = DIRECTION ( 'NONE',  ( 0.000000000000000000, 1.000000000000000000, 1.193512090021232842E-16 ) ) ;
#21457 = VECTOR ( 'NONE', #19232, 1000.000000000000000 ) ;
#21458 = CARTESIAN_POINT ( 'NONE',  ( -26.80246859415414917, -7.028748154183644736, -16.50000000000000000 ) ) ;
#21459 = AXIS2_PLACEMENT_3D ( 'NONE', #7782, #12478, #7952 ) ;
#21460 = LINE ( 'NONE', #102, #11359 ) ;
#21461 = VERTEX_POINT ( 'NONE', #28344 ) ;
#21462 = CARTESIAN_POINT ( 'NONE',  ( -15.43012792948217538, -7.204331193346492412, 7.429667576816606278 ) ) ;
#21463 = DIRECTION ( 'NONE',  ( 1.000000000000000000, 0.000000000000000000, 0.000000000000000000 ) ) ;
#21464 = FACE_BOUND ( 'NONE', #28078, .T. ) ;
#21465 = CARTESIAN_POINT ( 'NONE',  ( 0.3440795696225480427, -17.03036400190297783, 5.749228751562096562 ) ) ;
#21466 = DIRECTION ( 'NONE',  ( 1.000000000000000000, 0.000000000000000000, 0.000000000000000000 ) ) ;
#21467 = DIRECTION ( 'NONE',  ( -0.000000000000000000, -0.000000000000000000, 1.000000000000000000 ) ) ;
#21468 = CARTESIAN_POINT ( 'NONE',  ( -17.06646200723452722, 0.6378183210065171416, 19.25672174529527325 ) ) ;
#21469 = CARTESIAN_POINT ( 'NONE',  ( 37.99999999999999289, 90.00000000000001421, -75.50000000000001421 ) ) ;
#21470 = ORIENTED_EDGE ( 'NONE', *, *, #14349, .F. ) ;
#21471 = LINE ( 'NONE', #28362, #10263 ) ;
#21472 = CARTESIAN_POINT ( 'NONE',  ( 1.195154792889395967, 9.406652940105990623, 1.500000000000001332 ) ) ;
#21473 = ORIENTED_EDGE ( 'NONE', *, *, #6869, .T. ) ;
#21474 = ORIENTED_EDGE ( 'NONE', *, *, #6728, .T. ) ;
#21475 = CARTESIAN_POINT ( 'NONE',  ( 4.512576344050351018, 19.48449473338812510, 19.96797677718664232 ) ) ;
#21476 = CARTESIAN_POINT ( 'NONE',  ( -70.00000000000000000, 70.00000000000000000, -92.50000000000000000 ) ) ;
#21477 =( LENGTH_UNIT ( ) NAMED_UNIT ( * ) SI_UNIT ( .MILLI., .METRE. ) );
#21478 = ORIENTED_EDGE ( 'NONE', *, *, #16438, .T. ) ;
#21479 = AXIS2_PLACEMENT_3D ( 'NONE', #30039, #27086, #18191 ) ;
#21480 = LINE ( 'NONE', #9488, #13679 ) ;
#21481 = CARTESIAN_POINT ( 'NONE',  ( -8.647361814388510481, -14.68561526379591164, 7.652108011868850035 ) ) ;
#21482 = ORIENTED_EDGE ( 'NONE', *, *, #23869, .F. ) ;
#21483 = CARTESIAN_POINT ( 'NONE',  ( 18.41347767057966678, -7.852385608265396222, 18.35718225375110180 ) ) ;
#21484 = CARTESIAN_POINT ( 'NONE',  ( -15.97539537256530195, 12.03273630363204205, 19.48477075383299706 ) ) ;
#21485 = DIRECTION ( 'NONE',  ( 0.9975640502598243087, 0.000000000000000000, 0.06975647374412531632 ) ) ;
#21486 = EDGE_LOOP ( 'NONE', ( #12914, #19515, #30026, #9718 ) ) ;
#21487 = CARTESIAN_POINT ( 'NONE',  ( 15.39831020856429866, -7.255125275858175904, 19.08155846658118904 ) ) ;
#21488 = ORIENTED_EDGE ( 'NONE', *, *, #24067, .T. ) ;
#21489 = AXIS2_PLACEMENT_3D ( 'NONE', #14170, #7009, #16519 ) ;
#21490 = EDGE_LOOP ( 'NONE', ( #13682, #16633 ) ) ;
#21491 = DIRECTION ( 'NONE',  ( -0.000000000000000000, -0.000000000000000000, -1.000000000000000000 ) ) ;
#21492 = CARTESIAN_POINT ( 'NONE',  ( 27.03074382657074537, 6.449748410230989215, 42.96778633356034760 ) ) ;
#21494 = EDGE_CURVE ( 'NONE', #699, #2118, #13389, .T. ) ;
#21493 = VECTOR ( 'NONE', #20988, 1000.000000000000000 ) ;
#21495 = CARTESIAN_POINT ( 'NONE',  ( -8.079801766074020009, -15.02755831366980566, 18.50655187082627862 ) ) ;
#21496 = DIRECTION ( 'NONE',  ( 0.000000000000000000, 0.000000000000000000, 1.000000000000000000 ) ) ;
#21497 = CARTESIAN_POINT ( 'NONE',  ( -23.07950435457351190, 11.50806656539842798, 49.21048435262080289 ) ) ;
#21498 = CARTESIAN_POINT ( 'NONE',  ( -24.03057240117690441, -26.57182937991348481, 26.54355021145562787 ) ) ;
#21499 = EDGE_LOOP ( 'NONE', ( #5370, #27031 ) ) ;
#21500 = CARTESIAN_POINT ( 'NONE',  ( -16.81500952837178531, 2.642855143025228504, 19.22654678686458141 ) ) ;
#21501 = DIRECTION ( 'NONE',  ( 0.000000000000000000, 0.000000000000000000, -1.000000000000000000 ) ) ;
#21502 = DIRECTION ( 'NONE',  ( 0.000000000000000000, 0.000000000000000000, 1.000000000000000000 ) ) ;
#21503 = ORIENTED_EDGE ( 'NONE', *, *, #20457, .T. ) ;
#21504 = VERTEX_POINT ( 'NONE', #15871 ) ;
#21505 = CARTESIAN_POINT ( 'NONE',  ( -77.99999999999998579, -42.49999999999998579, 24.50000000000000000 ) ) ;
#21506 = LINE ( 'NONE', #148, #6648 ) ;
#21507 = VECTOR ( 'NONE', #28578, 1000.000000000000000 ) ;
#21508 = CARTESIAN_POINT ( 'NONE',  ( -39.87350638640939593, 4.706224724266459880, -6.500000000000000888 ) ) ;
#21509 = CARTESIAN_POINT ( 'NONE',  ( 6.187077094091595342, 11.47693674426096599, 24.50000000000000000 ) ) ;
#21510 = CARTESIAN_POINT ( 'NONE',  ( -15.49859937938256138, -7.047316568033163087, 7.267659094423556176 ) ) ;
#21511 = CARTESIAN_POINT ( 'NONE',  ( 64.99999999999998579, -70.00000000000000000, 12.49999999999999112 ) ) ;
#21512 = CARTESIAN_POINT ( 'NONE',  ( 2.168404344971008868E-16, 30.50000000000000000, 24.50000000000000000 ) ) ;
#21513 = ORIENTED_EDGE ( 'NONE', *, *, #9431, .F. ) ;
#21514 = AXIS2_PLACEMENT_3D ( 'NONE', #13629, #22814, #1753 ) ;
#21515 = LINE ( 'NONE', #9521, #20710 ) ;
#21516 = FACE_OUTER_BOUND ( 'NONE', #12617, .T. ) ;
#21517 = EDGE_CURVE ( 'NONE', #10764, #1242, #13543, .T. ) ;
#21518 = DIRECTION ( 'NONE',  ( -1.000000000000000000, 0.000000000000000000, 0.000000000000000000 ) ) ;
#21519 = ORIENTED_EDGE ( 'NONE', *, *, #13464, .T. ) ;
#21520 = CARTESIAN_POINT ( 'NONE',  ( 12.91703683527121704, 11.08965543756653460, 6.111214848085761986 ) ) ;
#21521 = EDGE_LOOP ( 'NONE', ( #14968, #21395, #28423, #18972 ) ) ;
#21522 = CARTESIAN_POINT ( 'NONE',  ( -4.163336342344337027E-14, 1.387778780781445676E-14, 24.50000000000000000 ) ) ;
#21523 = CARTESIAN_POINT ( 'NONE',  ( -33.35889463998628912, 23.76060433659045046, -9.833271769321862976 ) ) ;
#21524 = CARTESIAN_POINT ( 'NONE',  ( 39.99999999999996447, 90.00000000000001421, 59.49999999999999289 ) ) ;
#21525 = EDGE_CURVE ( 'NONE', #28674, #23884, #25069, .T. ) ;
#21526 = ORIENTED_EDGE ( 'NONE', *, *, #18387, .T. ) ;
#21527 = CARTESIAN_POINT ( 'NONE',  ( 35.98550141493651466, 1.281847341532557083, 27.50000000000000355 ) ) ;
#21528 = CIRCLE ( 'NONE', #8110, 9.482273699623480212 ) ;
#21529 = AXIS2_PLACEMENT_3D ( 'NONE', #10006, #26537, #21684 ) ;
#21530 = DIRECTION ( 'NONE',  ( -0.000000000000000000, -0.000000000000000000, -1.000000000000000000 ) ) ;
#21531 = EDGE_CURVE ( 'NONE', #24029, #1292, #6655, .T. ) ;
#21532 = VECTOR ( 'NONE', #9597, 1000.000000000000114 ) ;
#21533 = CARTESIAN_POINT ( 'NONE',  ( -32.98805937973593672, 22.67054169308932288, 8.000000000000003553 ) ) ;
#21534 = CARTESIAN_POINT ( 'NONE',  ( 33.03678844028523542, -25.60268484000898681, -16.50000000000000000 ) ) ;
#21535 = DIRECTION ( 'NONE',  ( -0.000000000000000000, 1.132880637372608986E-16, -1.000000000000000000 ) ) ;
#21536 = CARTESIAN_POINT ( 'NONE',  ( -31.46108752401733000, 15.19043599309334525, 40.06382167427029373 ) ) ;
#21537 = ORIENTED_EDGE ( 'NONE', *, *, #3065, .F. ) ;
#21538 = DIRECTION ( 'NONE',  ( -0.000000000000000000, -0.000000000000000000, -1.000000000000000000 ) ) ;
#21539 = ADVANCED_FACE ( 'NONE', ( #14599 ), #19276, .F. ) ;
#21540 = CARTESIAN_POINT ( 'NONE',  ( 10.11202017158463917, -41.14070756921186955, -1.500000000000000000 ) ) ;
#21541 = DIRECTION ( 'NONE',  ( 0.000000000000000000, -1.000000000000000000, 0.000000000000000000 ) ) ;
#21542 = VERTEX_POINT ( 'NONE', #7434 ) ;
#21543 = CYLINDRICAL_SURFACE ( 'NONE', #8090, 1.000000000000008438 ) ;
#21544 = EDGE_CURVE ( 'NONE', #19329, #1203, #16915, .T. ) ;
#21545 = CARTESIAN_POINT ( 'NONE',  ( -14.36006998371493637, -17.26937953831884442, 1.500000000000000000 ) ) ;
#21546 = LINE ( 'NONE', #12362, #19214 ) ;
#21547 = CARTESIAN_POINT ( 'NONE',  ( 4.894722408976176276, 16.30505022501959900, 7.156916968540298463 ) ) ;
#21548 = CARTESIAN_POINT ( 'NONE',  ( 19.64114023396309960, -37.13592150529014191, -1.500000000000000000 ) ) ;
#21549 = EDGE_LOOP ( 'NONE', ( #27612, #30834, #8963, #7508 ) ) ;
#21550 = CARTESIAN_POINT ( 'NONE',  ( -11.82521593960875528, 5.400395169024524655, 24.50000000000000000 ) ) ;
#21551 = CIRCLE ( 'NONE', #14090, 1.000000000000008660 ) ;
#21552 = CARTESIAN_POINT ( 'NONE',  ( 37.36871377735028688, -3.393397791468933278, 37.50000000003174705 ) ) ;
#21554 = CIRCLE ( 'NONE', #8132, 0.7500000000000006661 ) ;
#21553 = DIRECTION ( 'NONE',  ( -0.000000000000000000, -0.000000000000000000, -1.000000000000000000 ) ) ;
#21555 = ORIENTED_EDGE ( 'NONE', *, *, #16744, .T. ) ;
#21556 = DIRECTION ( 'NONE',  ( 0.000000000000000000, -1.000000000000000000, 1.669238443041286689E-16 ) ) ;
#21557 = EDGE_LOOP ( 'NONE', ( #27479, #2638, #16970, #2874 ) ) ;
#21558 = CARTESIAN_POINT ( 'NONE',  ( 15.41296542101254552, 5.939519782021115191, 24.50000000000000000 ) ) ;
#21559 = DIRECTION ( 'NONE',  ( -0.000000000000000000, -0.000000000000000000, -1.000000000000000000 ) ) ;
#21560 = ORIENTED_EDGE ( 'NONE', *, *, #28037, .T. ) ;
#21561 = EDGE_CURVE ( 'NONE', #1314, #21169, #6389, .T. ) ;
#21562 = AXIS2_PLACEMENT_3D ( 'NONE', #18020, #27531, #23738 ) ;
#21563 = ORIENTED_EDGE ( 'NONE', *, *, #13948, .T. ) ;
#21564 = ADVANCED_FACE ( 'NONE', ( #9467 ), #21767, .T. ) ;
#21565 = DIRECTION ( 'NONE',  ( 1.000000000000000000, 0.000000000000000000, 0.000000000000000000 ) ) ;
#21566 = ORIENTED_EDGE ( 'NONE', *, *, #16891, .T. ) ;
#21567 = EDGE_LOOP ( 'NONE', ( #177, #16987, #17162, #2341 ) ) ;
#21568 = ORIENTED_EDGE ( 'NONE', *, *, #12580, .T. ) ;
#21569 = CARTESIAN_POINT ( 'NONE',  ( 0.3440795696225442679, -17.03036400190298139, 18.44501272782439827 ) ) ;
#21570 = EDGE_CURVE ( 'NONE', #20802, #29075, #406, .T. ) ;
#21571 = CARTESIAN_POINT ( 'NONE',  ( -9.661386603328285361, -17.53179420831165558, 6.447548852708279377 ) ) ;
#21572 = AXIS2_PLACEMENT_3D ( 'NONE', #24387, #3031, #680 ) ;
#21573 = CARTESIAN_POINT ( 'NONE',  ( 5.016036949087476771, 16.26541432804313914, 19.41069149716887310 ) ) ;
#21574 = CARTESIAN_POINT ( 'NONE',  ( 0.9359619706472936951, -17.02419289499718147, 18.35718225375110180 ) ) ;
#21575 = EDGE_LOOP ( 'NONE', ( #277, #23370, #8666, #9354, #21279, #312, #9329, #22928, #1093, #22157, #10089, #23281, #21583, #5269, #19884, #6546, #30838, #11682, #29957, #9205, #9305, #11053, #9893, #11537, #1211, #7491, #12724, #14927, #9783, #11977, #9708, #5478, #12380, #5433, #10887, #8366, #11406, #1935, #10331, #28833, #5161, #9471, #8501, #24801, #28787, #17509, #6731, #30195, #10334, #19195, #6928, #12066, #6100, #21978, #10880, #24848, #27461, #23192, #17200, #9495, #24862, #2289, #14267, #12098, #11665, #20342, #3731, #16821, #5703, #25719, #18152, #10215, #2077, #27853, #23077, #6240, #11760 ) ) ;
#21576 = EDGE_CURVE ( 'NONE', #19220, #14452, #5039, .T. ) ;
#21577 = CARTESIAN_POINT ( 'NONE',  ( 18.53505294460179798, -7.514422089582853737, 5.779535427900761135 ) ) ;
#21578 = AXIS2_PLACEMENT_3D ( 'NONE', #2295, #18546, #28046 ) ;
#21579 = DIRECTION ( 'NONE',  ( 1.000000000000000000, 0.000000000000000000, 0.000000000000000000 ) ) ;
#21580 = CARTESIAN_POINT ( 'NONE',  ( 1.236176367852860780, -19.96182836857062171, 19.85730954408918336 ) ) ;
#21581 = CARTESIAN_POINT ( 'NONE',  ( 34.99999999999933920, 4.286263797015655244E-15, 92.49999999999998579 ) ) ;
#21582 = EDGE_CURVE ( 'NONE', #3169, #15101, #24297, .T. ) ;
#21583 = ORIENTED_EDGE ( 'NONE', *, *, #1556, .T. ) ;
#21584 = B_SPLINE_CURVE_WITH_KNOTS ( 'NONE', 3,
 ( #14185, #25454, #23087, #1732, #16085, #25604, #4221, #5463, #24477, #2501, #14964, #12170, #21668, #151, #9988, #760 ),
 .UNSPECIFIED., .F., .F.,
 ( 4, 2, 2, 2, 2, 2, 2, 4 ),
 ( 0.4999999999999994449, 0.6249999999999996669, 0.6874999999999997780, 0.7187499999999995559, 0.7499999999999994449, 0.8124999999999995559, 0.8749999999999997780, 1.000000000000000000 ),
 .UNSPECIFIED. ) ;
#21585 = AXIS2_PLACEMENT_3D ( 'NONE', #10792, #13460, #8304 ) ;
#21586 = DIRECTION ( 'NONE',  ( 1.000000000000000000, 0.000000000000000000, 0.000000000000000000 ) ) ;
#21587 = LINE ( 'NONE', #19101, #22238 ) ;
#21588 = CARTESIAN_POINT ( 'NONE',  ( -6.878634932266923130, 18.79866186728735400, 6.995624166085161910 ) ) ;
#21589 = DIRECTION ( 'NONE',  ( 1.000000000000000000, 0.000000000000000000, 0.000000000000000000 ) ) ;
#21590 = CARTESIAN_POINT ( 'NONE',  ( 1.010086789600752760E-15, 0.4400770685579618036, 9.000000000000001776 ) ) ;
#21591 = DIRECTION ( 'NONE',  ( -0.6707505147970012072, 0.7416830501633145944, 0.000000000000000000 ) ) ;
#21592 = CARTESIAN_POINT ( 'NONE',  ( 2.552544030762014415, -42.50000000000000000, -1.500000000000000000 ) ) ;
#21593 = ORIENTED_EDGE ( 'NONE', *, *, #30132, .T. ) ;
#21594 = ORIENTED_EDGE ( 'NONE', *, *, #8039, .T. ) ;
#21595 = FILL_AREA_STYLE ('',( #19256 ) ) ;
#21596 = CARTESIAN_POINT ( 'NONE',  ( -5.846240454020372290, 19.12690956503887918, 20.34789198813115618 ) ) ;
#21597 = CARTESIAN_POINT ( 'NONE',  ( -8.860628911697515875, 8.184276679720483116, 1.500000000000000000 ) ) ;
#21598 = CARTESIAN_POINT ( 'NONE',  ( 11.53007546964076191, -16.34234030559854034, 18.47531940416306639 ) ) ;
#21599 = ORIENTED_EDGE ( 'NONE', *, *, #11278, .F. ) ;
#21600 = APPLICATION_PROTOCOL_DEFINITION ( 'draft international standard', 'automotive_design', 1998, #4016 ) ;
#21601 = CARTESIAN_POINT ( 'NONE',  ( 15.59193442375634753, -6.853442328767824776, 18.49267272388512140 ) ) ;
#21602 = CARTESIAN_POINT ( 'NONE',  ( 4.806943871629680842, 16.33324523791883109, 6.018569869498933578 ) ) ;
#21603 = EDGE_CURVE ( 'NONE', #4914, #7455, #4624, .T. ) ;
#21604 = EDGE_LOOP ( 'NONE', ( #20377, #5612 ) ) ;
#21605 = B_SPLINE_CURVE_WITH_KNOTS ( 'NONE', 3,
 ( #11638, #4762, #30502, #9147, #30649, #2440, #21452, #546, #10068, #401 ),
 .UNSPECIFIED., .F., .F.,
 ( 4, 3, 3, 4 ),
 ( 2.017013542443209820E-16, 0.005033946524314806929, 0.01006789357361620452, 0.01510156516372195695 ),
 .UNSPECIFIED. ) ;
#21606 = VECTOR ( 'NONE', #19720, 1000.000000000000000 ) ;
#21607 = AXIS2_PLACEMENT_3D ( 'NONE', #9687, #6889, #4546 ) ;
#21608 = EDGE_CURVE ( 'NONE', #29972, #20277, #7122, .T. ) ;
#21609 = CARTESIAN_POINT ( 'NONE',  ( 12.35846532919129004, 11.73919094318043932, 7.652108011868850035 ) ) ;
#21610 = CARTESIAN_POINT ( 'NONE',  ( -19.82881186446047295, -38.45831515674161949, -16.50000000000000355 ) ) ;
#21611 = EDGE_CURVE ( 'NONE', #5849, #21196, #7365, .T. ) ;
#21612 = CARTESIAN_POINT ( 'NONE',  ( -38.41462058491280374, 7.368026156770138613, 35.01883456753041912 ) ) ;
#21613 = VERTEX_POINT ( 'NONE', #26297 ) ;
#21614 = CARTESIAN_POINT ( 'NONE',  ( 0.000000000000000000, 1.699320956058915452E-16, -1.500000000000001776 ) ) ;
#21615 = EDGE_CURVE ( 'NONE', #23454, #28205, #13360, .T. ) ;
#21616 = DIRECTION ( 'NONE',  ( 0.000000000000000000, 0.000000000000000000, 1.000000000000000000 ) ) ;
#21617 = CARTESIAN_POINT ( 'NONE',  ( -5.815855718377446415, -16.25752007041490188, 24.50000000000000000 ) ) ;
#21618 = ORIENTED_EDGE ( 'NONE', *, *, #26310, .F. ) ;
#21619 = CARTESIAN_POINT ( 'NONE',  ( -18.24831633358132521, -8.229495485092101603, 7.557577766377196582 ) ) ;
#21620 = CYLINDRICAL_SURFACE ( 'NONE', #14845, 0.7500000000000006661 ) ;
#21621 = CARTESIAN_POINT ( 'NONE',  ( 7.869584159753955532, 10.39565510934977333, 1.500000000000001332 ) ) ;
#21622 = PRODUCT_DEFINITION_SHAPE ( 'NONE', 'NONE',  #30859 ) ;
#21623 = CARTESIAN_POINT ( 'NONE',  ( -0.3606176111512335858, -20.01462698034515597, 5.940635272151477686 ) ) ;
#21624 = DIRECTION ( 'NONE',  ( 1.000000000000000000, 0.000000000000000000, 0.000000000000000000 ) ) ;
#21625 = CARTESIAN_POINT ( 'NONE',  ( -13.83213539500865785, 7.758783772730382111, 1.500000000000000000 ) ) ;
#21626 = VECTOR ( 'NONE', #26994, 1000.000000000000000 ) ;
#21627 = CARTESIAN_POINT ( 'NONE',  ( 37.98873790226522118, -9.615455971224255549, 13.00203930632523353 ) ) ;
#21628 = FACE_OUTER_BOUND ( 'NONE', #3404, .T. ) ;
#21629 = ORIENTED_EDGE ( 'NONE', *, *, #27155, .T. ) ;
#21630 = LINE ( 'NONE', #3223, #29693 ) ;
#21631 = DIRECTION ( 'NONE',  ( -0.9594929736144975907, 0.2817325568414293380, 0.000000000000000000 ) ) ;
#21632 = ORIENTED_EDGE ( 'NONE', *, *, #30561, .T. ) ;
#21633 = ORIENTED_EDGE ( 'NONE', *, *, #4183, .F. ) ;
#21634 = CARTESIAN_POINT ( 'NONE',  ( 4.690519134554619107, 19.44242338873975484, 18.54958172136248251 ) ) ;
#21635 = EDGE_CURVE ( 'NONE', #11117, #22736, #2446, .T. ) ;
#21636 = DIRECTION ( 'NONE',  ( 1.982541115402065110E-16, 0.000000000000000000, -1.000000000000000000 ) ) ;
#21637 = SHAPE_REPRESENTATION_RELATIONSHIP ( 'NONE' , 'NONE' ,  #28257, #30671 ) ;
#21638 = VERTEX_POINT ( 'NONE', #550 ) ;
#21639 = EDGE_CURVE ( 'NONE', #24660, #4417, #15317, .T. ) ;
#21640 = DIRECTION ( 'NONE',  ( 0.000000000000000000, 1.000000000000000000, -1.669238443041286689E-16 ) ) ;
#21641 = DIRECTION ( 'NONE',  ( 0.000000000000000000, -0.000000000000000000, -1.000000000000000000 ) ) ;
#21642 = ORIENTED_EDGE ( 'NONE', *, *, #7314, .T. ) ;
#21643 = CARTESIAN_POINT ( 'NONE',  ( 18.67779315278252739, -7.200759110456479206, 19.89182036555910571 ) ) ;
#21644 = CARTESIAN_POINT ( 'NONE',  ( 16.56580381663017576, 4.144794415032112767, 19.03762469184452755 ) ) ;
#21645 = CARTESIAN_POINT ( 'NONE',  ( -25.23756106473024019, 11.43858098102958287, -1.500000000000000000 ) ) ;
#21646 = EDGE_LOOP ( 'NONE', ( #14291, #12749, #29258, #30045, #24505, #27170, #2227 ) ) ;
#21647 = CARTESIAN_POINT ( 'NONE',  ( 15.40878509682498709, -7.233835690006360508, 19.66962785902261146 ) ) ;
#21648 = VECTOR ( 'NONE', #21914, 1000.000000000000000 ) ;
#21649 = ORIENTED_EDGE ( 'NONE', *, *, #1006, .F. ) ;
#21650 = VERTEX_POINT ( 'NONE', #29102 ) ;
#21651 = CARTESIAN_POINT ( 'NONE',  ( 38.42058609394389634, 7.733997452150218166, 32.05199712042067262 ) ) ;
#21652 = CARTESIAN_POINT ( 'NONE',  ( -12.81275022540756581, 11.20978530020977182, 19.87181966307587544 ) ) ;
#21653 = CARTESIAN_POINT ( 'NONE',  ( -9.895604986052601859, -17.40083251127919794, 18.64703902303423178 ) ) ;
#21654 = CARTESIAN_POINT ( 'NONE',  ( -52.16608720827707657, 36.86186943028246787, 57.49999999999999289 ) ) ;
#21655 = CARTESIAN_POINT ( 'NONE',  ( -23.72845085825479217, 12.99428747377815618, 47.94653096642124268 ) ) ;
#21656 = CYLINDRICAL_SURFACE ( 'NONE', #30786, 12.50000000000000000 ) ;
#21657 = ORIENTED_EDGE ( 'NONE', *, *, #366, .T. ) ;
#21658 = CARTESIAN_POINT ( 'NONE',  ( 9.579384792474776589, -14.08793303971873101, 7.595116371587256054 ) ) ;
#21659 = DIRECTION ( 'NONE',  ( 0.000000000000000000, 1.000000000000000000, 0.000000000000000000 ) ) ;
#21660 = DIRECTION ( 'NONE',  ( -1.000000000000000000, 0.000000000000000000, 0.000000000000000000 ) ) ;
#21661 = LINE ( 'NONE', #4984, #5842 ) ;
#21662 = EDGE_LOOP ( 'NONE', ( #26917, #3125, #20117, #7188 ) ) ;
#21663 = EDGE_LOOP ( 'NONE', ( #24034, #19403, #9132, #23328 ) ) ;
#21664 = PLANE ( 'NONE',  #25266 ) ;
#21665 = DIRECTION ( 'NONE',  ( 0.000000000000000000, 0.000000000000000000, 1.000000000000000000 ) ) ;
#21666 = LINE ( 'NONE', #149, #21294 ) ;
#21667 = CARTESIAN_POINT ( 'NONE',  ( -5.754904482333548899, 19.17304367822654854, 7.632642797338977658 ) ) ;
#21668 = CARTESIAN_POINT ( 'NONE',  ( 11.80522207451355143, 12.33118449395948169, 7.269896094239230777 ) ) ;
#21669 = ADVANCED_FACE ( 'NONE', ( #25997 ), #23629, .F. ) ;
#21670 = CARTESIAN_POINT ( 'NONE',  ( -25.48568755041063838, -12.36160011285428517, 1.500000000000001332 ) ) ;
#21671 = ORIENTED_EDGE ( 'NONE', *, *, #7117, .F. ) ;
#21672 = ORIENTED_EDGE ( 'NONE', *, *, #17580, .T. ) ;
#21673 = CARTESIAN_POINT ( 'NONE',  ( -32.02759086605583150, -18.14861398546997862, 34.50000000000000000 ) ) ;
#21674 = DIRECTION ( 'NONE',  ( 0.000000000000000000, 0.000000000000000000, 1.000000000000000000 ) ) ;
#21675 = EDGE_LOOP ( 'NONE', ( #12042, #28637, #18861, #15002 ) ) ;
#21676 = DIRECTION ( 'NONE',  ( 0.2972711322815261292, 0.9547931052914340189, 0.000000000000000000 ) ) ;
#21677 = ORIENTED_EDGE ( 'NONE', *, *, #2381, .T. ) ;
#21678 = DIRECTION ( 'NONE',  ( -0.000000000000000000, -0.000000000000000000, -1.000000000000000000 ) ) ;
#21679 = CARTESIAN_POINT ( 'NONE',  ( 16.59792644102986614, 3.991267607033987197, 19.96568007040468729 ) ) ;
#21680 = CARTESIAN_POINT ( 'NONE',  ( 4.510281037539698445E-13, -4.926614671774132148E-13, 82.49999999999998579 ) ) ;
#21681 = ORIENTED_EDGE ( 'NONE', *, *, #22660, .F. ) ;
#21682 = VECTOR ( 'NONE', #8148, 1000.000000000000000 ) ;
#21683 = FACE_OUTER_BOUND ( 'NONE', #21549, .T. ) ;
#21684 = DIRECTION ( 'NONE',  ( 0.6707505147970089787, 0.7416830501633076000, 0.000000000000000000 ) ) ;
#21685 = CARTESIAN_POINT ( 'NONE',  ( 24.03057240117690441, -26.57182937991349903, 24.50000000000000000 ) ) ;
#21686 = CARTESIAN_POINT ( 'NONE',  ( -18.25569084301828582, -8.169747224523369766, 5.775318986477950389 ) ) ;
#21687 = DIRECTION ( 'NONE',  ( -1.000000000000000000, 0.000000000000000000, 0.000000000000000000 ) ) ;
#21688 = FACE_OUTER_BOUND ( 'NONE', #6880, .T. ) ;
#21689 = FACE_OUTER_BOUND ( 'NONE', #16259, .T. ) ;
#21690 = ORIENTED_EDGE ( 'NONE', *, *, #8427, .T. ) ;
#21691 = DIRECTION ( 'NONE',  ( -0.000000000000000000, 0.000000000000000000, 1.000000000000000000 ) ) ;
#21692 = CARTESIAN_POINT ( 'NONE',  ( -39.00000000000000000, -5.563236990218529243, -1.500000000000000000 ) ) ;
#21693 = AXIS2_PLACEMENT_3D ( 'NONE', #30478, #16297, #2090 ) ;
#21694 = CARTESIAN_POINT ( 'NONE',  ( 7.500000000000000000, 5.196152422706624030, 9.000000000000001776 ) ) ;
#21695 = ORIENTED_EDGE ( 'NONE', *, *, #29443, .T. ) ;
#21696 = DIRECTION ( 'NONE',  ( 1.000000000000000000, 0.000000000000000000, 0.000000000000000000 ) ) ;
#21697 = CARTESIAN_POINT ( 'NONE',  ( -17.86647173498021957, -9.028149653223259463, 20.25542030744407640 ) ) ;
#21698 = LINE ( 'NONE', #26401, #5267 ) ;
#21699 = CARTESIAN_POINT ( 'NONE',  ( -14.83584055149731817, -17.84153987719691514, -1.500000000000000000 ) ) ;
#21700 = CARTESIAN_POINT ( 'NONE',  ( 10.11202017158463917, -41.14070756921186955, -1.500000000000000000 ) ) ;
#21701 = DIRECTION ( 'NONE',  ( 0.000000000000000000, 1.000000000000000000, 0.000000000000000000 ) ) ;
#21702 = VECTOR ( 'NONE', #2641, 1000.000000000000000 ) ;
#21703 = CARTESIAN_POINT ( 'NONE',  ( 30.06732515731210142, 27.07630587620099050, 30.35442667510426062 ) ) ;
#21704 = EDGE_CURVE ( 'NONE', #9483, #14021, #16634, .T. ) ;
#21705 = CARTESIAN_POINT ( 'NONE',  ( 19.59831178344207814, 3.989367808977725804, 7.272192800924339728 ) ) ;
#21706 = ORIENTED_EDGE ( 'NONE', *, *, #14163, .T. ) ;
#21707 = AXIS2_PLACEMENT_3D ( 'NONE', #1412, #29798, #3126 ) ;
#21708 = CARTESIAN_POINT ( 'NONE',  ( -40.00000000000000000, 90.00000000000001421, 22.49999999999999289 ) ) ;
#21709 = EDGE_LOOP ( 'NONE', ( #13841, #9524, #29988, #22407 ) ) ;
#21710 = CARTESIAN_POINT ( 'NONE',  ( 32.28307784207223108, -8.475829241206289666, 37.38016955275583086 ) ) ;
#21711 = CARTESIAN_POINT ( 'NONE',  ( -18.58529988941444699, 7.388276390372320535, 1.500000000000001332 ) ) ;
#21712 = ORIENTED_EDGE ( 'NONE', *, *, #12246, .F. ) ;
#21713 = VERTEX_POINT ( 'NONE', #22677 ) ;
#21714 = CARTESIAN_POINT ( 'NONE',  ( 9.062880100047298271, 0.6210184355499750453, -1.500000000000001776 ) ) ;
#21715 = EDGE_LOOP ( 'NONE', ( #25616, #29646, #12960, #12374 ) ) ;
#21716 = CIRCLE ( 'NONE', #8295, 3.000000000000002665 ) ;
#21717 = VERTEX_POINT ( 'NONE', #3359 ) ;
#21718 = ORIENTED_EDGE ( 'NONE', *, *, #1909, .T. ) ;
#21719 = CARTESIAN_POINT ( 'NONE',  ( -0.2311899301088675418, -17.01971842090038223, 19.45164628100866722 ) ) ;
#21720 = VECTOR ( 'NONE', #25132, 999.9999999999998863 ) ;
#21721 = CARTESIAN_POINT ( 'NONE',  ( -17.79341399750137498, 34.33949722786772440, 34.50000000000000000 ) ) ;
#21722 = CARTESIAN_POINT ( 'NONE',  ( -7.673856334772120924, -15.25703464229374617, 6.782048567692550378 ) ) ;
#21723 = DIRECTION ( 'NONE',  ( 0.000000000000000000, 1.000000000000000000, 1.193512090021232842E-16 ) ) ;
#21724 = CARTESIAN_POINT ( 'NONE',  ( 1.780236034000290957, -16.98472935612791801, 19.14333282897057842 ) ) ;
#21725 = VERTEX_POINT ( 'NONE', #12892 ) ;
#21726 = CARTESIAN_POINT ( 'NONE',  ( 7.500000000000000000, 0.000000000000000000, 9.000000000000000000 ) ) ;
#21727 = CARTESIAN_POINT ( 'NONE',  ( -23.13391957319673864, -11.02874123662317984, 45.12930086386443662 ) ) ;
#21728 = CARTESIAN_POINT ( 'NONE',  ( 5.204170427930421283E-15, -44.07656352898514740, -16.50000000000000000 ) ) ;
#21729 = CARTESIAN_POINT ( 'NONE',  ( 14.39714448835433025, 13.90806243540158071, 18.64703902303423178 ) ) ;
#21730 = DIRECTION ( 'NONE',  ( 0.000000000000000000, 0.000000000000000000, -1.000000000000000000 ) ) ;
#21731 = VERTEX_POINT ( 'NONE', #12579 ) ;
#21732 = CIRCLE ( 'NONE', #3826, 0.7499999999999997780 ) ;
#21733 = AXIS2_PLACEMENT_3D ( 'NONE', #3631, #13150, #1293 ) ;
#21734 = DIRECTION ( 'NONE',  ( 0.000000000000000000, 1.000000000000000000, 0.000000000000000000 ) ) ;
#21735 = CARTESIAN_POINT ( 'NONE',  ( -15.16307466679259264, -7.786257835066841437, 5.652196082364323360 ) ) ;
#21736 = CARTESIAN_POINT ( 'NONE',  ( -6.051176437752240567, 19.08139585423913331, 5.652605728828373977 ) ) ;
#21737 = DIRECTION ( 'NONE',  ( 0.000000000000000000, 0.000000000000000000, 1.000000000000000000 ) ) ;
#21738 = CARTESIAN_POINT ( 'NONE',  ( 0.5612050131688001153, 4.355613924421556149, 9.000000000000001776 ) ) ;
#21739 = ADVANCED_FACE ( 'NONE', ( #24414 ), #27221, .F. ) ;
#21740 = ADVANCED_FACE ( 'NONE', ( #24564 ), #12730, .F. ) ;
#21741 = CARTESIAN_POINT ( 'NONE',  ( -15.21221250122201596, -7.682808169219079275, 18.35377592296120497 ) ) ;
#21742 = CYLINDRICAL_SURFACE ( 'NONE', #19071, 20.00000000000000000 ) ;
#21743 = VECTOR ( 'NONE', #9696, 1000.000000000000000 ) ;
#21744 = EDGE_LOOP ( 'NONE', ( #12744, #982, #3999, #27713 ) ) ;
#21745 = ORIENTED_EDGE ( 'NONE', *, *, #3267, .F. ) ;
#21746 = DIRECTION ( 'NONE',  ( -1.000000000000000000, 0.000000000000000000, 0.000000000000000000 ) ) ;
#21747 = COLOUR_RGB ( '',0.7921568627450980005, 0.8196078431372548767, 0.9333333333333333481 ) ;
#21748 = EDGE_CURVE ( 'NONE', #14669, #10421, #19823, .T. ) ;
#21749 = LINE ( 'NONE', #5075, #23337 ) ;
#21750 = EDGE_CURVE ( 'NONE', #18090, #24218, #14907, .T. ) ;
#21751 = LINE ( 'NONE', #19422, #17562 ) ;
#21752 = EDGE_LOOP ( 'NONE', ( #9599, #27104, #8640, #29169 ) ) ;
#21753 = CARTESIAN_POINT ( 'NONE',  ( 4.510281037539698445E-13, -4.926614671774132148E-13, 82.49999999999998579 ) ) ;
#21754 = CIRCLE ( 'NONE', #22266, 0.7441270634456955690 ) ;
#21755 = CARTESIAN_POINT ( 'NONE',  ( 5.298970182598332634, 19.30368537022594211, 5.652196082367002106 ) ) ;
#21756 = CIRCLE ( 'NONE', #10317, 20.00000000000000000 ) ;
#21757 = EDGE_CURVE ( 'NONE', #15951, #16368, #901, .T. ) ;
#21758 = ORIENTED_EDGE ( 'NONE', *, *, #5428, .F. ) ;
#21759 = CARTESIAN_POINT ( 'NONE',  ( 6.247918173525853547, 19.01788707503811438, 19.56050940960062690 ) ) ;
#21760 = AXIS2_PLACEMENT_3D ( 'NONE', #29187, #27017, #20138 ) ;
#21761 = FACE_OUTER_BOUND ( 'NONE', #7345, .T. ) ;
#21762 = VECTOR ( 'NONE', #28280, 1000.000000000000000 ) ;
#21763 = EDGE_CURVE ( 'NONE', #9004, #7775, #17703, .T. ) ;
#21764 = CARTESIAN_POINT ( 'NONE',  ( 0.000000000000000000, -7.794228634059943595, 4.500000000000005329 ) ) ;
#21765 = CARTESIAN_POINT ( 'NONE',  ( -30.15176711667785980, -27.09037013813884798, 30.35400163365964943 ) ) ;
#21766 = EDGE_LOOP ( 'NONE', ( #2107, #141, #19261, #26420 ) ) ;
#21767 = CYLINDRICAL_SURFACE ( 'NONE', #6857, 27.70876437800068359 ) ;
#21768 = EDGE_CURVE ( 'NONE', #6600, #27382, #21822, .T. ) ;
#21769 = DIRECTION ( 'NONE',  ( -0.000000000000000000, -0.000000000000000000, -1.000000000000000000 ) ) ;
#21770 = DIRECTION ( 'NONE',  ( 1.000000000000000000, 0.000000000000000000, -0.000000000000000000 ) ) ;
#21771 = VECTOR ( 'NONE', #18879, 1000.000000000000000 ) ;
#21772 = VERTEX_POINT ( 'NONE', #3056 ) ;
#21773 = CARTESIAN_POINT ( 'NONE',  ( -18.47553274370955734, -7.705290464775616854, 6.641371103590088865 ) ) ;
#21774 = CARTESIAN_POINT ( 'NONE',  ( 14.70074466696774174, 13.56107787884953986, 5.679672709359371297 ) ) ;
#21775 = AXIS2_PLACEMENT_3D ( 'NONE', #13278, #25117, #3757 ) ;
#21776 = CARTESIAN_POINT ( 'NONE',  ( -0.6524377400371697000, -20.00727110999512348, 6.530762810602277924 ) ) ;
#21777 = VECTOR ( 'NONE', #6584, 1000.000000000000000 ) ;
#21778 = DIRECTION ( 'NONE',  ( 1.000000000000000000, 0.000000000000000000, 0.000000000000000000 ) ) ;
#21779 = AXIS2_PLACEMENT_3D ( 'NONE', #10853, #25182, #29263 ) ;
#21780 = CARTESIAN_POINT ( 'NONE',  ( -39.00000000000000000, 46.58316968839002925, 16.34922658321931976 ) ) ;
#21781 = CARTESIAN_POINT ( 'NONE',  ( 37.81968897652127026, -10.37739785557808680, 14.29161961893967181 ) ) ;
#21782 = CARTESIAN_POINT ( 'NONE',  ( -14.41708049311053053, 17.22181377296911720, 1.500000000000000000 ) ) ;
#21783 = ORIENTED_EDGE ( 'NONE', *, *, #11577, .T. ) ;
#21784 = EDGE_CURVE ( 'NONE', #10643, #15912, #22227, .T. ) ;
#21785 = EDGE_CURVE ( 'NONE', #24252, #8036, #19847, .T. ) ;
#21786 = FACE_BOUND ( 'NONE', #25539, .T. ) ;
#21787 = CARTESIAN_POINT ( 'NONE',  ( 4.805983152666244429, 19.41435796516022450, 7.528076282304598799 ) ) ;
#21788 = ORIENTED_EDGE ( 'NONE', *, *, #28456, .F. ) ;
#21789 = ADVANCED_FACE ( 'NONE', ( #27391 ), #1028, .F. ) ;
#21790 = ORIENTED_EDGE ( 'NONE', *, *, #24422, .F. ) ;
#21791 = DIRECTION ( 'NONE',  ( -0.000000000000000000, -0.000000000000000000, 1.000000000000000000 ) ) ;
#21792 = AXIS2_PLACEMENT_3D ( 'NONE', #13985, #20984, #21297 ) ;
#21793 = CARTESIAN_POINT ( 'NONE',  ( -11.29794076498435551, 48.71192074315335674, -45.08525989437928416 ) ) ;
#21794 = ADVANCED_FACE ( 'NONE', ( #19732, #10850 ), #20044, .T. ) ;
#21795 = CIRCLE ( 'NONE', #14299, 21.71568325578193637 ) ;
#21796 = ORIENTED_EDGE ( 'NONE', *, *, #13249, .F. ) ;
#21797 = FACE_OUTER_BOUND ( 'NONE', #24879, .T. ) ;
#21798 = CARTESIAN_POINT ( 'NONE',  ( -9.396043825398766813, -14.19290753657280035, 6.755862304746362845 ) ) ;
#21799 = EDGE_CURVE ( 'NONE', #27449, #26398, #15360, .T. ) ;
#21800 = CARTESIAN_POINT ( 'NONE',  ( 16.08779849516155025, -5.700297231796346509, 20.06253562465620632 ) ) ;
#21801 = CARTESIAN_POINT ( 'NONE',  ( -15.95879822657219194, 12.05485308878816220, 19.61564845152808090 ) ) ;
#21802 = AXIS2_PLACEMENT_3D ( 'NONE', #735, #10253, #19767 ) ;
#21803 = CARTESIAN_POINT ( 'NONE',  ( -4.163336342344337027E-14, 1.387778780781445676E-14, 1.500000000000000000 ) ) ;
#21804 = ORIENTED_EDGE ( 'NONE', *, *, #17175, .T. ) ;
#21805 = VECTOR ( 'NONE', #5861, 1000.000000000000000 ) ;
#21806 = CARTESIAN_POINT ( 'NONE',  ( 15.55762523216159821, -6.926306048554701889, 18.54473042795395088 ) ) ;
#21807 = ORIENTED_EDGE ( 'NONE', *, *, #13563, .F. ) ;
#21808 = EDGE_CURVE ( 'NONE', #18935, #27782, #15527, .T. ) ;
#21809 = CARTESIAN_POINT ( 'NONE',  ( 31.76816150359531576, -26.51947378167971792, -11.49999299985452694 ) ) ;
#21810 = CARTESIAN_POINT ( 'NONE',  ( -6.914714884271994322, 18.78545221144173638, 19.58863275299554019 ) ) ;
#21811 = CARTESIAN_POINT ( 'NONE',  ( -13.16038179581985723, 10.81844819380990330, 20.29090034784956131 ) ) ;
#21812 = AXIS2_PLACEMENT_3D ( 'NONE', #2499, #28547, #19340 ) ;
#21813 = EDGE_CURVE ( 'NONE', #10182, #22039, #3985, .T. ) ;
#21814 = AXIS2_PLACEMENT_3D ( 'NONE', #2995, #19660, #29184 ) ;
#21815 = FACE_OUTER_BOUND ( 'NONE', #8928, .T. ) ;
#21816 = CARTESIAN_POINT ( 'NONE',  ( 24.35970437652574816, -13.37404834226503958, -16.55003854064094426 ) ) ;
#21817 = CARTESIAN_POINT ( 'NONE',  ( 1.000000000000008438, 13.00000000000001421, 24.50000000000000000 ) ) ;
#21818 = LINE ( 'NONE', #5450, #18367 ) ;
#21819 = ORIENTED_EDGE ( 'NONE', *, *, #15449, .F. ) ;
#21820 = CARTESIAN_POINT ( 'NONE',  ( 10.75049709165479861, -16.88611404641621405, 5.749228751562096562 ) ) ;
#21821 = CARTESIAN_POINT ( 'NONE',  ( -28.75875294368007928, 28.70714236740944258, 10.32584181054939165 ) ) ;
#21822 = CIRCLE ( 'NONE', #2414, 14.52510309069105965 ) ;
#21823 = CARTESIAN_POINT ( 'NONE',  ( -15.49619650379776559, 12.67194488555737131, 7.627891251804737927 ) ) ;
#21824 = CARTESIAN_POINT ( 'NONE',  ( -40.00000000000000000, 87.00000000000001421, 62.49999999999999289 ) ) ;
#21825 = ORIENTED_EDGE ( 'NONE', *, *, #11116, .F. ) ;
#21826 = ORIENTED_EDGE ( 'NONE', *, *, #14533, .T. ) ;
#21827 = DIRECTION ( 'NONE',  ( 1.000000000000000000, 0.000000000000000000, 0.000000000000000000 ) ) ;
#21828 = CARTESIAN_POINT ( 'NONE',  ( 13.00999358272542850, -0.8602714556717643291, 1.500000000000001332 ) ) ;
#21829 = DIRECTION ( 'NONE',  ( 1.000000000000000000, 0.000000000000000000, -0.000000000000000000 ) ) ;
#21830 = LINE ( 'NONE', #17306, #19607 ) ;
#21831 = CARTESIAN_POINT ( 'NONE',  ( 0.01885174614965991896, 0.8831628876357848767, -9.000000000000003553 ) ) ;
#21832 = CARTESIAN_POINT ( 'NONE',  ( -16.90598708042468701, 2.083096162940503593, 18.44501272782439827 ) ) ;
#21833 = ORIENTED_EDGE ( 'NONE', *, *, #21127, .F. ) ;
#21834 = CIRCLE ( 'NONE', #23329, 0.7500000000000006661 ) ;
#21835 = ORIENTED_EDGE ( 'NONE', *, *, #1210, .F. ) ;
#21836 = CARTESIAN_POINT ( 'NONE',  ( -4.375757216953428294E-15, -39.50000000000000000, 34.49999999999999289 ) ) ;
#21837 = AXIS2_PLACEMENT_3D ( 'NONE', #3070, #12593, #17104 ) ;
#21838 = LINE ( 'NONE', #9677, #18691 ) ;
#21839 = CIRCLE ( 'NONE', #8412, 5.000000000000004441 ) ;
#21840 = CYLINDRICAL_SURFACE ( 'NONE', #10473, 2.000000000000001776 ) ;
#21841 = VERTEX_POINT ( 'NONE', #22990 ) ;
#21842 = CARTESIAN_POINT ( 'NONE',  ( 15.55631266752686770, 12.59833113950373651, 6.641371103590088865 ) ) ;
#21843 = ORIENTED_EDGE ( 'NONE', *, *, #17585, .T. ) ;
#21844 = CARTESIAN_POINT ( 'NONE',  ( 16.18939002998178722, -5.436351910499668705, 6.447548852708279377 ) ) ;
#21845 = CARTESIAN_POINT ( 'NONE',  ( 16.55530288949897155, 4.194058762902726833, 19.47952243369110548 ) ) ;
#21846 = AXIS2_PLACEMENT_3D ( 'NONE', #17483, #27006, #3278 ) ;
#21847 = DIRECTION ( 'NONE',  ( 0.000000000000000000, -1.132880637372608986E-16, 1.000000000000000000 ) ) ;
#21848 = ORIENTED_EDGE ( 'NONE', *, *, #6711, .F. ) ;
#21849 = CARTESIAN_POINT ( 'NONE',  ( 1.000000000000008438, 16.48749217771910125, 1.500000000000000000 ) ) ;
#21850 = CARTESIAN_POINT ( 'NONE',  ( 23.62400240902268322, 9.724154461249522541, 49.47829057475696857 ) ) ;
#21851 = DIRECTION ( 'NONE',  ( 0.000000000000000000, -1.000000000000000000, 0.000000000000000000 ) ) ;
#21852 = CARTESIAN_POINT ( 'NONE',  ( 32.28307784207223108, 8.475829241206289666, 41.62281023987511475 ) ) ;
#21853 = ADVANCED_FACE ( 'NONE', ( #23444 ), #11605, .F. ) ;
#21854 = EDGE_CURVE ( 'NONE', #19078, #7329, #18633, .T. ) ;
#21855 = FACE_OUTER_BOUND ( 'NONE', #17546, .T. ) ;
#21856 = CARTESIAN_POINT ( 'NONE',  ( 26.80246859415415273, 7.028748154183637631, -16.50000000000000000 ) ) ;
#21857 = CYLINDRICAL_SURFACE ( 'NONE', #8899, 0.7500000000000006661 ) ;
#21858 = ORIENTED_EDGE ( 'NONE', *, *, #24280, .F. ) ;
#21859 = CARTESIAN_POINT ( 'NONE',  ( 24.44496207165490276, 7.595930209050162141, 49.40206402021032517 ) ) ;
#21860 = AXIS2_PLACEMENT_3D ( 'NONE', #11172, #18353, #6489 ) ;
#21861 = CARTESIAN_POINT ( 'NONE',  ( -40.89187623478217404, -5.790488632116337797, -19.50000000000000355 ) ) ;
#21862 = CIRCLE ( 'NONE', #13897, 10.00000000000000000 ) ;
#21863 = CARTESIAN_POINT ( 'NONE',  ( 52.16608720827707657, 36.86186943028246787, 57.49999999999999289 ) ) ;
#21864 = VERTEX_POINT ( 'NONE', #6313 ) ;
#21865 = CARTESIAN_POINT ( 'NONE',  ( -18.02885658979140970, -8.699255478180123902, 20.34789198813115263 ) ) ;
#21866 = DIRECTION ( 'NONE',  ( -1.000000000000000000, -0.000000000000000000, -0.000000000000000000 ) ) ;
#21867 = CARTESIAN_POINT ( 'NONE',  ( -14.69412328735587003, 13.56780452301002704, 19.60917204426170457 ) ) ;
#21868 = CARTESIAN_POINT ( 'NONE',  ( 5.016036949087496311, 16.26541432804313203, 6.714907520933423690 ) ) ;
#21869 = CARTESIAN_POINT ( 'NONE',  ( -19.64114023396299302, -37.13592150529018454, -1.500000000000000000 ) ) ;
#21870 = DIRECTION ( 'NONE',  ( -0.000000000000000000, -0.000000000000000000, -1.000000000000000000 ) ) ;
#21871 = CARTESIAN_POINT ( 'NONE',  ( 35.12146917884712138, 13.20565518866672505, 37.49999999998515676 ) ) ;
#21872 = CARTESIAN_POINT ( 'NONE',  ( 37.99999999999999289, 209.2686044187655909, -28.49999999999999645 ) ) ;
#21873 = ORIENTED_EDGE ( 'NONE', *, *, #24817, .F. ) ;
#21874 = VECTOR ( 'NONE', #4349, 1000.000000000000000 ) ;
#21875 = CARTESIAN_POINT ( 'NONE',  ( 33.35889463998532278, -23.76060433658897963, -9.833271769321870082 ) ) ;
#21876 = ORIENTED_EDGE ( 'NONE', *, *, #18952, .F. ) ;
#21877 = LINE ( 'NONE', #24201, #16176 ) ;
#21878 =( BOUNDED_CURVE ( )  B_SPLINE_CURVE ( 3, ( #27002, #5629, #8590, #15123 ),
 .UNSPECIFIED., .F., .T. ) 
 B_SPLINE_CURVE_WITH_KNOTS ( ( 4, 4 ),
 ( 5.540737561276206868, 5.872433067142492469 ),
 .UNSPECIFIED. ) 
 CURVE ( )  GEOMETRIC_REPRESENTATION_ITEM ( )  RATIONAL_B_SPLINE_CURVE ( ( 1.000000000000000000, 0.9908525036704132205, 0.9908525036704132205, 1.000000000000000000 ) ) 
 REPRESENTATION_ITEM ( '' )  );
#21879 = DIRECTION ( 'NONE',  ( 1.000000000000000000, 0.000000000000000000, 0.000000000000000000 ) ) ;
#21880 = ORIENTED_EDGE ( 'NONE', *, *, #649, .T. ) ;
#21881 = ORIENTED_EDGE ( 'NONE', *, *, #21704, .T. ) ;
#21882 = CARTESIAN_POINT ( 'NONE',  ( 22.94541271837968566, 35.03073867843525591, -6.499999999999999112 ) ) ;
#21883 = AXIS2_PLACEMENT_3D ( 'NONE', #81, #7246, #21591 ) ;
#21884 = ORIENTED_EDGE ( 'NONE', *, *, #2235, .T. ) ;
#21885 = ORIENTED_EDGE ( 'NONE', *, *, #2165, .F. ) ;
#21886 = DIRECTION ( 'NONE',  ( 0.000000000000000000, -1.132880637372608986E-16, 1.000000000000000000 ) ) ;
#21887 = CARTESIAN_POINT ( 'NONE',  ( -13.79366593457946344, 36.54982519354243209, 34.50000000000000000 ) ) ;
#21888 = DIRECTION ( 'NONE',  ( -1.000000000000000000, 0.000000000000000000, 0.000000000000000000 ) ) ;
#21889 = CARTESIAN_POINT ( 'NONE',  ( 5.009972004270265344, 16.26741710164193222, 19.47784884541372108 ) ) ;
#21890 = VECTOR ( 'NONE', #8966, 1000.000000000000000 ) ;
#21891 = PLANE ( 'NONE',  #30754 ) ;
#21892 = VERTEX_POINT ( 'NONE', #1645 ) ;
#21893 = DIRECTION ( 'NONE',  ( 0.000000000000000000, 0.000000000000000000, -1.000000000000000000 ) ) ;
#21894 = DIRECTION ( 'NONE',  ( -0.4495526574063634095, 0.8932538319083086487, 0.000000000000000000 ) ) ;
#21895 = CARTESIAN_POINT ( 'NONE',  ( 14.23411040819767059, 14.07463391211592274, 19.03762469184452755 ) ) ;
#21896 = FACE_OUTER_BOUND ( 'NONE', #16973, .T. ) ;
#21897 = VERTEX_POINT ( 'NONE', #9113 ) ;
#21898 = AXIS2_PLACEMENT_3D ( 'NONE', #20882, #30407, #11680 ) ;
#21899 = DIRECTION ( 'NONE',  ( 0.000000000000000000, 0.000000000000000000, 1.000000000000000000 ) ) ;
#21900 = CARTESIAN_POINT ( 'NONE',  ( -17.99270058295303443, -8.773758909272052264, 5.661398277488802755 ) ) ;
#21901 = CARTESIAN_POINT ( 'NONE',  ( -6.505190245242042479, 15.79074656234091556, 6.782048567692550378 ) ) ;
#21902 = LINE ( 'NONE', #21271, #5313 ) ;
#21903 = CARTESIAN_POINT ( 'NONE',  ( -15.49172192819003335, -7.063155179282991192, 18.71435384576123440 ) ) ;
#21904 = DIRECTION ( 'NONE',  ( 1.000000000000000000, 0.000000000000000000, 0.000000000000000000 ) ) ;
#21905 = ORIENTED_EDGE ( 'NONE', *, *, #20427, .F. ) ;
#21906 = DIRECTION ( 'NONE',  ( 1.000000000000000000, 0.000000000000000000, 0.000000000000000000 ) ) ;
#21907 = DIRECTION ( 'NONE',  ( -0.000000000000000000, -0.000000000000000000, -1.000000000000000000 ) ) ;
#21908 = FACE_OUTER_BOUND ( 'NONE', #1365, .T. ) ;
#21909 = LINE ( 'NONE', #5848, #121 ) ;
#21910 = ORIENTED_EDGE ( 'NONE', *, *, #18756, .T. ) ;
#21911 = APPLICATION_PROTOCOL_DEFINITION ( 'draft international standard', 'automotive_design', 1998, #10394 ) ;
#21912 = CIRCLE ( 'NONE', #28913, 0.7500000000000006661 ) ;
#21913 = FACE_OUTER_BOUND ( 'NONE', #19408, .T. ) ;
#21914 = DIRECTION ( 'NONE',  ( 0.6548607339452890974, 0.7557495743542548272, 0.000000000000000000 ) ) ;
#21915 = VERTEX_POINT ( 'NONE', #11158 ) ;
#21916 = CARTESIAN_POINT ( 'NONE',  ( 45.00000000000045475, -4.871505565812501079E-13, 77.49999999999998579 ) ) ;
#21917 = CARTESIAN_POINT ( 'NONE',  ( 8.884323311075775109, 1.438332125858202692, 1.500000000000001332 ) ) ;
#21918 = AXIS2_PLACEMENT_3D ( 'NONE', #6032, #3385, #12915 ) ;
#21919 = CARTESIAN_POINT ( 'NONE',  ( -7.717362503654372041, -15.23305454438880702, 19.02573955821369367 ) ) ;
#21920 = CARTESIAN_POINT ( 'NONE',  ( -30.34931995752844358, -22.03541669038290607, 37.50000000004472867 ) ) ;
#21921 = ORIENTED_EDGE ( 'NONE', *, *, #1489, .F. ) ;
#21922 = CARTESIAN_POINT ( 'NONE',  ( -24.44496207165490276, 7.595930209050158588, 49.40206402021040333 ) ) ;
#21923 = PRODUCT_DEFINITION ( 'UNKNOWN', '', #14376, #17636 ) ;
#21924 = CARTESIAN_POINT ( 'NONE',  ( -12.56641067637617759, -40.32935944494947478, -1.500000000000000000 ) ) ;
#21925 = DIRECTION ( 'NONE',  ( -0.000000000000000000, -0.000000000000000000, -1.000000000000000000 ) ) ;
#21926 = EDGE_CURVE ( 'NONE', #3976, #21977, #12373, .T. ) ;
#21927 = ORIENTED_EDGE ( 'NONE', *, *, #16972, .T. ) ;
#21928 = CARTESIAN_POINT ( 'NONE',  ( 7.856594496258195726, 4.390207617113981442, -1.500000000000001332 ) ) ;
#21929 = DIRECTION ( 'NONE',  ( -0.000000000000000000, -0.000000000000000000, -1.000000000000000000 ) ) ;
#21930 = EDGE_CURVE ( 'NONE', #1203, #8258, #4362, .T. ) ;
#21931 = CIRCLE ( 'NONE', #14965, 0.7500000000000006661 ) ;
#21932 = DIRECTION ( 'NONE',  ( 1.000000000000000000, 0.000000000000000000, 0.000000000000000000 ) ) ;
#21933 = CARTESIAN_POINT ( 'NONE',  ( -5.881244434206279514, -6.812559277181949646, 21.50000000000000000 ) ) ;
#21934 = CARTESIAN_POINT ( 'NONE',  ( 35.76324912335250161, -16.99827115821247858, 8.803654662221047644 ) ) ;
#21935 = CARTESIAN_POINT ( 'NONE',  ( 24.03057240117691862, -26.57182937991349903, -6.500000000000000888 ) ) ;
#21936 = ORIENTED_EDGE ( 'NONE', *, *, #20894, .F. ) ;
#21937 = ADVANCED_FACE ( 'NONE', ( #13658 ), #15668, .F. ) ;
#21938 = DIRECTION ( 'NONE',  ( -1.000000000000000000, 0.000000000000000000, 0.000000000000000000 ) ) ;
#21939 = CARTESIAN_POINT ( 'NONE',  ( 45.00000000000045475, -4.871505565812501079E-13, 57.49999999999999289 ) ) ;
#21940 = EDGE_CURVE ( 'NONE', #1863, #18281, #16636, .T. ) ;
#21941 = EDGE_LOOP ( 'NONE', ( #23737, #8733, #7788, #12707, #20007, #29447, #4640, #28454, #8058, #17388, #747, #29803, #21706, #28926, #19895, #12755 ) ) ;
#21942 = ORIENTED_EDGE ( 'NONE', *, *, #5558, .F. ) ;
#21943 = EDGE_CURVE ( 'NONE', #5756, #12636, #11884, .T. ) ;
#21944 = DIRECTION ( 'NONE',  ( 0.2817325568414296710, 0.9594929736144973687, -0.000000000000000000 ) ) ;
#21945 = CARTESIAN_POINT ( 'NONE',  ( -14.97621673923063312, 47.70446069948408763, -55.98035886673119421 ) ) ;
#21946 = ORIENTED_EDGE ( 'NONE', *, *, #22309, .F. ) ;
#21947 = CARTESIAN_POINT ( 'NONE',  ( 15.52282850165806138, 12.63957212366657501, 19.66989035740801839 ) ) ;
#21948 = CARTESIAN_POINT ( 'NONE',  ( -26.36764545593177544, -31.31467416275353344, 1.500000000000000000 ) ) ;
#21949 = ORIENTED_EDGE ( 'NONE', *, *, #11661, .T. ) ;
#21950 = CARTESIAN_POINT ( 'NONE',  ( 2.878478920843521749, -0.8451976705243363641, 24.50000000000000000 ) ) ;
#21951 = CARTESIAN_POINT ( 'NONE',  ( 19.64806919293055287, 3.830191698062870742, 18.56793045041961321 ) ) ;
#21952 = AXIS2_PLACEMENT_3D ( 'NONE', #9814, #19327, #1235 ) ;
#21953 = DIRECTION ( 'NONE',  ( 0.000000000000000000, 0.000000000000000000, -1.000000000000000000 ) ) ;
#21954 = EDGE_LOOP ( 'NONE', ( #15782, #26833, #29721, #16591 ) ) ;
#21955 = CARTESIAN_POINT ( 'NONE',  ( 0.000000000000000000, 0.000000000000000000, 21.50000000000000000 ) ) ;
#21956 = EDGE_CURVE ( 'NONE', #26848, #19902, #2884, .T. ) ;
#21957 = VERTEX_POINT ( 'NONE', #9720 ) ;
#21958 = EDGE_CURVE ( 'NONE', #16110, #30524, #5051, .T. ) ;
#21959 = ADVANCED_FACE ( 'NONE', ( #23915 ), #24559, .T. ) ;
#21960 = EDGE_CURVE ( 'NONE', #15068, #23022, #10650, .T. ) ;
#21961 = ORIENTED_EDGE ( 'NONE', *, *, #14370, .F. ) ;
#21962 = EDGE_CURVE ( 'NONE', #10235, #25178, #20842, .T. ) ;
#21963 = CARTESIAN_POINT ( 'NONE',  ( 27.29267191310605156, 30.38807181596501650, 30.00869227221143731 ) ) ;
#21964 = CARTESIAN_POINT ( 'NONE',  ( -6.723597995833587859, 18.85470073956823711, 19.97651184436794125 ) ) ;
#21965 = CARTESIAN_POINT ( 'NONE',  ( -12.81506474335657408, 11.20733750501348425, 18.80699882434806369 ) ) ;
#21966 = DIRECTION ( 'NONE',  ( 1.000000000000000000, 0.000000000000000000, 0.000000000000000000 ) ) ;
#21967 = EDGE_CURVE ( 'NONE', #15826, #10427, #5357, .T. ) ;
#21968 = CARTESIAN_POINT ( 'NONE',  ( -31.29189664795533332, -25.39986983782039687, 30.52943660264045178 ) ) ;
#21969 = CARTESIAN_POINT ( 'NONE',  ( -37.16608720827707657, 51.86186943028246787, 12.49999999999999112 ) ) ;
#21970 = FACE_OUTER_BOUND ( 'NONE', #21292, .T. ) ;
#21971 = ORIENTED_EDGE ( 'NONE', *, *, #16253, .T. ) ;
#21972 = EDGE_CURVE ( 'NONE', #8400, #7329, #8397, .T. ) ;
#21973 = CARTESIAN_POINT ( 'NONE',  ( 9.096230214749077447, -14.38931669386025192, 6.211014596808754007 ) ) ;
#21974 = CARTESIAN_POINT ( 'NONE',  ( 69.99999999999998579, -50.00000000000000000, 12.49999999999999112 ) ) ;
#21975 = VECTOR ( 'NONE', #23155, 1000.000000000000000 ) ;
#21976 = CARTESIAN_POINT ( 'NONE',  ( 9.640932123708072510, -14.04859418185266584, 7.626437579292365321 ) ) ;
#21977 = VERTEX_POINT ( 'NONE', #7853 ) ;
#21978 = ORIENTED_EDGE ( 'NONE', *, *, #2285, .F. ) ;
#21979 = DIRECTION ( 'NONE',  ( 0.000000000000000000, -1.000000000000000000, 0.000000000000000000 ) ) ;
#21980 = DIRECTION ( 'NONE',  ( 0.000000000000000000, 0.000000000000000000, 1.000000000000000000 ) ) ;
#21981 = CARTESIAN_POINT ( 'NONE',  ( 18.53278507915171147, -7.520016387818814430, 20.22386025856690495 ) ) ;
#21982 = CARTESIAN_POINT ( 'NONE',  ( 8.499586724479435418, 2.959227181723830036, 21.50000000000000000 ) ) ;
#21983 = DIRECTION ( 'NONE',  ( -0.000000000000000000, -0.000000000000000000, 1.000000000000000000 ) ) ;
#21984 = CARTESIAN_POINT ( 'NONE',  ( 6.262045289545330462, 18.99438835075423881, 6.518927109361845496 ) ) ;
#21985 = EDGE_CURVE ( 'NONE', #9360, #20390, #22189, .T. ) ;
#21986 = ORIENTED_EDGE ( 'NONE', *, *, #4768, .T. ) ;
#21987 = VECTOR ( 'NONE', #11974, 1000.000000000000000 ) ;
#21988 = CARTESIAN_POINT ( 'NONE',  ( -6.974883619896829146, -5.687793815610328707, 21.50000000000000000 ) ) ;
#21989 = DIRECTION ( 'NONE',  ( 1.000000000000000000, 0.000000000000000000, 0.000000000000000000 ) ) ;
#21990 = CARTESIAN_POINT ( 'NONE',  ( 19.82764810689592849, 2.754998275627142945, 7.557577766377196582 ) ) ;
#21991 = ORIENTED_EDGE ( 'NONE', *, *, #1524, .F. ) ;
#21992 = CARTESIAN_POINT ( 'NONE',  ( 12.88134121443597380, 11.13293444107316787, 7.272049892295485485 ) ) ;
#21993 = EDGE_CURVE ( 'NONE', #26065, #6853, #30794, .T. ) ;
#21994 = ORIENTED_EDGE ( 'NONE', *, *, #20621, .F. ) ;
#21995 = CARTESIAN_POINT ( 'NONE',  ( 18.48179574117062529, -7.690589227441819276, 7.603368798681074736 ) ) ;
#21996 = EDGE_CURVE ( 'NONE', #20433, #15822, #29316, .T. ) ;
#21997 = CARTESIAN_POINT ( 'NONE',  ( 16.55667234709053659, 4.187688857952014843, 19.21769074125272425 ) ) ;
#21998 = VECTOR ( 'NONE', #4286, 1000.000000000000000 ) ;
#21999 = DIRECTION ( 'NONE',  ( 0.000000000000000000, 0.000000000000000000, 1.000000000000000000 ) ) ;
#22000 = ORIENTED_EDGE ( 'NONE', *, *, #23269, .F. ) ;
#22001 = CARTESIAN_POINT ( 'NONE',  ( -11.82521593960875528, 5.400395169024524655, 1.500000000000001332 ) ) ;
#22002 = DIRECTION ( 'NONE',  ( 0.000000000000000000, -1.000000000000000000, 0.000000000000000000 ) ) ;
#22003 = CARTESIAN_POINT ( 'NONE',  ( 4.668110441710642711, -19.44758969394385062, 1.500000000000001332 ) ) ;
#22004 = CARTESIAN_POINT ( 'NONE',  ( 1.015311529865299489, 39.50000000000000000, 34.49999999999999289 ) ) ;
#22005 = CARTESIAN_POINT ( 'NONE',  ( -35.13669516613692423, -8.778141986582063794, 34.58384122122906490 ) ) ;
#22006 = CARTESIAN_POINT ( 'NONE',  ( 31.57476163834523675, 15.10795358447670189, 39.99718304312875716 ) ) ;
#22007 = AXIS2_PLACEMENT_3D ( 'NONE', #13775, #11443, #20929 ) ;
#22008 = CARTESIAN_POINT ( 'NONE',  ( -5.069257791428326776, 7.538175180318475554, -1.500000000000000888 ) ) ;
#22009 = CARTESIAN_POINT ( 'NONE',  ( -13.38159811071079552, 10.55828946507379307, 18.34798005862662507 ) ) ;
#22010 = CARTESIAN_POINT ( 'NONE',  ( 46.04937334709716623, 69.44700547456450579, 60.46534098734598928 ) ) ;
#22011 = ORIENTED_EDGE ( 'NONE', *, *, #29576, .T. ) ;
#22012 = CARTESIAN_POINT ( 'NONE',  ( 29.79020748929575291, -27.43254185190355443, 16.85628874541750477 ) ) ;
#22013 = DIRECTION ( 'NONE',  ( 0.000000000000000000, 1.000000000000000000, 0.000000000000000000 ) ) ;
#22014 = DIRECTION ( 'NONE',  ( 0.000000000000000000, 1.000000000000000000, 0.000000000000000000 ) ) ;
#22015 = DIRECTION ( 'NONE',  ( 0.000000000000000000, 0.000000000000000000, 1.000000000000000000 ) ) ;
#22016 = AXIS2_PLACEMENT_3D ( 'NONE', #5091, #14276, #16783 ) ;
#22017 = CARTESIAN_POINT ( 'NONE',  ( -23.96732207938974213, -33.98584080153308662, -1.500000000000000000 ) ) ;
#22018 = DIRECTION ( 'NONE',  ( -0.9898214418809326842, -0.1423148382732852824, 0.000000000000000000 ) ) ;
#22019 = CARTESIAN_POINT ( 'NONE',  ( 3.763133143576435913, -8.268028093133381162, 13.22130136205108641 ) ) ;
#22020 = EDGE_CURVE ( 'NONE', #27558, #22434, #8322, .T. ) ;
#22021 = CARTESIAN_POINT ( 'NONE',  ( -25.07950435457407323, -11.50806656539752737, -16.55003854064094426 ) ) ;
#22022 = ORIENTED_EDGE ( 'NONE', *, *, #15441, .F. ) ;
#22023 = FACE_OUTER_BOUND ( 'NONE', #29061, .T. ) ;
#22024 = VERTEX_POINT ( 'NONE', #24995 ) ;
#22025 = DIRECTION ( 'NONE',  ( 0.000000000000000000, 0.000000000000000000, -1.000000000000000000 ) ) ;
#22026 = DIRECTION ( 'NONE',  ( -0.000000000000000000, -0.000000000000000000, 1.000000000000000000 ) ) ;
#22027 = ORIENTED_EDGE ( 'NONE', *, *, #16675, .T. ) ;
#22028 = ORIENTED_EDGE ( 'NONE', *, *, #14891, .T. ) ;
#22029 = DIRECTION ( 'NONE',  ( 0.000000000000000000, 0.000000000000000000, 1.000000000000000000 ) ) ;
#22030 = CIRCLE ( 'NONE', #9594, 20.32284676574536064 ) ;
#22031 = ORIENTED_EDGE ( 'NONE', *, *, #5780, .T. ) ;
#22032 = ORIENTED_EDGE ( 'NONE', *, *, #5727, .T. ) ;
#22033 = EDGE_LOOP ( 'NONE', ( #19583, #15219, #19028, #26996 ) ) ;
#22034 = CARTESIAN_POINT ( 'NONE',  ( -4.608906612435655248, -7.730328572437724866, -1.500000000000002665 ) ) ;
#22035 = DIRECTION ( 'NONE',  ( 0.000000000000000000, 0.000000000000000000, 1.000000000000000000 ) ) ;
#22036 = DIRECTION ( 'NONE',  ( -0.000000000000000000, -0.000000000000000000, 1.000000000000000000 ) ) ;
#22037 = CARTESIAN_POINT ( 'NONE',  ( -37.40739136233791129, 12.02481294536538847, 15.34406802053112706 ) ) ;
#22038 = DIRECTION ( 'NONE',  ( -0.000000000000000000, 1.000000000000000000, -0.000000000000000000 ) ) ;
#22039 = VERTEX_POINT ( 'NONE', #3320 ) ;
#22040 = CARTESIAN_POINT ( 'NONE',  ( -11.25470158702820456, -16.53282404628957991, 7.156831654632821227 ) ) ;
#22041 = DIRECTION ( 'NONE',  ( -0.9329908884337543284, -0.3598999890241648125, 0.000000000000000000 ) ) ;
#22042 = FACE_OUTER_BOUND ( 'NONE', #2112, .T. ) ;
#22043 = FACE_BOUND ( 'NONE', #29484, .T. ) ;
#22044 = ORIENTED_EDGE ( 'NONE', *, *, #14496, .F. ) ;
#22045 = DIRECTION ( 'NONE',  ( -1.000000000000000000, 0.000000000000000000, 0.000000000000000000 ) ) ;
#22046 = CARTESIAN_POINT ( 'NONE',  ( -17.64660589602034690, -9.450098986197513540, 7.098451512883313441 ) ) ;
#22047 = CARTESIAN_POINT ( 'NONE',  ( -5.764374838704561910, 16.04809504443726098, 5.678370764302467677 ) ) ;
#22048 = FACE_OUTER_BOUND ( 'NONE', #10717, .T. ) ;
#22049 = VECTOR ( 'NONE', #9097, 1000.000000000000000 ) ;
#22050 = CARTESIAN_POINT ( 'NONE',  ( -15.56928374346769495, -6.880100827600170277, 19.11611934778430921 ) ) ;
#22051 = DIRECTION ( 'NONE',  ( 1.000000000000000000, 0.000000000000000000, 0.000000000000000000 ) ) ;
#22052 = ORIENTED_EDGE ( 'NONE', *, *, #8098, .F. ) ;
#22053 = ORIENTED_EDGE ( 'NONE', *, *, #16997, .T. ) ;
#22054 =( BOUNDED_CURVE ( )  B_SPLINE_CURVE ( 3, ( #10668, #20174, #4113, #30011 ),
 .UNSPECIFIED., .F., .F. ) 
 B_SPLINE_CURVE_WITH_KNOTS ( ( 4, 4 ),
 ( 0.4107522400370940407, 0.7424477459033789195 ),
 .UNSPECIFIED. ) 
 CURVE ( )  GEOMETRIC_REPRESENTATION_ITEM ( )  RATIONAL_B_SPLINE_CURVE ( ( 1.000000000000000000, 0.9908525036704132205, 0.9908525036704132205, 1.000000000000000000 ) ) 
 REPRESENTATION_ITEM ( '' )  );
#22055 = DIRECTION ( 'NONE',  ( -1.000000000000000000, 0.000000000000000000, 0.000000000000000000 ) ) ;
#22056 = DIRECTION ( 'NONE',  ( -0.000000000000000000, -0.000000000000000000, 1.000000000000000000 ) ) ;
#22057 = CARTESIAN_POINT ( 'NONE',  ( -14.78913018809137370, 13.49064936509565982, 7.176035686813569292 ) ) ;
#22058 = CARTESIAN_POINT ( 'NONE',  ( 1.530808498934191521E-15, -12.50000000000000000, -87.50000000000000000 ) ) ;
#22059 = ORIENTED_EDGE ( 'NONE', *, *, #11159, .F. ) ;
#22060 = APPLICATION_PROTOCOL_DEFINITION ( 'draft international standard', 'automotive_design', 1998, #23710 ) ;
#22061 = DIRECTION ( 'NONE',  ( -0.000000000000000000, 1.000000000000000000, -0.000000000000000000 ) ) ;
#22062 = ADVANCED_FACE ( 'NONE', ( #5820 ), #12850, .F. ) ;
#22063 = DIRECTION ( 'NONE',  ( 0.000000000000000000, 0.000000000000000000, 1.000000000000000000 ) ) ;
#22064 = ORIENTED_EDGE ( 'NONE', *, *, #27567, .T. ) ;
#22065 = CARTESIAN_POINT ( 'NONE',  ( 4.564720541824407896, 16.40857754966928184, 18.49267272388512140 ) ) ;
#22066 = CARTESIAN_POINT ( 'NONE',  ( 0.000000000000000000, 0.000000000000000000, -16.50000000000000000 ) ) ;
#22067 = CARTESIAN_POINT ( 'NONE',  ( 0.000000000000000000, 0.000000000000000000, 1.500000000000001332 ) ) ;
#22068 = CARTESIAN_POINT ( 'NONE',  ( -29.59797164802278857, -23.03477555636723650, 37.49999999995527133 ) ) ;
#22069 = ORIENTED_EDGE ( 'NONE', *, *, #22945, .F. ) ;
#22070 = DIRECTION ( 'NONE',  ( -0.000000000000000000, -0.000000000000000000, -1.000000000000000000 ) ) ;
#22071 = AXIS2_PLACEMENT_3D ( 'NONE', #9969, #7621, #10429 ) ;
#22072 = CIRCLE ( 'NONE', #14120, 0.7500000000000006661 ) ;
#22073 = DIRECTION ( 'NONE',  ( 0.000000000000000000, 0.000000000000000000, 1.000000000000000000 ) ) ;
#22074 = CARTESIAN_POINT ( 'NONE',  ( 24.03057240117691862, 26.57182937991349903, 1.500000000000000000 ) ) ;
#22075 = ORIENTED_EDGE ( 'NONE', *, *, #24594, .F. ) ;
#22076 = DIRECTION ( 'NONE',  ( -0.000000000000000000, -0.000000000000000000, 1.000000000000000000 ) ) ;
#22077 = CARTESIAN_POINT ( 'NONE',  ( 14.73074142449663881, 5.627958522269737252, 24.50000000000000000 ) ) ;
#22078 =( NAMED_UNIT ( * ) PLANE_ANGLE_UNIT ( ) SI_UNIT ( $, .RADIAN. ) );
#22079 = LINE ( 'NONE', #27083, #839 ) ;
#22080 = DIRECTION ( 'NONE',  ( -0.000000000000000000, -0.000000000000000000, 1.000000000000000000 ) ) ;
#22081 = DIRECTION ( 'NONE',  ( 1.000000000000000000, 0.000000000000000000, 0.000000000000000000 ) ) ;
#22082 = CARTESIAN_POINT ( 'NONE',  ( 37.63480807633214198, -11.15005181301510362, 14.85427662740586463 ) ) ;
#22083 = DIRECTION ( 'NONE',  ( 0.000000000000000000, 0.000000000000000000, -1.000000000000000000 ) ) ;
#22084 = ORIENTED_EDGE ( 'NONE', *, *, #7279, .T. ) ;
#22085 = CARTESIAN_POINT ( 'NONE',  ( 0.000000000000000000, 0.000000000000000000, 1.500000000000001332 ) ) ;
#22086 = AXIS2_PLACEMENT_3D ( 'NONE', #27048, #20016, #27198 ) ;
#22087 = CARTESIAN_POINT ( 'NONE',  ( -19.84344116185557283, 2.497567387674354489, 7.652108011868850035 ) ) ;
#22088 = ORIENTED_EDGE ( 'NONE', *, *, #17973, .F. ) ;
#22089 = ORIENTED_EDGE ( 'NONE', *, *, #4571, .F. ) ;
#22090 = EDGE_CURVE ( 'NONE', #10953, #20218, #24849, .T. ) ;
#22091 = CIRCLE ( 'NONE', #21079, 0.7500000000000006661 ) ;
#22092 = CARTESIAN_POINT ( 'NONE',  ( -1.438332125858111432, 8.884323311075791096, 21.50000000000000000 ) ) ;
#22093 = DIRECTION ( 'NONE',  ( -0.000000000000000000, -0.000000000000000000, -1.000000000000000000 ) ) ;
#22094 = CIRCLE ( 'NONE', #182, 20.00000000000000355 ) ;
#22095 = ORIENTED_EDGE ( 'NONE', *, *, #5362, .F. ) ;
#22096 = CARTESIAN_POINT ( 'NONE',  ( -6.191185452821632573, -38.91708858248148317, 27.50000000000000000 ) ) ;
#22097 = CARTESIAN_POINT ( 'NONE',  ( 12.57902516942791493, 11.48976026227457936, 18.39701043959520987 ) ) ;
#22098 = B_SPLINE_CURVE_WITH_KNOTS ( 'NONE', 3,
 ( #8764, #10971, #27350, #12997, #17834, #1459, #18289, #8488, #22641, #27647, #13473, #13307, #5975, #22805, #17990, #6437, #22954, #11118 ),
 .UNSPECIFIED., .F., .F.,
 ( 4, 2, 2, 2, 2, 2, 2, 2, 4 ),
 ( 0.003174295595554288765, 0.003570702171545512855, 0.003967108747536736944, 0.004363515323527961468, 0.004759921899519185123, 0.005156328475510408779, 0.005552735051501633302, 0.005949141627492857826, 0.006345548203484081481 ),
 .UNSPECIFIED. ) ;
#22099 = ADVANCED_FACE ( 'NONE', ( #3485 ), #26890, .F. ) ;
#22100 = ORIENTED_EDGE ( 'NONE', *, *, #24030, .T. ) ;
#22101 = EDGE_CURVE ( 'NONE', #14088, #6009, #5978, .T. ) ;
#22102 = CARTESIAN_POINT ( 'NONE',  ( 18.43859109590531276, -7.792859017390148857, 20.32367522806703874 ) ) ;
#22103 = CARTESIAN_POINT ( 'NONE',  ( 18.28487737789067324, -8.104377114558880990, 5.651480102388687143 ) ) ;
#22104 = CARTESIAN_POINT ( 'NONE',  ( 40.53905774364188375, 2.041855955180682081, -16.50000000000000355 ) ) ;
#22105 = EDGE_LOOP ( 'NONE', ( #13491, #27833, #21402, #25037 ) ) ;
#22106 = CARTESIAN_POINT ( 'NONE',  ( -4.699300155657183176, 16.36248368692915989, 18.83976166372256245 ) ) ;
#22107 = ORIENTED_EDGE ( 'NONE', *, *, #799, .F. ) ;
#22108 = B_SPLINE_CURVE_WITH_KNOTS ( 'NONE', 3,
 ( #19104, #28620, #7244, #10121, #29899, #5292, #29318, #9983, #3114, #26661, #30041, #5456, #14958, #24317, #3693, #25364, #12483, #3997 ),
 .UNSPECIFIED., .F., .F.,
 ( 4, 2, 2, 2, 2, 2, 2, 2, 4 ),
 ( 0.003174295595554316521, 0.003570702171545547983, 0.003967108747536779445, 0.004363515323528011775, 0.004759921899519242369, 0.005156328475510474699, 0.005552735051501706161, 0.005949141627492937623, 0.006345548203484169085 ),
 .UNSPECIFIED. ) ;
#22109 = CARTESIAN_POINT ( 'NONE',  ( 6.176953700987930951, 38.93706494759733516, 27.50000000000000355 ) ) ;
#22110 = ORIENTED_EDGE ( 'NONE', *, *, #29608, .T. ) ;
#22111 = EDGE_CURVE ( 'NONE', #11519, #6070, #3419, .T. ) ;
#22112 = CIRCLE ( 'NONE', #12675, 0.7499999999999997780 ) ;
#22113 = CARTESIAN_POINT ( 'NONE',  ( 28.56150147175966936, 28.94728505588477674, 30.15884368954713679 ) ) ;
#22114 = CARTESIAN_POINT ( 'NONE',  ( 16.66634534075878094, 3.639270104310704745, 5.749491821935610147 ) ) ;
#22115 = CARTESIAN_POINT ( 'NONE',  ( -14.68399241520484111, 13.60504237629023194, 19.33715507985239412 ) ) ;
#22116 = CARTESIAN_POINT ( 'NONE',  ( -19.54426622602688468, 37.07991288358297055, -1.499999999999999778 ) ) ;
#22117 = CARTESIAN_POINT ( 'NONE',  ( -31.36844279130544777, 25.28729038194961731, 30.54136519211768430 ) ) ;
#22118 = CARTESIAN_POINT ( 'NONE',  ( 77.99999999999998579, 42.50000000000000711, 32.26246401786215756 ) ) ;
#22119 = CARTESIAN_POINT ( 'NONE',  ( 37.16608720827707657, -36.86186943028246787, 97.07879600563551037 ) ) ;
#22120 = ORIENTED_EDGE ( 'NONE', *, *, #6157, .T. ) ;
#22121 = CARTESIAN_POINT ( 'NONE',  ( -19.91230480659700319, 2.053870633397346435, 5.749491821935610147 ) ) ;
#22122 = CARTESIAN_POINT ( 'NONE',  ( 33.53502205450880069, -14.39784139885291836, 34.49999999999999289 ) ) ;
#22123 = ADVANCED_FACE ( 'NONE', ( #518 ), #24528, .T. ) ;
#22124 = FACE_BOUND ( 'NONE', #3266, .T. ) ;
#22125 = ORIENTED_EDGE ( 'NONE', *, *, #30529, .T. ) ;
#22126 = ORIENTED_EDGE ( 'NONE', *, *, #868, .T. ) ;
#22127 = DIRECTION ( 'NONE',  ( -0.000000000000000000, 0.000000000000000000, 1.000000000000000000 ) ) ;
#22128 = EDGE_CURVE ( 'NONE', #16170, #25535, #22828, .T. ) ;
#22129 = CARTESIAN_POINT ( 'NONE',  ( 25.64627119138473432, -23.40052582045089480, -16.50000000000000000 ) ) ;
#22130 = EDGE_CURVE ( 'NONE', #30416, #11554, #22979, .T. ) ;
#22131 = PRODUCT ( 'MAS-342', 'MAS-342', '', ( #5079 ) ) ;
#22132 = DIRECTION ( 'NONE',  ( 1.000000000000000000, 0.000000000000000000, 0.000000000000000000 ) ) ;
#22133 = ORIENTED_EDGE ( 'NONE', *, *, #13572, .F. ) ;
#22134 = DIRECTION ( 'NONE',  ( 0.000000000000000000, -1.132880637372608986E-16, 1.000000000000000000 ) ) ;
#22135 = CARTESIAN_POINT ( 'NONE',  ( 6.812559277181973627, -5.881244434206257310, 1.500000000000001332 ) ) ;
#22136 = CIRCLE ( 'NONE', #1226, 0.7499999999999997780 ) ;
#22137 = EDGE_CURVE ( 'NONE', #2587, #2272, #12696, .T. ) ;
#22138 = LINE ( 'NONE', #17151, #20385 ) ;
#22139 = ORIENTED_EDGE ( 'NONE', *, *, #5567, .T. ) ;
#22140 = EDGE_CURVE ( 'NONE', #4513, #2571, #2080, .T. ) ;
#22141 = DIRECTION ( 'NONE',  ( 1.000000000000000000, 0.000000000000000000, -0.000000000000000000 ) ) ;
#22142 = CARTESIAN_POINT ( 'NONE',  ( -50.00000000000000000, -50.00000000000000000, 12.49999999999999112 ) ) ;
#22143 = CARTESIAN_POINT ( 'NONE',  ( 16.87846183053957461, 2.201534687727673578, 6.530762810602277924 ) ) ;
#22144 = EDGE_CURVE ( 'NONE', #10762, #4980, #10391, .T. ) ;
#22145 = ORIENTED_EDGE ( 'NONE', *, *, #7857, .T. ) ;
#22146 = CARTESIAN_POINT ( 'NONE',  ( 14.97341519046260494, 13.28616376876794547, 7.652108011868850035 ) ) ;
#22147 = EDGE_LOOP ( 'NONE', ( #23720, #12845, #27617, #15574 ) ) ;
#22148 = EDGE_CURVE ( 'NONE', #13692, #28753, #3662, .T. ) ;
#22149 = DIRECTION ( 'NONE',  ( -1.000000000000000000, 0.000000000000000000, 0.000000000000000000 ) ) ;
#22150 = B_SPLINE_CURVE_WITH_KNOTS ( 'NONE', 3,
 ( #24479, #762, #15260, #15115, #10286, #7645, #19638 ),
 .UNSPECIFIED., .F., .F.,
 ( 4, 3, 4 ),
 ( 0.000000000000000000, 0.005028111721406030438, 0.01005622344633218777 ),
 .UNSPECIFIED. ) ;
#22151 = CARTESIAN_POINT ( 'NONE',  ( -32.60829997825918980, 13.18983524832148291, 39.84356070656662041 ) ) ;
#22152 = ADVANCED_FACE ( 'NONE', ( #5158 ), #23442, .F. ) ;
#22153 = CARTESIAN_POINT ( 'NONE',  ( -25.18466322232233523, 6.657711795334218863, 44.70772167919928108 ) ) ;
#22154 = VERTEX_POINT ( 'NONE', #13796 ) ;
#22155 = EDGE_CURVE ( 'NONE', #194, #13705, #27832, .T. ) ;
#22156 = CARTESIAN_POINT ( 'NONE',  ( 6.899999999999999467, 5.196152422706634688, -9.000000000000001776 ) ) ;
#22157 = ORIENTED_EDGE ( 'NONE', *, *, #19319, .F. ) ;
#22158 = LINE ( 'NONE', #17168, #21249 ) ;
#22159 = AXIS2_PLACEMENT_3D ( 'NONE', #4425, #16431, #13940 ) ;
#22160 = CARTESIAN_POINT ( 'NONE',  ( -27.03943647958860552, 26.20092231554396633, 34.80090346875805096 ) ) ;
#22161 = CARTESIAN_POINT ( 'NONE',  ( 10.33891776879019808, -17.14136798460503996, 19.77662771831109367 ) ) ;
#22162 = DIRECTION ( 'NONE',  ( 1.000000000000000000, 0.000000000000000000, 0.000000000000000000 ) ) ;
#22163 = ORIENTED_EDGE ( 'NONE', *, *, #15083, .T. ) ;
#22164 = CARTESIAN_POINT ( 'NONE',  ( -25.18096005886327760, -6.640581704039637323, 48.95928115109028766 ) ) ;
#22165 = CARTESIAN_POINT ( 'NONE',  ( -13.52555592105307980, 10.38406032642568455, 18.37415474056476938 ) ) ;
#22166 = DIRECTION ( 'NONE',  ( 0.000000000000000000, 0.000000000000000000, 1.000000000000000000 ) ) ;
#22167 = ORIENTED_EDGE ( 'NONE', *, *, #23049, .F. ) ;
#22168 = CARTESIAN_POINT ( 'NONE',  ( 32.52553806410312376, -23.45536643706434532, 8.015563212847093055 ) ) ;
#22169 = EDGE_CURVE ( 'NONE', #19541, #8561, #5480, .T. ) ;
#22170 = PLANE ( 'NONE',  #27186 ) ;
#22171 = EDGE_CURVE ( 'NONE', #3179, #12072, #12897, .T. ) ;
#22172 = CARTESIAN_POINT ( 'NONE',  ( 32.24119409414369386, 26.76047229433004659, -16.50000600000000262 ) ) ;
#22173 = CARTESIAN_POINT ( 'NONE',  ( 8.606594496258196614, 4.390207617113981442, 21.50000000000000000 ) ) ;
#22174 = CARTESIAN_POINT ( 'NONE',  ( 5.105024945674004222, 42.22604126506330857, -1.500000000000000000 ) ) ;
#22175 = ADVANCED_FACE ( 'NONE', ( #4268 ), #19192, .F. ) ;
#22176 = FACE_OUTER_BOUND ( 'NONE', #8685, .T. ) ;
#22177 = DIRECTION ( 'NONE',  ( -0.000000000000000000, -0.000000000000000000, 1.000000000000000000 ) ) ;
#22178 = CARTESIAN_POINT ( 'NONE',  ( 19.63396244889325715, 3.810028285208273857, 5.853797745100183469 ) ) ;
#22179 = VERTEX_POINT ( 'NONE', #318 ) ;
#22180 = CARTESIAN_POINT ( 'NONE',  ( 24.03057240117691862, 26.57182937991349903, 1.500000000000001332 ) ) ;
#22181 = CARTESIAN_POINT ( 'NONE',  ( -4.163336342344337027E-14, 1.387778780781445676E-14, 1.500000000000000000 ) ) ;
#22182 = CARTESIAN_POINT ( 'NONE',  ( 9.436481611552752113, 0.9307681286968852996, 13.00000000000000178 ) ) ;
#22183 = ORIENTED_EDGE ( 'NONE', *, *, #7231, .T. ) ;
#22184 = AXIS2_PLACEMENT_3D ( 'NONE', #11712, #4689, #11421 ) ;
#22185 = ORIENTED_EDGE ( 'NONE', *, *, #14908, .F. ) ;
#22186 = ADVANCED_FACE ( 'NONE', ( #627 ), #28878, .F. ) ;
#22187 = CARTESIAN_POINT ( 'NONE',  ( -8.795879380940579750, -2.270234684139648795, -1.500000000000001998 ) ) ;
#22188 = VERTEX_POINT ( 'NONE', #16283 ) ;
#22189 = LINE ( 'NONE', #19548, #25819 ) ;
#22190 = CARTESIAN_POINT ( 'NONE',  ( -8.523310919002204500, 38.38027722185356083, 34.49999999999998579 ) ) ;
#22191 = CARTESIAN_POINT ( 'NONE',  ( -3.515970705488605130, 17.06554576617236307, -1.500000000000000000 ) ) ;
#22192 = DIRECTION ( 'NONE',  ( -2.312964634635740689E-15, 1.000000000000000000, 0.000000000000000000 ) ) ;
#22193 = CARTESIAN_POINT ( 'NONE',  ( -30.53339558441486190, 7.800891647352838909, 39.24389099736758624 ) ) ;
#22194 = AXIS2_PLACEMENT_3D ( 'NONE', #12901, #6323, #15836 ) ;
#22195 = ORIENTED_EDGE ( 'NONE', *, *, #14950, .F. ) ;
#22196 = LINE ( 'NONE', #832, #8410 ) ;
#22197 = CARTESIAN_POINT ( 'NONE',  ( -70.00000000000000000, 70.00000000000000000, -92.50000000000000000 ) ) ;
#22198 =( NAMED_UNIT ( * ) SI_UNIT ( $, .STERADIAN. ) SOLID_ANGLE_UNIT ( ) );
#22199 = FACE_OUTER_BOUND ( 'NONE', #29086, .T. ) ;
#22200 = EDGE_LOOP ( 'NONE', ( #10387, #20035, #11856, #25032 ) ) ;
#22201 = EDGE_CURVE ( 'NONE', #17387, #4972, #484, .T. ) ;
#22202 = EDGE_CURVE ( 'NONE', #4883, #5400, #15341, .T. ) ;
#22203 = CARTESIAN_POINT ( 'NONE',  ( -9.085694127122227570, -14.40282604532831812, 20.12545155307891065 ) ) ;
#22204 = DIRECTION ( 'NONE',  ( 0.9898434871385290990, -0.1411469255096601816, 0.01695335921306606250 ) ) ;
#22205 = CARTESIAN_POINT ( 'NONE',  ( -6.495433978329088198, 18.93455902173411687, 5.810767894563978686 ) ) ;
#22206 = VECTOR ( 'NONE', #5650, 1000.000000000000000 ) ;
#22207 = CARTESIAN_POINT ( 'NONE',  ( 11.24508296785401917, -16.56092475412858533, 5.661398277488802755 ) ) ;
#22208 = CARTESIAN_POINT ( 'NONE',  ( 10.11202017158399968, 41.14070756921128691, -1.500000000000000000 ) ) ;
#22209 = AXIS2_PLACEMENT_3D ( 'NONE', #12009, #4363, #11694 ) ;
#22210 = CARTESIAN_POINT ( 'NONE',  ( -50.00000000000000000, -50.00000000000000000, -92.50000000000000000 ) ) ;
#22211 = ORIENTED_EDGE ( 'NONE', *, *, #20437, .T. ) ;
#22212 = VERTEX_POINT ( 'NONE', #8449 ) ;
#22213 = CARTESIAN_POINT ( 'NONE',  ( 0.07661102881317785607, -6.914460432017389024, -6.023803224821256741 ) ) ;
#22214 = CARTESIAN_POINT ( 'NONE',  ( -8.099370871114970782, -15.01721251069485596, 7.545655578832109356 ) ) ;
#22215 = CARTESIAN_POINT ( 'NONE',  ( -14.70245401545669139, 13.58508552794529223, 6.420335371522007506 ) ) ;
#22216 = CARTESIAN_POINT ( 'NONE',  ( 69.99999999999998579, -70.00000000000000000, -92.50000000000000000 ) ) ;
#22217 = ORIENTED_EDGE ( 'NONE', *, *, #16064, .T. ) ;
#22218 = ITEM_DEFINED_TRANSFORMATION ( 'NONE', 'NONE', #30805,  #7396 ) ;
#22219 = DIRECTION ( 'NONE',  ( 0.000000000000000000, 0.000000000000000000, 1.000000000000000000 ) ) ;
#22220 = VECTOR ( 'NONE', #21310, 1000.000000000000000 ) ;
#22221 = DIRECTION ( 'NONE',  ( 0.000000000000000000, 0.000000000000000000, -1.000000000000000000 ) ) ;
#22222 = VERTEX_POINT ( 'NONE', #22611 ) ;
#22223 = DIRECTION ( 'NONE',  ( 0.000000000000000000, 0.000000000000000000, 1.000000000000000000 ) ) ;
#22224 = CARTESIAN_POINT ( 'NONE',  ( 0.5590800469813690388, -5.620102221249836383, 8.265697409064610923 ) ) ;
#22225 = CARTESIAN_POINT ( 'NONE',  ( -33.31528697581643428, -22.10504849272555106, 30.86792493716536612 ) ) ;
#22226 = ORIENTED_EDGE ( 'NONE', *, *, #20586, .T. ) ;
#22227 = LINE ( 'NONE', #5547, #24316 ) ;
#22228 = AXIS2_PLACEMENT_3D ( 'NONE', #28224, #14175, #26191 ) ;
#22229 = CIRCLE ( 'NONE', #810, 1.000000000000009548 ) ;
#22230 = DIRECTION ( 'NONE',  ( 1.000000000000000000, 0.000000000000000000, 0.000000000000000000 ) ) ;
#22231 = VECTOR ( 'NONE', #5663, 1000.000000000000000 ) ;
#22232 = FACE_OUTER_BOUND ( 'NONE', #4593, .T. ) ;
#22233 = DIRECTION ( 'NONE',  ( 0.1423148382732889183, 0.9898214418809321291, 0.000000000000000000 ) ) ;
#22234 = ORIENTED_EDGE ( 'NONE', *, *, #29756, .T. ) ;
#22235 = DIRECTION ( 'NONE',  ( 0.000000000000000000, 1.000000000000000000, 0.000000000000000000 ) ) ;
#22236 = CARTESIAN_POINT ( 'NONE',  ( 13.01350570279883634, 10.97146294988705506, 19.41069149716887310 ) ) ;
#22237 = DIRECTION ( 'NONE',  ( 0.000000000000000000, 0.000000000000000000, 1.000000000000000000 ) ) ;
#22238 = VECTOR ( 'NONE', #28617, 1000.000000000000000 ) ;
#22239 = CARTESIAN_POINT ( 'NONE',  ( -40.57664911653668582, 0.2791883433268081416, -16.50000000000000000 ) ) ;
#22241 = EDGE_CURVE ( 'NONE', #6747, #3010, #23314, .T. ) ;
#22240 = CARTESIAN_POINT ( 'NONE',  ( 0.000000000000000000, 0.000000000000000000, -1.500000000000000000 ) ) ;
#22242 = CARTESIAN_POINT ( 'NONE',  ( 35.28464582062836996, -18.14901843200646425, 8.522369028210444952 ) ) ;
#22243 = CIRCLE ( 'NONE', #23716, 20.00000000000000000 ) ;
#22244 = DIRECTION ( 'NONE',  ( 0.000000000000000000, 0.000000000000000000, -1.000000000000000000 ) ) ;
#22245 = EDGE_LOOP ( 'NONE', ( #16113, #11666, #26544, #11469 ) ) ;
#22246 = DIRECTION ( 'NONE',  ( -1.000000000000000000, 0.000000000000000000, 0.000000000000000000 ) ) ;
#22247 = DIRECTION ( 'NONE',  ( 0.000000000000000000, 0.000000000000000000, 1.000000000000000000 ) ) ;
#22248 = EDGE_LOOP ( 'NONE', ( #29890, #15777, #21884, #13332 ) ) ;
#22249 = VERTEX_POINT ( 'NONE', #29645 ) ;
#22250 = CIRCLE ( 'NONE', #15775, 9.482273699623480212 ) ;
#22251 = DIRECTION ( 'NONE',  ( -0.000000000000000000, -0.000000000000000000, -1.000000000000000000 ) ) ;
#22252 = CARTESIAN_POINT ( 'NONE',  ( 1.837104849652355830E-15, 50.00000000000000000, -70.00000000000000000 ) ) ;
#22253 = VECTOR ( 'NONE', #29270, 1000.000000000000000 ) ;
#22254 =( NAMED_UNIT ( * ) SI_UNIT ( $, .STERADIAN. ) SOLID_ANGLE_UNIT ( ) );
#22255 = AXIS2_PLACEMENT_3D ( 'NONE', #21545, #17027, #180 ) ;
#22256 = CARTESIAN_POINT ( 'NONE',  ( -6.804986885018592169, -38.79337642873097991, 27.50000000000000355 ) ) ;
#22257 = CARTESIAN_POINT ( 'NONE',  ( 12.77210943289887801, 11.26383436979580566, 18.55820869691756769 ) ) ;
#22258 = VERTEX_POINT ( 'NONE', #10614 ) ;
#22259 = CARTESIAN_POINT ( 'NONE',  ( -16.81771903218351838, 2.627522578025005107, 6.864725433338323413 ) ) ;
#22260 = CARTESIAN_POINT ( 'NONE',  ( 19.65054205152828004, 3.817440173033144202, 20.13759033520874908 ) ) ;
#22261 = CARTESIAN_POINT ( 'NONE',  ( 0.000000000000000000, 0.000000000000000000, 0.000000000000000000 ) ) ;
#22262 = ORIENTED_EDGE ( 'NONE', *, *, #23330, .F. ) ;
#22263 = CARTESIAN_POINT ( 'NONE',  ( -4.580173031745207624, 16.39361746661297659, 19.47784884541372818 ) ) ;
#22264 = ORIENTED_EDGE ( 'NONE', *, *, #28051, .T. ) ;
#22265 = CARTESIAN_POINT ( 'NONE',  ( -16.89565484000427986, 2.154541803992424231, 20.22273502201483453 ) ) ;
#22266 = AXIS2_PLACEMENT_3D ( 'NONE', #30745, #9232, #16709 ) ;
#22267 = ORIENTED_EDGE ( 'NONE', *, *, #12007, .F. ) ;
#22268 = CARTESIAN_POINT ( 'NONE',  ( 14.89790177301713392, 39.30146707257869565, 29.12506352215398664 ) ) ;
#22269 = CARTESIAN_POINT ( 'NONE',  ( 16.55580462840120504, 4.191719245021451101, 6.782048567692550378 ) ) ;
#22270 = LINE ( 'NONE', #15715, #2655 ) ;
#22271 = AXIS2_PLACEMENT_3D ( 'NONE', #29785, #18080, #6222 ) ;
#22272 = CARTESIAN_POINT ( 'NONE',  ( 0.7788148816922453310, -17.02744011591805062, 7.652108011868850923 ) ) ;
#22273 = CARTESIAN_POINT ( 'NONE',  ( -29.04471618533923305, -28.48400268535028346, 30.20750335454674129 ) ) ;
#22274 = CARTESIAN_POINT ( 'NONE',  ( 8.743977807160074889, 3.668292057956028973, 1.500000000000001332 ) ) ;
#22275 = EDGE_CURVE ( 'NONE', #7455, #18044, #29290, .T. ) ;
#22276 = CARTESIAN_POINT ( 'NONE',  ( -29.61203839202723032, -15.40012917324033381, 37.38016955275590192 ) ) ;
#22277 = ORIENTED_EDGE ( 'NONE', *, *, #2103, .F. ) ;
#22278 = CIRCLE ( 'NONE', #8845, 0.7500000000000006661 ) ;
#22279 = CARTESIAN_POINT ( 'NONE',  ( 10.28124378133233741, -17.17592898829030901, 6.864725433338323413 ) ) ;
#22280 = CARTESIAN_POINT ( 'NONE',  ( -30.69494854373527915, 26.21875054186513054, 8.554645101623277625 ) ) ;
#22281 = DIRECTION ( 'NONE',  ( 0.000000000000000000, -0.4961389383568337030, 0.8682431421244592995 ) ) ;
#22282 = AXIS2_PLACEMENT_3D ( 'NONE', #2180, #21502, #12320 ) ;
#22283 = ORIENTED_EDGE ( 'NONE', *, *, #25507, .T. ) ;
#22284 = EDGE_LOOP ( 'NONE', ( #12693, #8103, #15573, #16738, #25966, #3132 ) ) ;
#22285 = FACE_OUTER_BOUND ( 'NONE', #30387, .T. ) ;
#22286 = CLOSED_SHELL ( 'NONE', ( #5204, #12661, #15057, #7641, #4429, #9409, #23119, #18351, #787, #23423, #9394, #12227, #6, #5032, #5730, #24703, #1200, #10735, #29375, #3701, #8471, #29010 ) ) ;
#22287 = CARTESIAN_POINT ( 'NONE',  ( 18.64396409872438198, -7.239577540284320989, 19.96797677718664232 ) ) ;
#22288 = ORIENTED_EDGE ( 'NONE', *, *, #15674, .F. ) ;
#22289 = CARTESIAN_POINT ( 'NONE',  ( 0.000000000000000000, 1.699320956058915452E-16, -1.500000000000001776 ) ) ;
#22290 = CIRCLE ( 'NONE', #6835, 9.084132297865673777 ) ;
#22291 = DIRECTION ( 'NONE',  ( 0.000000000000000000, -1.000000000000000000, 0.000000000000000000 ) ) ;
#22292 = CIRCLE ( 'NONE', #10845, 0.7500000000000011102 ) ;
#22293 = DIRECTION ( 'NONE',  ( -1.000000000000000000, 0.000000000000000000, 0.000000000000000000 ) ) ;
#22294 = EDGE_LOOP ( 'NONE', ( #6083, #17994 ) ) ;
#22295 = B_SPLINE_CURVE_WITH_KNOTS ( 'NONE', 3,
 ( #25887, #4978, #30558, #28218, #6698, #25730, #19023, #26187, #2487, #11690, #139, #19168, #16678, #7010, #9658, #30702 ),
 .UNSPECIFIED., .F., .F.,
 ( 4, 2, 2, 2, 2, 2, 2, 4 ),
 ( 0.4999999999999998890, 0.6250000000000012212, 0.6875000000000019984, 0.7187500000000022204, 0.7500000000000026645, 0.8125000000000017764, 0.8750000000000007772, 1.000000000000000000 ),
 .UNSPECIFIED. ) ;
#22296 = AXIS2_PLACEMENT_3D ( 'NONE', #18637, #15988, #6768 ) ;
#22297 = DIRECTION ( 'NONE',  ( 1.000000000000000000, 0.000000000000000000, 0.000000000000000000 ) ) ;
#22298 = CARTESIAN_POINT ( 'NONE',  ( -3.395021109945016491, -30.50000000000000355, 1.500000000000000000 ) ) ;
#22299 = CARTESIAN_POINT ( 'NONE',  ( 19.89647750965486495, 2.201534687727673578, 6.530762810602277924 ) ) ;
#22300 = EDGE_LOOP ( 'NONE', ( #26284, #19275, #21881, #10595 ) ) ;
#22301 = CARTESIAN_POINT ( 'NONE',  ( 12.82328378257164836, 11.20259424400691195, 5.940635272151477686 ) ) ;
#22302 = ORIENTED_EDGE ( 'NONE', *, *, #10961, .T. ) ;
#22303 = AXIS2_PLACEMENT_3D ( 'NONE', #24358, #3004, #12522 ) ;
#22304 = CARTESIAN_POINT ( 'NONE',  ( -25.64627119138473432, -23.40052582045089480, -6.500000000000000888 ) ) ;
#22305 = CARTESIAN_POINT ( 'NONE',  ( 32.14097302481091134, -14.40131566728160273, 35.53783135158875695 ) ) ;
#22306 = VERTEX_POINT ( 'NONE', #15274 ) ;
#22307 = EDGE_CURVE ( 'NONE', #6254, #14731, #1260, .T. ) ;
#22308 = CARTESIAN_POINT ( 'NONE',  ( 25.23756106473024019, 11.43858098102958287, -16.50000000000000000 ) ) ;
#22309 = EDGE_CURVE ( 'NONE', #22753, #6144, #9230, .T. ) ;
#22310 = DIRECTION ( 'NONE',  ( -1.000000000000000000, 0.000000000000000000, 0.000000000000000000 ) ) ;
#22311 = DIRECTION ( 'NONE',  ( 0.000000000000000000, 0.000000000000000000, -1.000000000000000000 ) ) ;
#22312 = CARTESIAN_POINT ( 'NONE',  ( 15.63826127963997870, 35.59355150539998647, 34.50000000000000000 ) ) ;
#22313 = VECTOR ( 'NONE', #14125, 1000.000000000000000 ) ;
#22314 = ADVANCED_FACE ( 'NONE', ( #24956 ), #3594, .F. ) ;
#22315 = CIRCLE ( 'NONE', #10861, 0.7500000000000006661 ) ;
#22316 = CARTESIAN_POINT ( 'NONE',  ( -2.338573377552018773, 39.50000000000000711, 27.50000000000000355 ) ) ;
#22317 = CARTESIAN_POINT ( 'NONE',  ( 10.30179067644846747, -17.16362715220463642, 19.66989035740801839 ) ) ;
#22318 = ADVANCED_FACE ( 'NONE', ( #24490 ), #17322, .F. ) ;
#22319 = CARTESIAN_POINT ( 'NONE',  ( 10.42970548045642332, -17.06546344489796851, 18.72886616302736940 ) ) ;
#22320 = ORIENTED_EDGE ( 'NONE', *, *, #24823, .T. ) ;
#22321 = EDGE_CURVE ( 'NONE', #21077, #8486, #12658, .T. ) ;
#22322 = DIRECTION ( 'NONE',  ( -0.000000000000000000, -0.000000000000000000, -1.000000000000000000 ) ) ;
#22323 = CARTESIAN_POINT ( 'NONE',  ( 8.860628911697515875, 8.184276679720483116, -1.500000000000000000 ) ) ;
#22324 = CARTESIAN_POINT ( 'NONE',  ( -15.76141475779637879, 12.34077778289585048, 18.56793045041961321 ) ) ;
#22325 = CARTESIAN_POINT ( 'NONE',  ( 33.47438960496221227, 10.94461781313380477, 35.53941315612136975 ) ) ;
#22326 = PLANE ( 'NONE',  #24855 ) ;
#22327 = ORIENTED_EDGE ( 'NONE', *, *, #16853, .F. ) ;
#22329 = EDGE_CURVE ( 'NONE', #2507, #24787, #11910, .T. ) ;
#22328 = CARTESIAN_POINT ( 'NONE',  ( 0.000000000000000000, -2.435693370351110282E-15, 21.50000000000000355 ) ) ;
#22330 = B_SPLINE_SURFACE_WITH_KNOTS ( 'NONE', 3, 1, ( 
 ( #9608, #30499 ),
 ( #25838, #14264 ),
 ( #2116, #28166 ),
 ( #14441, #25988 ),
 ( #21449, #6795 ),
 ( #11494, #1973 ),
 ( #23622, #16771 ),
 ( #4472, #23943 ),
 ( #2589, #12106 ),
 ( #2265, #11634 ),
 ( #13980, #21126 ),
 ( #20977, #30646 ),
 ( #23784, #9292 ),
 ( #4615, #9752 ),
 ( #4759, #18660 ),
 ( #18817, #26129 ),
 ( #28336, #6961 ),
 ( #16622, #14116 ),
 ( #91, #26287 ),
 ( #16471, #19117 ),
 ( #4924, #21602 ),
 ( #240, #28635 ),
 ( #25679, #30813 ),
 ( #7259, #11785 ),
 ( #21290, #9460 ),
 ( #18975, #19266 ),
 ( #28485, #6647 ),
 ( #7114, #16164 ),
 ( #4300, #13830 ),
 ( #27066, #2899 ),
 ( #21755, #697 ) ),
 .UNSPECIFIED., .F., .F., .F.,
 ( 4, 3, 3, 3, 3, 3, 3, 3, 3, 3, 4 ),
 ( 2, 2 ),
 ( 0.000000000000000000, 0.05425176834609633791, 0.1085332949128352958, 0.1623767749169382768, 0.2157504826133063158, 0.2688657508888171455, 0.3218907763505476360, 0.3749548578363336993, 0.4282048033836242107, 0.4818374082110501444, 0.4999999999131655715 ),
 ( 0.000000000000000000, 1.000000000000000000 ),
 .UNSPECIFIED. ) ;
#22331 = CYLINDRICAL_SURFACE ( 'NONE', #1394, 2.898871837527151829 ) ;
#22332 = DIRECTION ( 'NONE',  ( -0.000000000000000000, -0.000000000000000000, -1.000000000000000000 ) ) ;
#22333 = VECTOR ( 'NONE', #18954, 1000.000000000000000 ) ;
#22334 = CARTESIAN_POINT ( 'NONE',  ( 66.99999999999998579, 0.000000000000000000, 59.49999999999999289 ) ) ;
#22335 = ADVANCED_FACE ( 'NONE', ( #29493 ), #24805, .F. ) ;
#22336 = CARTESIAN_POINT ( 'NONE',  ( 77.99999999999998579, 42.50000000000000000, 27.50000000000000711 ) ) ;
#22337 = EDGE_CURVE ( 'NONE', #6070, #21841, #13414, .T. ) ;
#22338 = CARTESIAN_POINT ( 'NONE',  ( 15.37842778815315725, 39.08494192275733781, 34.54087420883106319 ) ) ;
#22339 = ORIENTED_EDGE ( 'NONE', *, *, #1199, .T. ) ;
#22340 = DIRECTION ( 'NONE',  ( -0.000000000000000000, 1.132880637372608986E-16, -1.000000000000000000 ) ) ;
#22341 = AXIS2_PLACEMENT_3D ( 'NONE', #28142, #16285, #25179 ) ;
#22342 = DIRECTION ( 'NONE',  ( 0.000000000000000000, 1.000000000000000000, 0.000000000000000000 ) ) ;
#22343 = ORIENTED_EDGE ( 'NONE', *, *, #12223, .F. ) ;
#22344 = ORIENTED_EDGE ( 'NONE', *, *, #4019, .T. ) ;
#22345 = DIRECTION ( 'NONE',  ( 0.000000000000000000, 0.000000000000000000, 1.000000000000000000 ) ) ;
#22346 = ADVANCED_FACE ( 'NONE', ( #5264, #10092, #10242 ), #29339, .F. ) ;
#22347 = VERTEX_POINT ( 'NONE', #28825 ) ;
#22348 = CARTESIAN_POINT ( 'NONE',  ( -2.703030265324078307, -12.75514121382991384, 24.50000000000000000 ) ) ;
#22349 = EDGE_CURVE ( 'NONE', #25448, #30732, #24124, .T. ) ;
#22350 = AXIS2_PLACEMENT_3D ( 'NONE', #18973, #25985, #9138 ) ;
#22351 = CARTESIAN_POINT ( 'NONE',  ( -19.07766892062203468, 33.49890683909209343, 34.49999999999998579 ) ) ;
#22352 = ADVANCED_FACE ( 'NONE', ( #7762 ), #432, .F. ) ;
#22353 = DIRECTION ( 'NONE',  ( -0.000000000000000000, 1.132880637372608986E-16, -1.000000000000000000 ) ) ;
#22354 = AXIS2_PLACEMENT_3D ( 'NONE', #23763, #28616, #19410 ) ;
#22355 = CARTESIAN_POINT ( 'NONE',  ( 9.185733585337910512, -2.352830851074146246, 21.50000000000000000 ) ) ;
#22356 = DIRECTION ( 'NONE',  ( 0.000000000000000000, 0.000000000000000000, 1.000000000000000000 ) ) ;
#22357 = VECTOR ( 'NONE', #26155, 1000.000000000000000 ) ;
#22358 = EDGE_CURVE ( 'NONE', #11642, #498, #23840, .T. ) ;
#22359 = DIRECTION ( 'NONE',  ( 0.000000000000000000, 0.000000000000000000, 1.000000000000000000 ) ) ;
#22360 = DIRECTION ( 'NONE',  ( 1.000000000000000000, 0.000000000000000000, 0.000000000000000000 ) ) ;
#22361 = DIRECTION ( 'NONE',  ( 0.000000000000000000, 1.000000000000000000, 0.000000000000000000 ) ) ;
#22362 = CARTESIAN_POINT ( 'NONE',  ( 0.000000000000000000, 7.500000000000000000, -1.500000000000000444 ) ) ;
#22363 = EDGE_LOOP ( 'NONE', ( #15395, #29480, #4114, #20383 ) ) ;
#22364 = ADVANCED_FACE ( 'NONE', ( #29127 ), #7458, .F. ) ;
#22365 = AXIS2_PLACEMENT_3D ( 'NONE', #11179, #20832, #25980 ) ;
#22366 = CARTESIAN_POINT ( 'NONE',  ( -11.33306590618138543, -16.50086680533498296, 19.66989035740801839 ) ) ;
#22367 = DIRECTION ( 'NONE',  ( 0.000000000000000000, 0.000000000000000000, -1.000000000000000000 ) ) ;
#22368 = LINE ( 'NONE', #27371, #13082 ) ;
#22369 = CARTESIAN_POINT ( 'NONE',  ( 10.67336573878037775, -13.33112751634290127, 6.892848776733236704 ) ) ;
#22370 = EDGE_CURVE ( 'NONE', #21897, #10292, #11830, .T. ) ;
#22371 = CARTESIAN_POINT ( 'NONE',  ( -39.83602371821034183, 11.57901747687032490, -19.50000000000000355 ) ) ;
#22372 = AXIS2_PLACEMENT_3D ( 'NONE', #14069, #1923, #1772 ) ;
#22373 = CARTESIAN_POINT ( 'NONE',  ( -30.31220697679117393, 11.23460505553742550, 1.500000000000000000 ) ) ;
#22374 = VERTEX_POINT ( 'NONE', #13067 ) ;
#22375 = ORIENTED_EDGE ( 'NONE', *, *, #28026, .T. ) ;
#22376 = CARTESIAN_POINT ( 'NONE',  ( -31.89304216768361400, 14.79375299452194703, 35.60059606544055555 ) ) ;
#22377 = CARTESIAN_POINT ( 'NONE',  ( -35.76344986165608475, 22.29344514668535027, -19.50000000000000355 ) ) ;
#22378 = CARTESIAN_POINT ( 'NONE',  ( 5.965445004520304018, -42.10621517464141306, 34.60264052001484458 ) ) ;
#22379 = CARTESIAN_POINT ( 'NONE',  ( -0.1984805017666675109, -17.02075843868213667, 6.910395520694541993 ) ) ;
#22380 = ORIENTED_EDGE ( 'NONE', *, *, #29410, .T. ) ;
#22381 = CARTESIAN_POINT ( 'NONE',  ( -7.974144905643821168, -5.130938270761582487, 13.00000000000000178 ) ) ;
#22382 = CIRCLE ( 'NONE', #9911, 0.7441270634457163302 ) ;
#22383 = DIRECTION ( 'NONE',  ( 1.000000000000000000, 0.000000000000000000, 0.000000000000000000 ) ) ;
#22384 = EDGE_CURVE ( 'NONE', #11838, #16268, #27099, .T. ) ;
#22385 = VERTEX_POINT ( 'NONE', #22556 ) ;
#22386 = DIRECTION ( 'NONE',  ( 1.000000000000000000, 0.000000000000000000, 0.000000000000000000 ) ) ;
#22387 = EDGE_CURVE ( 'NONE', #7554, #21542, #18401, .T. ) ;
#22388 = AXIS2_PLACEMENT_3D ( 'NONE', #16615, #23777, #7419 ) ;
#22389 = DIRECTION ( 'NONE',  ( -0.000000000000000000, -0.000000000000000000, 1.000000000000000000 ) ) ;
#22390 = CARTESIAN_POINT ( 'NONE',  ( -37.12542188692624734, 5.327348916628460884, 37.50000000001456613 ) ) ;
#22391 = ORIENTED_EDGE ( 'NONE', *, *, #4468, .F. ) ;
#22392 = DIRECTION ( 'NONE',  ( 1.000000000000000000, 0.000000000000000000, 0.000000000000000000 ) ) ;
#22393 = DIRECTION ( 'NONE',  ( -0.000000000000000000, -0.000000000000000000, -1.000000000000000000 ) ) ;
#22394 = DIRECTION ( 'NONE',  ( 0.000000000000000000, 0.000000000000000000, 1.000000000000000000 ) ) ;
#22395 = CARTESIAN_POINT ( 'NONE',  ( -19.80925230797852876, 2.758332870380178825, 20.32243167357988511 ) ) ;
#22396 = ORIENTED_EDGE ( 'NONE', *, *, #21615, .F. ) ;
#22397 = CARTESIAN_POINT ( 'NONE',  ( 39.99999999999998579, 80.00000000000001421, 22.49999999999999289 ) ) ;
#22398 = CARTESIAN_POINT ( 'NONE',  ( -5.687793815610304726, 6.974883619896852238, 1.500000000000001332 ) ) ;
#22399 = DIRECTION ( 'NONE',  ( 0.000000000000000000, 0.000000000000000000, 1.000000000000000000 ) ) ;
#22400 = FACE_OUTER_BOUND ( 'NONE', #8381, .T. ) ;
#22401 = FACE_OUTER_BOUND ( 'NONE', #23747, .T. ) ;
#22402 = CARTESIAN_POINT ( 'NONE',  ( -65.00000000000000000, -70.00000000000000000, 12.49999999999999112 ) ) ;
#22403 = ORIENTED_EDGE ( 'NONE', *, *, #6894, .T. ) ;
#22404 = CARTESIAN_POINT ( 'NONE',  ( 36.00000000000000000, -1.546978760965586295E-11, 34.75735931288068059 ) ) ;
#22405 = AXIS2_PLACEMENT_3D ( 'NONE', #27453, #26483, #14012 ) ;
#22406 = LINE ( 'NONE', #28967, #26536 ) ;
#22407 = ORIENTED_EDGE ( 'NONE', *, *, #13184, .T. ) ;
#22408 = ORIENTED_EDGE ( 'NONE', *, *, #13012, .T. ) ;
#22409 = CARTESIAN_POINT ( 'NONE',  ( -11.40980092660686829, 6.310027164379044429, 1.500000000000001332 ) ) ;
#22410 = CARTESIAN_POINT ( 'NONE',  ( -6.062559277181930106, 5.881244434206302607, -1.500000000000000888 ) ) ;
#22411 = CARTESIAN_POINT ( 'NONE',  ( -7.523478279969216587, 49.43269233655315276, -67.98621439856492543 ) ) ;
#22412 =( GEOMETRIC_REPRESENTATION_CONTEXT ( 3 ) GLOBAL_UNCERTAINTY_ASSIGNED_CONTEXT ( ( #8936 ) ) GLOBAL_UNIT_ASSIGNED_CONTEXT ( ( #12715, #29240, #9600 ) ) REPRESENTATION_CONTEXT ( 'NONE', 'WORKASPACE' ) );
#22413 = CARTESIAN_POINT ( 'NONE',  ( -4.375757216953428294E-15, -39.50000000000000000, 27.50000000000000355 ) ) ;
#22414 = LINE ( 'NONE', #1057, #28116 ) ;
#22415 = EDGE_CURVE ( 'NONE', #11549, #26020, #22849, .T. ) ;
#22416 = ORIENTED_EDGE ( 'NONE', *, *, #11336, .F. ) ;
#22417 = ORIENTED_EDGE ( 'NONE', *, *, #6720, .F. ) ;
#22418 = FACE_OUTER_BOUND ( 'NONE', #5917, .T. ) ;
#22419 = CARTESIAN_POINT ( 'NONE',  ( 19.76130184095197961, 3.194145055459935101, 20.34789198813115263 ) ) ;
#22420 = DIRECTION ( 'NONE',  ( 1.000000000000000000, 0.000000000000000000, -0.000000000000000000 ) ) ;
#22421 = EDGE_LOOP ( 'NONE', ( #1016, #11385, #8939, #25989 ) ) ;
#22422 = DIRECTION ( 'NONE',  ( 0.000000000000000000, 0.000000000000000000, -1.000000000000000000 ) ) ;
#22423 = ORIENTED_EDGE ( 'NONE', *, *, #27078, .T. ) ;
#22424 = CARTESIAN_POINT ( 'NONE',  ( 39.99999999999998579, 80.00000000000001421, 52.49999999999999289 ) ) ;
#22425 = VERTEX_POINT ( 'NONE', #11027 ) ;
#22426 = PRESENTATION_STYLE_ASSIGNMENT (( #19942 ) ) ;
#22427 = CARTESIAN_POINT ( 'NONE',  ( 34.59464071930022300, -19.79227917861567221, 31.10398916234817079 ) ) ;
#22428 = CARTESIAN_POINT ( 'NONE',  ( 19.63091490780798409, 3.916522693408249545, 5.951255046771932733 ) ) ;
#22429 = CARTESIAN_POINT ( 'NONE',  ( -70.00000000000000000, 70.00000000000000000, 12.49999999999999112 ) ) ;
#22430 = CYLINDRICAL_SURFACE ( 'NONE', #13766, 2.061368542273053883 ) ;
#22431 = CARTESIAN_POINT ( 'NONE',  ( -38.39051948279409743, 7.594952977269135097, 32.04396099389172292 ) ) ;
#22432 = CARTESIAN_POINT ( 'NONE',  ( 2.168404344971008868E-16, 30.50000000000000000, 24.50000000000000000 ) ) ;
#22433 = FACE_BOUND ( 'NONE', #19791, .T. ) ;
#22434 = VERTEX_POINT ( 'NONE', #20217 ) ;
#22435 = CARTESIAN_POINT ( 'NONE',  ( 9.138492726993304061, -14.36378254522092135, 6.111214848085761986 ) ) ;
#22436 = CARTESIAN_POINT ( 'NONE',  ( 11.56680498864186291, -16.33760111733343123, 18.50655187082627862 ) ) ;
#22437 = DIRECTION ( 'NONE',  ( -0.4539545692076750738, -0.8910248307962433945, 0.000000000000000000 ) ) ;
#22438 = ORIENTED_EDGE ( 'NONE', *, *, #25431, .F. ) ;
#22439 = ORIENTED_EDGE ( 'NONE', *, *, #9612, .T. ) ;
#22440 = CARTESIAN_POINT ( 'NONE',  ( 0.000000000000000000, 0.000000000000000000, -1.500000000000000000 ) ) ;
#22441 = LINE ( 'NONE', #10127, #19094 ) ;
#22442 = CARTESIAN_POINT ( 'NONE',  ( -5.978582851986702806, 19.10413308555694911, 5.652196082367002106 ) ) ;
#22443 = ORIENTED_EDGE ( 'NONE', *, *, #2711, .F. ) ;
#22444 = FACE_OUTER_BOUND ( 'NONE', #24104, .T. ) ;
#22445 = PLANE ( 'NONE',  #26628 ) ;
#22446 = DIRECTION ( 'NONE',  ( -0.000000000000000000, -0.000000000000000000, 1.000000000000000000 ) ) ;
#22447 = ORIENTED_EDGE ( 'NONE', *, *, #23082, .T. ) ;
#22448 = LINE ( 'NONE', #13264, #21184 ) ;
#22449 = CARTESIAN_POINT ( 'NONE',  ( -37.99999999999999289, 70.00000000000000000, -69.49999999999998579 ) ) ;
#22450 = CARTESIAN_POINT ( 'NONE',  ( 19.89475757678375345, 2.217009531549524848, 6.864725433338323413 ) ) ;
#22451 = ORIENTED_EDGE ( 'NONE', *, *, #26013, .F. ) ;
#22452 = DIRECTION ( 'NONE',  ( 1.000000000000000000, 0.000000000000000000, 0.000000000000000000 ) ) ;
#22453 = ORIENTED_EDGE ( 'NONE', *, *, #6134, .T. ) ;
#22454 = CARTESIAN_POINT ( 'NONE',  ( -13.71336669116180929, 10.15199454966009718, 18.45571264222803975 ) ) ;
#22455 = CARTESIAN_POINT ( 'NONE',  ( 29.61203839202725518, -15.40012917324033381, 37.38016955275580244 ) ) ;
#22456 = ORIENTED_EDGE ( 'NONE', *, *, #10664, .T. ) ;
#22457 = DIRECTION ( 'NONE',  ( -0.000000000000000000, -0.000000000000000000, -1.000000000000000000 ) ) ;
#22458 = CIRCLE ( 'NONE', #1551, 15.00000000000000000 ) ;
#22459 = CARTESIAN_POINT ( 'NONE',  ( 33.55239377822428537, 10.10392708029668185, 39.95942412019666534 ) ) ;
#22460 = CARTESIAN_POINT ( 'NONE',  ( 14.73074142449663881, 5.627958522269738140, 1.500000000000001332 ) ) ;
#22461 = CIRCLE ( 'NONE', #18985, 23.20393738267342698 ) ;
#22462 = CARTESIAN_POINT ( 'NONE',  ( -28.55068628633582861, 24.19494186940698199, 34.80090346875805096 ) ) ;
#22463 = DIRECTION ( 'NONE',  ( 1.000000000000000000, 0.000000000000000000, 0.000000000000000000 ) ) ;
#22464 = CARTESIAN_POINT ( 'NONE',  ( -2.195509399283147268E-15, 7.573738413550469062, -4.881900264494495545 ) ) ;
#22465 = ORIENTED_EDGE ( 'NONE', *, *, #20633, .F. ) ;
#22466 = CARTESIAN_POINT ( 'NONE',  ( -40.00000000000000000, 87.00000000000001421, 15.49999999999998934 ) ) ;
#22467 = CARTESIAN_POINT ( 'NONE',  ( -15.69442553397267304, 12.42550873695622826, 20.19593175699879595 ) ) ;
#22468 = CARTESIAN_POINT ( 'NONE',  ( 1.000000000000008438, 17.23749217771910480, 24.50000000000000000 ) ) ;
#22469 = DIRECTION ( 'NONE',  ( 0.000000000000000000, 0.000000000000000000, 1.000000000000000000 ) ) ;
#22470 = ORIENTED_EDGE ( 'NONE', *, *, #19009, .F. ) ;
#22471 = CARTESIAN_POINT ( 'NONE',  ( -8.090471615930056259, 1.687027447297517080, -3.621320343559650379 ) ) ;
#22472 = CARTESIAN_POINT ( 'NONE',  ( -40.49689208720899813, 64.44504373098514804, 62.50000000000000000 ) ) ;
#22473 = B_SPLINE_CURVE_WITH_KNOTS ( 'NONE', 3,
 ( #11219, #21021, #18093, #18553, #3748, #6394, #13267, #1414, #20431, #25423, #8588, #4049, #8891, #18415 ),
 .UNSPECIFIED., .F., .F.,
 ( 4, 2, 2, 2, 2, 2, 4 ),
 ( 2.111164903073641426E-07, 0.0004668847526555942461, 0.0009335583888208811134, 0.001400232024986168035, 0.001866905661151454848, 0.002800252933482020451, 0.003733600205812585837 ),
 .UNSPECIFIED. ) ;
#22474 = CARTESIAN_POINT ( 'NONE',  ( -25.47847050916410439, -26.57182937991348481, -1.500000000000001332 ) ) ;
#22475 = CARTESIAN_POINT ( 'NONE',  ( -49.99999999999998579, 209.2686044187655909, -75.50000000000002842 ) ) ;
#22476 = CYLINDRICAL_SURFACE ( 'NONE', #11637, 3.000000000000002665 ) ;
#22477 = EDGE_CURVE ( 'NONE', #11031, #7019, #27248, .T. ) ;
#22478 = LINE ( 'NONE', #3157, #24856 ) ;
#22479 = ORIENTED_EDGE ( 'NONE', *, *, #27895, .T. ) ;
#22480 = VECTOR ( 'NONE', #164, 1000.000000000000000 ) ;
#22481 = CARTESIAN_POINT ( 'NONE',  ( 25.41654339919795902, 6.509636863629522097, 44.52079389600188364 ) ) ;
#22482 = ORIENTED_EDGE ( 'NONE', *, *, #29793, .F. ) ;
#22483 = CARTESIAN_POINT ( 'NONE',  ( -1.000000000000008438, 13.00000000000001421, 1.500000000000001332 ) ) ;
#22484 = DIRECTION ( 'NONE',  ( 1.000000000000000000, 0.000000000000000000, 0.000000000000000000 ) ) ;
#22485 = ORIENTED_EDGE ( 'NONE', *, *, #10728, .T. ) ;
#22486 = ORIENTED_EDGE ( 'NONE', *, *, #30503, .F. ) ;
#22487 = DIRECTION ( 'NONE',  ( 0.000000000000000000, 0.000000000000000000, 1.000000000000000000 ) ) ;
#22488 = EDGE_CURVE ( 'NONE', #2369, #2413, #1776, .T. ) ;
#22489 = CARTESIAN_POINT ( 'NONE',  ( 12.24063095261064404, 4.490763173670002217, 24.50000000000000000 ) ) ;
#22490 = ORIENTED_EDGE ( 'NONE', *, *, #11319, .T. ) ;
#22491 = DIRECTION ( 'NONE',  ( 0.000000000000000000, 0.000000000000000000, 1.000000000000000000 ) ) ;
#22492 = CARTESIAN_POINT ( 'NONE',  ( 4.852933661107258878, 49.77225640444542876, -69.22700773620653081 ) ) ;
#22493 = CIRCLE ( 'NONE', #29485, 0.7500000000000006661 ) ;
#22494 = CARTESIAN_POINT ( 'NONE',  ( 19.18576292979354747, 22.55620591602726677, 1.500000000000000000 ) ) ;
#22495 = CARTESIAN_POINT ( 'NONE',  ( -37.68080749674851404, 10.96349481065684017, 11.26294974525756132 ) ) ;
#22496 = EDGE_CURVE ( 'NONE', #3349, #16393, #9894, .T. ) ;
#22497 = CARTESIAN_POINT ( 'NONE',  ( -40.00000000000002842, 80.00000000000001421, 47.50000000000014921 ) ) ;
#22498 = ADVANCED_FACE ( 'NONE', ( #20382 ), #3545, .F. ) ;
#22499 = PLANE ( 'NONE',  #20835 ) ;
#22500 = DIRECTION ( 'NONE',  ( -0.000000000000000000, -0.000000000000000000, 1.000000000000000000 ) ) ;
#22501 = CARTESIAN_POINT ( 'NONE',  ( 12.13430697852916929, 11.98518526348621016, 20.29915277494337644 ) ) ;
#22502 = DIRECTION ( 'NONE',  ( -0.000000000000000000, 0.000000000000000000, 1.000000000000000000 ) ) ;
#22503 = ORIENTED_EDGE ( 'NONE', *, *, #5526, .T. ) ;
#22504 = AXIS2_PLACEMENT_3D ( 'NONE', #8559, #28175, #6806 ) ;
#22505 = DIRECTION ( 'NONE',  ( 0.000000000000000000, -1.000000000000000000, 0.000000000000000000 ) ) ;
#22506 = CARTESIAN_POINT ( 'NONE',  ( -4.604861147465549642, 16.38721654675108752, 6.910395520694541993 ) ) ;
#22507 = CARTESIAN_POINT ( 'NONE',  ( 11.71757112412214141, -16.22992597261980308, 5.951255046771932733 ) ) ;
#22508 = CARTESIAN_POINT ( 'NONE',  ( -67.00000000000000000, 50.00000000000000000, 59.49999999999999289 ) ) ;
#22509 = LINE ( 'NONE', #8510, #19586 ) ;
#22510 = VERTEX_POINT ( 'NONE', #15384 ) ;
#22511 = ORIENTED_EDGE ( 'NONE', *, *, #24384, .F. ) ;
#22512 = CARTESIAN_POINT ( 'NONE',  ( -30.03865005752670214, 15.52610542268208604, 36.94359686637174178 ) ) ;
#22513 = CARTESIAN_POINT ( 'NONE',  ( 2.552544031601107211, 42.49999999998228617, -1.500000000000000000 ) ) ;
#22514 = ADVANCED_FACE ( 'NONE', ( #24909 ), #8385, .F. ) ;
#22515 = CARTESIAN_POINT ( 'NONE',  ( -12.72607405277288350, 11.30422146305940245, 6.420335371522007506 ) ) ;
#22516 = ADVANCED_FACE ( 'NONE', ( #15542 ), #22867, .F. ) ;
#22518 = VECTOR ( 'NONE', #10986, 1000.000000000000000 ) ;
#22517 = DIRECTION ( 'NONE',  ( -0.000000000000000000, -0.000000000000000000, 1.000000000000000000 ) ) ;
#22519 = ORIENTED_EDGE ( 'NONE', *, *, #4207, .T. ) ;
#22520 = CARTESIAN_POINT ( 'NONE',  ( 3.794966104506363180, 16.62713903699921048, 7.652108011868852699 ) ) ;
#22521 = EDGE_CURVE ( 'NONE', #25063, #19467, #12918, .T. ) ;
#22522 = CARTESIAN_POINT ( 'NONE',  ( 32.74775157612609178, -27.21557300919356948, -19.50000000000000355 ) ) ;
#22523 = CARTESIAN_POINT ( 'NONE',  ( -8.925879454855033757, -14.50801274514188677, 7.557577766377196582 ) ) ;
#22524 = EDGE_LOOP ( 'NONE', ( #11097, #23684, #17577, #28601 ) ) ;
#22525 = CARTESIAN_POINT ( 'NONE',  ( 5.721595087358985587, 19.18273663903466897, 18.44501272782439827 ) ) ;
#22526 = EDGE_CURVE ( 'NONE', #26251, #17832, #9412, .T. ) ;
#22527 = LINE ( 'NONE', #17874, #4353 ) ;
#22528 = CARTESIAN_POINT ( 'NONE',  ( -4.272706734768129344, -37.25579118954082247, 37.50000000000000000 ) ) ;
#22529 = ORIENTED_EDGE ( 'NONE', *, *, #24076, .F. ) ;
#22530 = EDGE_CURVE ( 'NONE', #24759, #8522, #11509, .T. ) ;
#22531 = CARTESIAN_POINT ( 'NONE',  ( 11.93826604606910990, -16.04611492155651575, 6.788986777570701570 ) ) ;
#22532 = EDGE_CURVE ( 'NONE', #4573, #27291, #18200, .T. ) ;
#22533 = CARTESIAN_POINT ( 'NONE',  ( -1.000000000000008438, 13.00000000000001421, 1.500000000000001332 ) ) ;
#22534 = LINE ( 'NONE', #27542, #1884 ) ;
#22535 = CARTESIAN_POINT ( 'NONE',  ( 6.899999999999999467, 5.196152422706634688, -9.000000000000001776 ) ) ;
#22536 = VERTEX_POINT ( 'NONE', #23327 ) ;
#22537 = DIRECTION ( 'NONE',  ( -1.000000000000000000, 0.000000000000000000, 0.000000000000000000 ) ) ;
#22538 = EDGE_CURVE ( 'NONE', #9741, #17647, #24864, .T. ) ;
#22539 = AXIS2_PLACEMENT_3D ( 'NONE', #28133, #16428, #2071 ) ;
#22540 = VECTOR ( 'NONE', #6088, 1000.000000000000000 ) ;
#22541 = SURFACE_STYLE_FILL_AREA ( #19741 ) ;
#22542 = CIRCLE ( 'NONE', #29528, 1.000000000000007772 ) ;
#22543 = CARTESIAN_POINT ( 'NONE',  ( 7.483314773547865784, 75.00000000000001421, 50.49999999999998579 ) ) ;
#22544 = CARTESIAN_POINT ( 'NONE',  ( -40.05520497409654013, 7.028746409781321702, -16.50000000000000000 ) ) ;
#22545 = CARTESIAN_POINT ( 'NONE',  ( -19.91398265452221850, -1.852915226174652208, 24.50000000000000000 ) ) ;
#22546 = DIRECTION ( 'NONE',  ( 1.000000000000000000, 0.000000000000000000, 0.000000000000000000 ) ) ;
#22547 = CARTESIAN_POINT ( 'NONE',  ( -20.00000000000004263, 1.387778780781445676E-14, 24.50000000000000000 ) ) ;
#22548 = ORIENTED_EDGE ( 'NONE', *, *, #27123, .F. ) ;
#22549 = CARTESIAN_POINT ( 'NONE',  ( 32.89824568090541845, -8.841523719485385513, 40.93443584516763423 ) ) ;
#22550 = DIRECTION ( 'NONE',  ( -1.000000000000000000, 0.000000000000000000, 0.000000000000000000 ) ) ;
#22551 = EDGE_LOOP ( 'NONE', ( #3115, #26591, #27216, #10104 ) ) ;
#22552 = VERTEX_POINT ( 'NONE', #1966 ) ;
#22553 = DIRECTION ( 'NONE',  ( -0.000000000000000000, -0.000000000000000000, 1.000000000000000000 ) ) ;
#22554 = CARTESIAN_POINT ( 'NONE',  ( 39.83602371821015709, 11.57901747687536265, -19.50000000000000355 ) ) ;
#22555 = EDGE_CURVE ( 'NONE', #4126, #886, #6912, .T. ) ;
#22556 = CARTESIAN_POINT ( 'NONE',  ( -6.301234758012551396, 6.543385983536412986, -1.500000000000001110 ) ) ;
#22557 = EDGE_CURVE ( 'NONE', #24466, #14711, #949, .T. ) ;
#22558 = ORIENTED_EDGE ( 'NONE', *, *, #8811, .F. ) ;
#22559 = PLANE ( 'NONE',  #23835 ) ;
#22560 = EDGE_CURVE ( 'NONE', #8734, #2233, #6792, .T. ) ;
#22561 = DIRECTION ( 'NONE',  ( 1.000000000000000000, 0.000000000000000000, 0.000000000000000000 ) ) ;
#22562 = AXIS2_PLACEMENT_3D ( 'NONE', #13319, #20923, #25316 ) ;
#22563 = ORIENTED_EDGE ( 'NONE', *, *, #25169, .T. ) ;
#22564 = AXIS2_PLACEMENT_3D ( 'NONE', #2066, #26084, #16725 ) ;
#22565 = CARTESIAN_POINT ( 'NONE',  ( -19.84651427434117821, 2.615565199888951309, 7.652108011868850035 ) ) ;
#22566 = CARTESIAN_POINT ( 'NONE',  ( 16.66826434373539811, 3.628879393376897244, 20.25542030744407640 ) ) ;
#22567 = CARTESIAN_POINT ( 'NONE',  ( 15.21635490854752781, 12.97988522761634478, 7.526993102356318133 ) ) ;
#22568 = FACE_BOUND ( 'NONE', #24756, .T. ) ;
#22569 = ORIENTED_EDGE ( 'NONE', *, *, #2266, .T. ) ;
#22570 = DIRECTION ( 'NONE',  ( -0.000000000000000000, -0.000000000000000000, 1.000000000000000000 ) ) ;
#22571 = EDGE_LOOP ( 'NONE', ( #4752, #28348, #26567, #16838, #1101 ) ) ;
#22572 = DIRECTION ( 'NONE',  ( 1.000000000000000000, 0.000000000000000000, 0.000000000000000000 ) ) ;
#22573 = ORIENTED_EDGE ( 'NONE', *, *, #17397, .T. ) ;
#22574 = CARTESIAN_POINT ( 'NONE',  ( -6.222613296526853688, 19.00773140132666938, 20.32200205377525393 ) ) ;
#22575 = CARTESIAN_POINT ( 'NONE',  ( -26.11179934312166395, 14.04991663536888780, 41.10667063058299675 ) ) ;
#22576 = CARTESIAN_POINT ( 'NONE',  ( 22.95669091611928181, 27.54300778121952575, 1.500000000000000000 ) ) ;
#22577 = CARTESIAN_POINT ( 'NONE',  ( 9.248129367672065726, 2.094186647214772989, 13.00000000000000178 ) ) ;
#22578 = VECTOR ( 'NONE', #12706, 1000.000000000000000 ) ;
#22579 = CARTESIAN_POINT ( 'NONE',  ( 1.767905995587313761, -16.98559759804296476, 6.917457548096558995 ) ) ;
#22580 = DIRECTION ( 'NONE',  ( 1.000000000000000000, 0.000000000000000000, -0.000000000000000000 ) ) ;
#22581 = CIRCLE ( 'NONE', #30075, 9.482273699623480212 ) ;
#22582 = CARTESIAN_POINT ( 'NONE',  ( -8.978548835163147501, -14.47379921348856868, 7.526951045817043884 ) ) ;
#22583 = DIRECTION ( 'NONE',  ( -0.000000000000000000, -0.000000000000000000, 1.000000000000000000 ) ) ;
#22584 = VERTEX_POINT ( 'NONE', #18813 ) ;
#22585 = EDGE_CURVE ( 'NONE', #9785, #28674, #11489, .T. ) ;
#22586 = AXIS2_PLACEMENT_3D ( 'NONE', #14347, #12328, #26364 ) ;
#22587 = LINE ( 'NONE', #17929, #20750 ) ;
#22588 = ADVANCED_FACE ( 'NONE', ( #25831 ), #20972, .F. ) ;
#22589 = CARTESIAN_POINT ( 'NONE',  ( -32.53389886252318774, 23.45533066602934724, 17.99999999999999645 ) ) ;
#22590 = CARTESIAN_POINT ( 'NONE',  ( -8.303920738747237351, -3.683253992019803746, -1.500000000000002220 ) ) ;
#22591 = ORIENTED_EDGE ( 'NONE', *, *, #26550, .F. ) ;
#22592 = ORIENTED_EDGE ( 'NONE', *, *, #10939, .T. ) ;
#22593 = DIRECTION ( 'NONE',  ( 0.9329908884337537733, -0.3598999890241659783, 0.000000000000000000 ) ) ;
#22594 = DIRECTION ( 'NONE',  ( 1.000000000000000000, 0.000000000000000000, 0.000000000000000000 ) ) ;
#22595 = CARTESIAN_POINT ( 'NONE',  ( -4.863253556059218496, 16.31819504766686890, 5.940635272151477686 ) ) ;
#22596 = ORIENTED_EDGE ( 'NONE', *, *, #13608, .T. ) ;
#22597 = LINE ( 'NONE', #10603, #29524 ) ;
#22598 = CARTESIAN_POINT ( 'NONE',  ( -3.000000000000041744, 1.387778780781445676E-14, 24.50000000000000000 ) ) ;
#22599 = CARTESIAN_POINT ( 'NONE',  ( -9.436481611552759219, -0.9307681286968260137, 1.500000000000001332 ) ) ;
#22600 = ORIENTED_EDGE ( 'NONE', *, *, #10325, .F. ) ;
#22601 = DIRECTION ( 'NONE',  ( 0.000000000000000000, -1.000000000000000000, 0.000000000000000000 ) ) ;
#22602 = CARTESIAN_POINT ( 'NONE',  ( 22.49999999999992184, 1.663324310589599759E-14, 62.49999999999999289 ) ) ;
#22603 = CARTESIAN_POINT ( 'NONE',  ( 16.82202058066697248, 2.664153601443037367, 5.796888747622817029 ) ) ;
#22604 = ORIENTED_EDGE ( 'NONE', *, *, #16117, .F. ) ;
#22605 = B_SPLINE_CURVE_WITH_KNOTS ( 'NONE', 3,
 ( #15145, #17501, #22168, #12981, #14840, #1278, #8147, #24355, #3151, #12676, #1119, #3002, #12520, #17180, #10318, #19834, #10631, #13134, #24826, #24661, #14994, #29359, #22628, #19526, #20144, #7682, #29191, #15296, #7998, #27171, #5332, #27021, #10478, #29661, #12827, #17816, #29039, #26702, #22012, #969, #27329, #26870, #647, #10162, #19991, #17654, #19670, #7831, #5493, #24506, #11407, #25129 ),
 .UNSPECIFIED., .F., .F.,
 ( 4, 2, 2, 2, 2, 2, 2, 2, 2, 2, 2, 2, 2, 2, 2, 2, 2, 2, 2, 2, 2, 2, 2, 2, 2, 4 ),
 ( 0.03093351381247303605, 0.03229139417284349750, 0.03364927453321395895, 0.03500715489358443427, 0.03636503525395490266, 0.03704397543414014726, 0.03772291561432539186, 0.03840185579451063647, 0.03908079597469588107, 0.03975973615488111873, 0.04043867633506636333, 0.04111761651525160793, 0.04179655669543684560, 0.04247549687562209020, 0.04315443705580733480, 0.04383337723599257940, 0.04451231741617782400, 0.04519125759636306167, 0.04587019777654829933, 0.04722807813691876078, 0.04790701831710400538, 0.04858595849728923610, 0.04994383885765971143, 0.05130171921803017288, 0.05198065939821540360, 0.05265959957840063432 ),
 .UNSPECIFIED. ) ;
#22606 = LINE ( 'NONE', #17480, #9335 ) ;
#22607 = VECTOR ( 'NONE', #11592, 1000.000000000000000 ) ;
#22608 = ORIENTED_EDGE ( 'NONE', *, *, #9581, .F. ) ;
#22609 = CARTESIAN_POINT ( 'NONE',  ( -13.88572908629245184, 9.930151408457417617, 19.96568007040468729 ) ) ;
#22610 = AXIS2_PLACEMENT_3D ( 'NONE', #26688, #5784, #15281 ) ;
#22611 = CARTESIAN_POINT ( 'NONE',  ( -57.50000000000001421, 50.00000000000000000, 12.49999999999999112 ) ) ;
#22612 = EDGE_LOOP ( 'NONE', ( #9801, #24515, #18456, #17041 ) ) ;
#22613 = VERTEX_POINT ( 'NONE', #8837 ) ;
#22614 = VECTOR ( 'NONE', #4881, 1000.000000000000000 ) ;
#22615 = CARTESIAN_POINT ( 'NONE',  ( 3.062389757841103677, 16.80148204205677587, 6.672349528511551497 ) ) ;
#22616 = DIRECTION ( 'NONE',  ( 0.000000000000000000, 0.000000000000000000, -1.000000000000000000 ) ) ;
#22617 = CARTESIAN_POINT ( 'NONE',  ( 5.296161872597624942, 19.28602264385379428, 20.34789198813115263 ) ) ;
#22618 = DIRECTION ( 'NONE',  ( -1.000000000000000000, 0.000000000000000000, 0.000000000000000000 ) ) ;
#22619 = FACE_OUTER_BOUND ( 'NONE', #13731, .T. ) ;
#22620 = CARTESIAN_POINT ( 'NONE',  ( 19.88037316481945282, 2.342382300094908665, 19.87181966307587544 ) ) ;
#22621 = EDGE_LOOP ( 'NONE', ( #18397, #11980, #10680, #23393 ) ) ;
#22622 = LINE ( 'NONE', #15930, #11747 ) ;
#22623 = CARTESIAN_POINT ( 'NONE',  ( 15.40995608898785107, -7.231564984717128830, 6.310736198168394928 ) ) ;
#22624 = CARTESIAN_POINT ( 'NONE',  ( -13.95900029477595439, 9.834024558217739909, 18.92976555901915603 ) ) ;
#22625 = CARTESIAN_POINT ( 'NONE',  ( 46.52886723831935711, 69.65281032693101793, 60.08552518507810447 ) ) ;
#22626 = ORIENTED_EDGE ( 'NONE', *, *, #9142, .T. ) ;
#22627 = EDGE_LOOP ( 'NONE', ( #1621, #3380, #21526, #27706 ) ) ;
#22628 = CARTESIAN_POINT ( 'NONE',  ( 28.06446820126206987, -29.51148668445827283, 12.10055096529683638 ) ) ;
#22629 = CYLINDRICAL_SURFACE ( 'NONE', #14118, 15.00000000000000000 ) ;
#22630 = CARTESIAN_POINT ( 'NONE',  ( -5.973960059363100150, 19.10558826632600216, 20.34789198813115263 ) ) ;
#22631 =( NAMED_UNIT ( * ) SI_UNIT ( $, .STERADIAN. ) SOLID_ANGLE_UNIT ( ) );
#22632 = CYLINDRICAL_SURFACE ( 'NONE', #20562, 1.000000000000008660 ) ;
#22633 = FACE_OUTER_BOUND ( 'NONE', #16221, .T. ) ;
#22634 = CARTESIAN_POINT ( 'NONE',  ( 16.87629972246965337, 2.221555249129149257, 6.385774490351134425 ) ) ;
#22635 = ORIENTED_EDGE ( 'NONE', *, *, #26339, .F. ) ;
#22636 = LINE ( 'NONE', #27344, #28938 ) ;
#22637 = CARTESIAN_POINT ( 'NONE',  ( -32.49060333908415288, 8.555881924488323520, 41.40175883617482100 ) ) ;
#22638 = DIRECTION ( 'NONE',  ( -0.000000000000000000, -0.000000000000000000, 1.000000000000000000 ) ) ;
#22639 = ORIENTED_EDGE ( 'NONE', *, *, #23113, .T. ) ;
#22640 = VERTEX_POINT ( 'NONE', #23470 ) ;
#22641 = CARTESIAN_POINT ( 'NONE',  ( -19.69217677393684696, 3.495450461901487671, 6.781503518395076036 ) ) ;
#22642 = DIRECTION ( 'NONE',  ( 0.000000000000000000, 0.000000000000000000, 1.000000000000000000 ) ) ;
#22643 = ORIENTED_EDGE ( 'NONE', *, *, #15654, .T. ) ;
#22644 = CARTESIAN_POINT ( 'NONE',  ( -0.6299556268942230197, -19.99014111075367595, 6.386539667786101937 ) ) ;
#22645 = VECTOR ( 'NONE', #15156, 1000.000000000000000 ) ;
#22646 = CARTESIAN_POINT ( 'NONE',  ( 7.944760815330115911, 49.36648745528790982, -67.73260676410613712 ) ) ;
#22647 = CARTESIAN_POINT ( 'NONE',  ( 1.073881485057758711, 0.9711784013061475207, 1.500000000000000000 ) ) ;
#22648 = CARTESIAN_POINT ( 'NONE',  ( -37.85956889627766486, 10.20476609408173552, 11.84522522745651862 ) ) ;
#22649 = CARTESIAN_POINT ( 'NONE',  ( -5.621668343899183462, 16.09410144477764604, 18.34838970509067479 ) ) ;
#22650 = CARTESIAN_POINT ( 'NONE',  ( -11.64054540341807353, 16.26338533980437262, 1.500000000000001332 ) ) ;
#22651 = DIRECTION ( 'NONE',  ( 0.000000000000000000, 0.000000000000000000, 1.000000000000000000 ) ) ;
#22652 = CARTESIAN_POINT ( 'NONE',  ( 14.79741041486972897, 13.48156734445488070, 20.33971507717571114 ) ) ;
#22653 = DIRECTION ( 'NONE',  ( 0.000000000000000000, 0.000000000000000000, 1.000000000000000000 ) ) ;
#22654 = ORIENTED_EDGE ( 'NONE', *, *, #8631, .F. ) ;
#22655 = AXIS2_PLACEMENT_3D ( 'NONE', #26881, #3011, #5502 ) ;
#22656 = CARTESIAN_POINT ( 'NONE',  ( -9.269489102446176076, -14.27959628656685886, 18.80699882434806369 ) ) ;
#22657 = LINE ( 'NONE', #1306, #19253 ) ;
#22658 = LINE ( 'NONE', #30453, #15037 ) ;
#22659 = CARTESIAN_POINT ( 'NONE',  ( 11.87672590887049573, -16.11366389249059594, 6.233981582756856987 ) ) ;
#22660 = EDGE_CURVE ( 'NONE', #12760, #30101, #27711, .T. ) ;
#22661 = CARTESIAN_POINT ( 'NONE',  ( 5.374868878255610660, 44.10336124695606230, -19.50000000000000355 ) ) ;
#22662 = CARTESIAN_POINT ( 'NONE',  ( 24.44496207165490631, -7.595930209050163029, -16.55003854064094426 ) ) ;
#22663 = ORIENTED_EDGE ( 'NONE', *, *, #12020, .T. ) ;
#22664 = EDGE_LOOP ( 'NONE', ( #27807, #3893, #23420, #21560 ) ) ;
#22665 = CARTESIAN_POINT ( 'NONE',  ( -30.50257113119998209, 15.54031451041691270, 36.52435908487349536 ) ) ;
#22666 = CARTESIAN_POINT ( 'NONE',  ( 34.07766914598172292, -21.40380666527112652, -1.500000000000000000 ) ) ;
#22667 = CARTESIAN_POINT ( 'NONE',  ( -3.741133385587110283, -42.33143344558632748, 28.85421604109468063 ) ) ;
#22668 = DIRECTION ( 'NONE',  ( 1.000000000000000000, 0.000000000000000000, 0.000000000000000000 ) ) ;
#22669 = ORIENTED_EDGE ( 'NONE', *, *, #18370, .T. ) ;
#22670 = DIRECTION ( 'NONE',  ( 1.000000000000000000, 4.440892098500625373E-15, 0.000000000000000000 ) ) ;
#22671 = CARTESIAN_POINT ( 'NONE',  ( 5.105024945674004222, 42.22604126506330857, -1.500000000000000000 ) ) ;
#22672 = CARTESIAN_POINT ( 'NONE',  ( -8.917851762035224894, -14.51287734179233802, 5.749228751562096562 ) ) ;
#22673 = ORIENTED_EDGE ( 'NONE', *, *, #23669, .T. ) ;
#22674 = CARTESIAN_POINT ( 'NONE',  ( -13.00999358272542494, -0.8602714556717691030, 1.500000000000001332 ) ) ;
#22675 = CARTESIAN_POINT ( 'NONE',  ( -5.433041902549405222, -37.12271733102753046, 37.49999999999359801 ) ) ;
#22676 = ORIENTED_EDGE ( 'NONE', *, *, #29297, .T. ) ;
#22677 = CARTESIAN_POINT ( 'NONE',  ( -4.622016212553093695, -12.19167610014704906, 24.50000000000000000 ) ) ;
#22678 = DIRECTION ( 'NONE',  ( -0.6707505147970128645, -0.7416830501633041584, 0.000000000000000000 ) ) ;
#22679 = CARTESIAN_POINT ( 'NONE',  ( 32.06827542805550735, -14.53851282002520406, 39.79035104390192146 ) ) ;
#22680 = CARTESIAN_POINT ( 'NONE',  ( -24.03448224033878944, 8.660042335149837456, 45.23564988763775574 ) ) ;
#22681 = ORIENTED_EDGE ( 'NONE', *, *, #4314, .T. ) ;
#22682 = CARTESIAN_POINT ( 'NONE',  ( 6.601643239663004076E-16, 42.50000000000000000, 28.83974596215562514 ) ) ;
#22683 = AXIS2_PLACEMENT_3D ( 'NONE', #16722, #21398, #24037 ) ;
#22684 = CARTESIAN_POINT ( 'NONE',  ( -8.456776945386934585E-15, 29.50000000000000000, 1.500000000000001332 ) ) ;
#22685 = EDGE_CURVE ( 'NONE', #23519, #23603, #13974, .T. ) ;
#22686 = FACE_OUTER_BOUND ( 'NONE', #11782, .T. ) ;
#22687 = EDGE_CURVE ( 'NONE', #6050, #2551, #25349, .T. ) ;
#22688 = LINE ( 'NONE', #1341, #22253 ) ;
#22689 = AXIS2_PLACEMENT_3D ( 'NONE', #29486, #10758, #24949 ) ;
#22690 = CARTESIAN_POINT ( 'NONE',  ( -16.99844672487172659, 1.385815296940135388, 5.653604225791664994 ) ) ;
#22691 = FACE_OUTER_BOUND ( 'NONE', #9041, .T. ) ;
#22692 = DIRECTION ( 'NONE',  ( 0.000000000000000000, 0.000000000000000000, 1.000000000000000000 ) ) ;
#22693 = EDGE_CURVE ( 'NONE', #6050, #12408, #18361, .T. ) ;
#22694 = DIRECTION ( 'NONE',  ( -0.000000000000000000, -0.000000000000000000, -1.000000000000000000 ) ) ;
#22695 = ADVANCED_FACE ( 'NONE', ( #1664 ), #21123, .F. ) ;
#22696 = CARTESIAN_POINT ( 'NONE',  ( 9.007774317138279585, -14.44244895400450801, 6.714907520933423690 ) ) ;
#22697 = CARTESIAN_POINT ( 'NONE',  ( 5.296161872597630271, 19.28602264385381204, 7.652108011868850035 ) ) ;
#22698 = DIRECTION ( 'NONE',  ( -1.000000000000000000, 0.000000000000000000, 0.000000000000000000 ) ) ;
#22699 = ORIENTED_EDGE ( 'NONE', *, *, #28347, .F. ) ;
#22700 = ORIENTED_EDGE ( 'NONE', *, *, #29224, .T. ) ;
#22701 = CARTESIAN_POINT ( 'NONE',  ( -13.00999358272542494, -0.8602714556717691030, 1.500000000000001332 ) ) ;
#22702 = CARTESIAN_POINT ( 'NONE',  ( -40.89187623478217404, -5.790488632116337797, -19.50000000000000355 ) ) ;
#22703 = ADVANCED_FACE ( 'NONE', ( #25527 ), #6341, .F. ) ;
#22704 = DIRECTION ( 'NONE',  ( 0.000000000000000000, 0.000000000000000000, 1.000000000000000000 ) ) ;
#22705 = ORIENTED_EDGE ( 'NONE', *, *, #23445, .F. ) ;
#22706 = DIRECTION ( 'NONE',  ( 0.000000000000000000, -1.132880637372608986E-16, 1.000000000000000000 ) ) ;
#22707 = EDGE_CURVE ( 'NONE', #22552, #26111, #14109, .T. ) ;
#22708 = PLANE ( 'NONE',  #7706 ) ;
#22710 = EDGE_CURVE ( 'NONE', #1147, #23584, #21284, .T. ) ;
#22709 = AXIS2_PLACEMENT_3D ( 'NONE', #22085, #14462, #10086 ) ;
#22711 = EDGE_LOOP ( 'NONE', ( #1353, #25851, #7737, #17917 ) ) ;
#22712 = ORIENTED_EDGE ( 'NONE', *, *, #265, .F. ) ;
#22713 = CARTESIAN_POINT ( 'NONE',  ( -19.75759631649036407, 3.218781778493905676, 7.359006845440219102 ) ) ;
#22714 = CARTESIAN_POINT ( 'NONE',  ( 16.65022252850693363, 3.724077645907920342, 20.19593175699879595 ) ) ;
#22715 = CIRCLE ( 'NONE', #18741, 0.7499999999999997780 ) ;
#22716 = DIRECTION ( 'NONE',  ( 0.000000000000000000, 0.000000000000000000, 1.000000000000000000 ) ) ;
#22717 = LINE ( 'NONE', #13387, #12998 ) ;
#22718 = ORIENTED_EDGE ( 'NONE', *, *, #24457, .T. ) ;
#22719 = LINE ( 'NONE', #3717, #8371 ) ;
#22720 = VERTEX_POINT ( 'NONE', #4003 ) ;
#22721 = CARTESIAN_POINT ( 'NONE',  ( 0.000000000000000000, -2.435693370351110282E-15, 21.50000000000000355 ) ) ;
#22722 = CARTESIAN_POINT ( 'NONE',  ( -6.414842543015754295, 17.06554576617236307, 1.500000000000000000 ) ) ;
#22723 = AXIS2_PLACEMENT_3D ( 'NONE', #18443, #11246, #6422 ) ;
#22724 = EDGE_CURVE ( 'NONE', #3185, #26303, #30806, .T. ) ;
#22725 = DIRECTION ( 'NONE',  ( 0.000000000000000000, -1.000000000000000000, 0.000000000000000000 ) ) ;
#22726 = EDGE_CURVE ( 'NONE', #9342, #22982, #28845, .T. ) ;
#22727 = CARTESIAN_POINT ( 'NONE',  ( 2.703030265324084080, -12.75514121382991384, 1.500000000000001332 ) ) ;
#22728 = CARTESIAN_POINT ( 'NONE',  ( 16.59873159789849595, 3.986191100139169663, 6.041646659195333058 ) ) ;
#22729 = CARTESIAN_POINT ( 'NONE',  ( -15.33339156390900193, 12.86857621502489657, 18.34777357837152323 ) ) ;
#22730 = EDGE_CURVE ( 'NONE', #19427, #3343, #18511, .T. ) ;
#22731 = CARTESIAN_POINT ( 'NONE',  ( -10.39981488257415698, -17.10438141112845400, 20.33971507717571114 ) ) ;
#22732 = VECTOR ( 'NONE', #8324, 1000.000000000000000 ) ;
#22733 = DIRECTION ( 'NONE',  ( -0.000000000000000000, -1.000000000000000000, -0.000000000000000000 ) ) ;
#22734 = CARTESIAN_POINT ( 'NONE',  ( -9.225205623801109311, -14.30976465324222957, 6.031926333436658183 ) ) ;
#22735 = CARTESIAN_POINT ( 'NONE',  ( 0.8750451464062526385, 9.041888939645140510, -1.500000000000000666 ) ) ;
#22736 = VERTEX_POINT ( 'NONE', #9603 ) ;
#22737 = EDGE_CURVE ( 'NONE', #7773, #6035, #21749, .T. ) ;
#22738 = DIRECTION ( 'NONE',  ( 0.06975647374412530244, 0.000000000000000000, 0.9975640502598241977 ) ) ;
#22739 = AXIS2_PLACEMENT_3D ( 'NONE', #1310, #24393, #19711 ) ;
#22740 = CARTESIAN_POINT ( 'NONE',  ( 35.76481447503398670, -5.202797454133663457, 34.80090346875810070 ) ) ;
#22741 = VERTEX_POINT ( 'NONE', #9907 ) ;
#22742 = ORIENTED_EDGE ( 'NONE', *, *, #7655, .T. ) ;
#22743 = CARTESIAN_POINT ( 'NONE',  ( 49.66189766834159514, 69.99759634488681570, 19.83556485701890892 ) ) ;
#22744 = CARTESIAN_POINT ( 'NONE',  ( 11.40980092660686118, 6.310027164379057751, 1.500000000000001332 ) ) ;
#22745 = ADVANCED_FACE ( 'NONE', ( #21908 ), #19111, .T. ) ;
#22746 = CARTESIAN_POINT ( 'NONE',  ( -5.460567910819449366, 19.25894470870317221, 5.796888747622817029 ) ) ;
#22747 = ORIENTED_EDGE ( 'NONE', *, *, #12967, .T. ) ;
#22748 = CARTESIAN_POINT ( 'NONE',  ( -9.675133109038686285, -8.168544852422948921, 1.500000000000000000 ) ) ;
#22749 = VECTOR ( 'NONE', #28151, 1000.000000000000000 ) ;
#22750 = CARTESIAN_POINT ( 'NONE',  ( -15.26435939152463384, 8.070345032481604619, 1.500000000000000000 ) ) ;
#22751 = VECTOR ( 'NONE', #19284, 1000.000000000000000 ) ;
#22752 = CARTESIAN_POINT ( 'NONE',  ( 23.21352257770656990, 10.78826658734920230, 49.40206402021032517 ) ) ;
#22753 = VERTEX_POINT ( 'NONE', #14258 ) ;
#22754 = LINE ( 'NONE', #29636, #20227 ) ;
#22755 = CARTESIAN_POINT ( 'NONE',  ( 12.35522127307955920, 11.74279147895036068, 5.652196082364320695 ) ) ;
#22756 = CARTESIAN_POINT ( 'NONE',  ( -40.00000000000002842, 90.00000000000001421, 27.49999999999983658 ) ) ;
#22757 = EDGE_LOOP ( 'NONE', ( #1324, #6441, #4370, #10076 ) ) ;
#22758 = CIRCLE ( 'NONE', #24251, 0.7500000000000004441 ) ;
#22759 = CARTESIAN_POINT ( 'NONE',  ( 15.18428249823343457, 13.04421712177833470, 5.749228751562096562 ) ) ;
#22760 = ORIENTED_EDGE ( 'NONE', *, *, #19679, .F. ) ;
#22761 = ADVANCED_FACE ( 'NONE', ( #26282 ), #16765, .F. ) ;
#22762 = VECTOR ( 'NONE', #12974, 1000.000000000000000 ) ;
#22763 = EDGE_CURVE ( 'NONE', #4121, #21028, #8420, .T. ) ;
#22764 = CIRCLE ( 'NONE', #12335, 9.084132297865673777 ) ;
#22765 = ORIENTED_EDGE ( 'NONE', *, *, #4701, .F. ) ;
#22766 = ORIENTED_EDGE ( 'NONE', *, *, #14529, .T. ) ;
#22767 = CARTESIAN_POINT ( 'NONE',  ( 3.623302445573600039, 16.66947753447049863, 7.559636331181775581 ) ) ;
#22768 = CARTESIAN_POINT ( 'NONE',  ( -28.34828976096172681, 29.18752572968383419, 1.500000000000000000 ) ) ;
#22769 = B_SPLINE_CURVE_WITH_KNOTS ( 'NONE', 3,
 ( #27899, #23495, #28502, #25548, #13553, #11515, #26008, #28184, #8867, #21145, #23032, #28357, #16491, #4636 ),
 .UNSPECIFIED., .F., .F.,
 ( 4, 2, 2, 2, 2, 2, 4 ),
 ( 2.108610145937280049E-07, 0.0004867403503157841311, 0.0009732698396169746011, 0.001459799328918164746, 0.001946328818219355324, 0.002919387796821722603, 0.003892446775424090316 ),
 .UNSPECIFIED. ) ;
#22770 = CARTESIAN_POINT ( 'NONE',  ( 6.262360769054551746, 18.99428434097456631, 19.47728749465737863 ) ) ;
#22771 = VECTOR ( 'NONE', #9088, 1000.000000000000000 ) ;
#22772 = ORIENTED_EDGE ( 'NONE', *, *, #19904, .F. ) ;
#22773 = CIRCLE ( 'NONE', #9330, 1.000000000000010436 ) ;
#22774 = CARTESIAN_POINT ( 'NONE',  ( -17.94248964168179938, -34.33858135081683827, 27.50000000000001066 ) ) ;
#22775 = CARTESIAN_POINT ( 'NONE',  ( 10.75049709165479683, -16.88611404641621405, 18.44501272782439827 ) ) ;
#22776 = CARTESIAN_POINT ( 'NONE',  ( 16.86235748570415183, 2.342382300094908665, 19.87181966307587544 ) ) ;
#22777 = ORIENTED_EDGE ( 'NONE', *, *, #19819, .T. ) ;
#22778 = VECTOR ( 'NONE', #7987, 1000.000000000000000 ) ;
#22779 = CARTESIAN_POINT ( 'NONE',  ( -19.74495986540963699, 3.294819794740639463, 19.96783386855779341 ) ) ;
#22780 = CARTESIAN_POINT ( 'NONE',  ( 18.35115206909799923, -7.996681782469499566, 7.652108011868850035 ) ) ;
#22781 = CIRCLE ( 'NONE', #15818, 9.000000000000000000 ) ;
#22782 = FACE_OUTER_BOUND ( 'NONE', #12114, .T. ) ;
#22783 = CARTESIAN_POINT ( 'NONE',  ( 3.269395338272003126, 16.75466097144276034, 18.73743063545763121 ) ) ;
#22784 = ORIENTED_EDGE ( 'NONE', *, *, #9963, .F. ) ;
#22785 = ORIENTED_EDGE ( 'NONE', *, *, #2320, .F. ) ;
#22786 = CIRCLE ( 'NONE', #1381, 0.7500000000000006661 ) ;
#22787 = CARTESIAN_POINT ( 'NONE',  ( -7.392982946727046034, 5.278755796068742789, -1.500000000000001110 ) ) ;
#22788 = DIRECTION ( 'NONE',  ( 1.000000000000000000, 0.000000000000000000, 0.000000000000000000 ) ) ;
#22789 = CARTESIAN_POINT ( 'NONE',  ( -5.048943207435891978, 19.37072948160042429, 19.66989035740801839 ) ) ;
#22790 = CARTESIAN_POINT ( 'NONE',  ( -25.64627119138473432, 23.40052582045089480, -16.50000000000000000 ) ) ;
#22791 = AXIS2_PLACEMENT_3D ( 'NONE', #13765, #4099, #23262 ) ;
#22792 = DIRECTION ( 'NONE',  ( -0.000000000000000000, 1.132880637372608986E-16, -1.000000000000000000 ) ) ;
#22793 = DIRECTION ( 'NONE',  ( -0.000000000000000000, -0.000000000000000000, 1.000000000000000000 ) ) ;
#22794 = DIRECTION ( 'NONE',  ( -0.000000000000000000, 0.000000000000000000, 1.000000000000000000 ) ) ;
#22795 = AXIS2_PLACEMENT_3D ( 'NONE', #861, #17553, #24713 ) ;
#22796 = ORIENTED_EDGE ( 'NONE', *, *, #9795, .T. ) ;
#22797 = CIRCLE ( 'NONE', #11845, 6.999999999999999112 ) ;
#22798 = FACE_OUTER_BOUND ( 'NONE', #8446, .T. ) ;
#22799 = EDGE_LOOP ( 'NONE', ( #24582, #5504, #2802, #1866 ) ) ;
#22800 = AXIS2_PLACEMENT_3D ( 'NONE', #10862, #8533, #6178 ) ;
#22801 = DIRECTION ( 'NONE',  ( -1.000000000000000000, -0.000000000000000000, -0.000000000000000000 ) ) ;
#22802 = CARTESIAN_POINT ( 'NONE',  ( 5.881244434206234217, 6.812559277181991391, 1.500000000000001332 ) ) ;
#22803 = ORIENTED_EDGE ( 'NONE', *, *, #9033, .F. ) ;
#22804 = ORIENTED_EDGE ( 'NONE', *, *, #1752, .F. ) ;
#22805 = CARTESIAN_POINT ( 'NONE',  ( -19.75724448635271457, 3.108068420208399907, 5.849008070840541862 ) ) ;
#22806 = AXIS2_PLACEMENT_3D ( 'NONE', #21614, #9761, #10073 ) ;
#22807 = EDGE_CURVE ( 'NONE', #24290, #9920, #1473, .T. ) ;
#22808 = DIRECTION ( 'NONE',  ( 0.000000000000000000, 0.000000000000000000, 1.000000000000000000 ) ) ;
#22809 = ORIENTED_EDGE ( 'NONE', *, *, #1089, .T. ) ;
#22810 = CARTESIAN_POINT ( 'NONE',  ( 4.608906612435600181, 7.730328572437758616, 21.50000000000000000 ) ) ;
#22811 = CIRCLE ( 'NONE', #15344, 34.99999999999933920 ) ;
#22812 = ADVANCED_FACE ( 'NONE', ( #7731 ), #17230, .F. ) ;
#22813 = CARTESIAN_POINT ( 'NONE',  ( 15.00007558036415567, 47.69693630192244882, -54.01249125054359723 ) ) ;
#22814 = DIRECTION ( 'NONE',  ( 0.000000000000000000, 0.000000000000000000, 1.000000000000000000 ) ) ;
#22815 = CARTESIAN_POINT ( 'NONE',  ( -23.20738078402527549, -23.09073189384302793, -16.50001200000000523 ) ) ;
#22816 = DIRECTION ( 'NONE',  ( 0.000000000000000000, 0.000000000000000000, -1.000000000000000000 ) ) ;
#22817 = CARTESIAN_POINT ( 'NONE',  ( 37.99999999999999289, 70.00000000000000000, -87.50000000000000000 ) ) ;
#22818 = DIRECTION ( 'NONE',  ( 0.000000000000000000, -0.000000000000000000, -1.000000000000000000 ) ) ;
#22819 = CARTESIAN_POINT ( 'NONE',  ( -19.18576292979354392, -22.55620591602727742, 24.50000000000000000 ) ) ;
#22820 = VERTEX_POINT ( 'NONE', #5384 ) ;
#22821 = CIRCLE ( 'NONE', #27824, 2.898871837527151385 ) ;
#22822 = AXIS2_PLACEMENT_3D ( 'NONE', #24967, #25440, #15928 ) ;
#22823 = CARTESIAN_POINT ( 'NONE',  ( 0.000000000000000000, 12.50000000000000000, -87.50000000000000000 ) ) ;
#22824 = CARTESIAN_POINT ( 'NONE',  ( -6.055745631507628346, 15.95075576291064756, 7.500147780736496017 ) ) ;
#22825 = FACE_OUTER_BOUND ( 'NONE', #14960, .T. ) ;
#22826 = CARTESIAN_POINT ( 'NONE',  ( 0.000000000000000000, 44.39187623478217404, -19.50000000000000355 ) ) ;
#22827 = LINE ( 'NONE', #22662, #5637 ) ;
#22828 = CIRCLE ( 'NONE', #17354, 1.447898107987198646 ) ;
#22829 = VERTEX_POINT ( 'NONE', #26755 ) ;
#22830 = DIRECTION ( 'NONE',  ( -0.000000000000000000, -0.000000000000000000, 1.000000000000000000 ) ) ;
#22831 = CARTESIAN_POINT ( 'NONE',  ( -35.76344986165604212, -22.29344514668547461, -19.50000000000000355 ) ) ;
#22832 = CARTESIAN_POINT ( 'NONE',  ( 0.4781620243103129053, -42.50348742054170970, 34.61334324197476775 ) ) ;
#22833 = B_SPLINE_CURVE_WITH_KNOTS ( 'NONE', 3,
 ( #14622, #9787, #29283, #19302, #888, #14765, #3227, #10241, #26797, #24743, #10091, #5574 ),
 .UNSPECIFIED., .F., .F.,
 ( 4, 2, 2, 2, 2, 4 ),
 ( 0.000000000000000000, 0.005323107084052460837, 0.01064621416810492167, 0.01596932125215738338, 0.01863087479418361336, 0.02129242833620984335 ),
 .UNSPECIFIED. ) ;
#22834 = DIRECTION ( 'NONE',  ( -0.9096319953545185522, 0.4154150130018859355, 0.000000000000000000 ) ) ;
#22835 = ORIENTED_EDGE ( 'NONE', *, *, #23486, .F. ) ;
#22836 = CARTESIAN_POINT ( 'NONE',  ( -2.555255504830902691, 9.131494062835640690, 21.50000000000000000 ) ) ;
#22837 = CARTESIAN_POINT ( 'NONE',  ( 39.00000000000000000, 5.563236990218597633, -1.500000000000000000 ) ) ;
#22838 = CARTESIAN_POINT ( 'NONE',  ( -8.546421330728135146, -14.74799399454104432, 5.652196082367002994 ) ) ;
#22839 = ORIENTED_EDGE ( 'NONE', *, *, #8049, .T. ) ;
#22840 = B_SPLINE_SURFACE_WITH_KNOTS ( 'NONE', 1, 3, ( 
 ( #1763, #18757, #23270, #20926, #4408, #4556, #13924, #14060, #30005, #27661, #25322, #29036, #4709, #11899, #30755, #18918, #12194, #19372, #28892, #9544, #14680, #12358, #9857, #175, #2836, #32, #17024, #26075, #9695, #14209, #21861, #5329, #9401, #14838, #28426, #7050, #26548, #12046, #496, #7526, #2532, #23723 ),
 ( #4865, #2214, #16716, #5175, #26227, #21224, #2371, #10016, #26396, #21392, #19204, #16557, #19057, #28574, #14381, #7677, #17177, #7203, #21540, #23888, #28733, #26697, #24183, #7369, #11731, #16878, #5021, #14534, #24032, #2679, #21692, #333, #10627, #12518, #17650, #3148, #1115, #10315, #24971, #29188, #24658, #792 ) ),
 .UNSPECIFIED., .F., .T., .F.,
 ( 2, 2 ),
 ( 4, 2, 2, 2, 2, 2, 2, 2, 2, 2, 2, 2, 2, 2, 2, 2, 2, 2, 2, 2, 4 ),
 ( 0.000000000000000000, 1.000000000000000000 ),
 ( 0.000000000000000000, 0.1963495408493620697, 0.3926990816987241395, 0.7853981633974482790, 1.178097245096172418, 1.570796326794896558, 1.963495408493620697, 2.356194490192344837, 2.748893571891068976, 2.945243112740430824, 3.141592653589793116, 3.337942194439155408, 3.534291735288517255, 3.926990816987241395, 4.319689898685965090, 4.712388980384689674, 5.105088062083414258, 5.497787143782137953, 5.890486225480861648, 6.086835766330223940, 6.283185307179586232 ),
 .UNSPECIFIED. ) ;
#22841 = CIRCLE ( 'NONE', #26842, 0.7500000000000006661 ) ;
#22842 = AXIS2_PLACEMENT_3D ( 'NONE', #9777, #564, #10084 ) ;
#22843 = CARTESIAN_POINT ( 'NONE',  ( -8.325649706210086265, -14.88445757357571786, 20.34789198813115618 ) ) ;
#22844 = AXIS2_PLACEMENT_3D ( 'NONE', #4154, #16010, #1056 ) ;
#22845 = CARTESIAN_POINT ( 'NONE',  ( 19.59736455876166517, 3.994007928088045389, 18.73377938172348678 ) ) ;
#22846 = ORIENTED_EDGE ( 'NONE', *, *, #19805, .F. ) ;
#22847 = CARTESIAN_POINT ( 'NONE',  ( -29.61203839202723032, -15.40012917324033381, 41.62281023987518580 ) ) ;
#22848 = DIRECTION ( 'NONE',  ( 0.000000000000000000, 1.000000000000000000, -0.000000000000000000 ) ) ;
#22849 = CIRCLE ( 'NONE', #8930, 9.084132297865673777 ) ;
#22850 = ORIENTED_EDGE ( 'NONE', *, *, #22241, .F. ) ;
#22851 = DIRECTION ( 'NONE',  ( 0.000000000000000000, 0.000000000000000000, 1.000000000000000000 ) ) ;
#22852 = CARTESIAN_POINT ( 'NONE',  ( 16.59792644105115755, 3.991267606926847122, 7.269896094239229889 ) ) ;
#22853 = CARTESIAN_POINT ( 'NONE',  ( 0.6218383925729463746, -19.99069893758406735, 18.37545668562167478 ) ) ;
#22854 = DIRECTION ( 'NONE',  ( 1.000000000000000000, 0.000000000000000000, 0.000000000000000000 ) ) ;
#22855 = CARTESIAN_POINT ( 'NONE',  ( -17.02473723649752557, 1.129071356226221345, 7.545655578832111132 ) ) ;
#22856 = FACE_BOUND ( 'NONE', #27049, .T. ) ;
#22857 = DIRECTION ( 'NONE',  ( -5.125319360840571077E-16, 1.000000000000000000, 0.000000000000000000 ) ) ;
#22858 = CARTESIAN_POINT ( 'NONE',  ( -15.16307827826492627, -7.786259562520722710, 5.652196082368482699 ) ) ;
#22859 = CARTESIAN_POINT ( 'NONE',  ( -37.50000000000005684, 9.285362311011880811E-15, 37.50000000000000000 ) ) ;
#22860 = CARTESIAN_POINT ( 'NONE',  ( 32.28307784207223108, -8.475829241206289666, 41.62281023987511475 ) ) ;
#22861 = DIRECTION ( 'NONE',  ( 0.000000000000000000, 0.000000000000000000, 1.000000000000000000 ) ) ;
#22862 = CIRCLE ( 'NONE', #9426, 37.50000000000001421 ) ;
#22863 = VERTEX_POINT ( 'NONE', #14729 ) ;
#22864 = ORIENTED_EDGE ( 'NONE', *, *, #22137, .T. ) ;
#22865 = FACE_OUTER_BOUND ( 'NONE', #14959, .T. ) ;
#22866 = CARTESIAN_POINT ( 'NONE',  ( -35.76344986165608475, 22.29344514668535027, -19.50000000000000355 ) ) ;
#22867 = PLANE ( 'NONE',  #14391 ) ;
#22868 = ORIENTED_EDGE ( 'NONE', *, *, #22724, .F. ) ;
#22869 = CIRCLE ( 'NONE', #9433, 1.000000000000000888 ) ;
#22870 = CARTESIAN_POINT ( 'NONE',  ( 23.05654803568420874, -35.38768970123555135, -9.833278305091164739 ) ) ;
#22871 = DIRECTION ( 'NONE',  ( -0.000000000000000000, -0.000000000000000000, 1.000000000000000000 ) ) ;
#22872 = ORIENTED_EDGE ( 'NONE', *, *, #26147, .F. ) ;
#22873 = VERTEX_POINT ( 'NONE', #14890 ) ;
#22874 = PRODUCT_DEFINITION ( 'UNKNOWN', '', #17365, #22920 ) ;
#22875 = CARTESIAN_POINT ( 'NONE',  ( -16.92089108241427198, 1.982400079378045410, 5.701226463332907279 ) ) ;
#22876 = FACE_OUTER_BOUND ( 'NONE', #26204, .T. ) ;
#22877 = CARTESIAN_POINT ( 'NONE',  ( -11.82521593960875528, 5.400395169024524655, 1.500000000000001332 ) ) ;
#22878 = CARTESIAN_POINT ( 'NONE',  ( 0.000000000000000000, -3.165563358393047634E-15, 27.94260272410217638 ) ) ;
#22879 = ORIENTED_EDGE ( 'NONE', *, *, #10806, .T. ) ;
#22880 = CARTESIAN_POINT ( 'NONE',  ( 0.000000000000000000, 7.500000000000007994, -87.50000000000000000 ) ) ;
#22881 = ORIENTED_EDGE ( 'NONE', *, *, #18979, .F. ) ;
#22882 = ADVANCED_FACE ( 'NONE', ( #26603 ), #20093, .T. ) ;
#22883 = CARTESIAN_POINT ( 'NONE',  ( 0.3567147238643512130, -19.99681861211370659, 5.652196082369963293 ) ) ;
#22884 = CARTESIAN_POINT ( 'NONE',  ( -16.94912694327470959, 1.778434105053336545, 18.34727598691068096 ) ) ;
#22885 = VERTEX_POINT ( 'NONE', #20345 ) ;
#22886 = DIRECTION ( 'NONE',  ( 1.000000000000000000, 0.000000000000000000, 0.000000000000000000 ) ) ;
#22887 = CARTESIAN_POINT ( 'NONE',  ( -5.352643706120517209, -7.827050521741861999, 1.500000000000001332 ) ) ;
#22888 = AXIS2_PLACEMENT_3D ( 'NONE', #11672, #9179, #18692 ) ;
#22889 = ADVANCED_FACE ( 'NONE', ( #1318 ), #15347, .F. ) ;
#22890 = CARTESIAN_POINT ( 'NONE',  ( 32.98805937973595093, -22.67054169308931222, 8.000000000000003553 ) ) ;
#22891 = ADVANCED_FACE ( 'NONE', ( #7885 ), #7309, .T. ) ;
#22892 = CARTESIAN_POINT ( 'NONE',  ( -32.98805937973593672, 80.00000000000000000, 13.00000000000000178 ) ) ;
#22893 = CARTESIAN_POINT ( 'NONE',  ( -19.94516883457951550, 1.701953382846944196, 18.73743063545763121 ) ) ;
#22894 = DIRECTION ( 'NONE',  ( -0.000000000000000000, 0.000000000000000000, 1.000000000000000000 ) ) ;
#22895 = ORIENTED_EDGE ( 'NONE', *, *, #11639, .T. ) ;
#22896 = CIRCLE ( 'NONE', #12963, 50.00000000000000000 ) ;
#22897 = DIRECTION ( 'NONE',  ( -0.9975640502598243087, 0.000000000000000000, 0.06975647374412531632 ) ) ;
#22898 = CARTESIAN_POINT ( 'NONE',  ( 35.99999999999999289, -2.601438916704202242, 27.50000000000001066 ) ) ;
#22899 = ORIENTED_EDGE ( 'NONE', *, *, #24204, .T. ) ;
#22900 = ORIENTED_EDGE ( 'NONE', *, *, #7113, .T. ) ;
#22901 = CARTESIAN_POINT ( 'NONE',  ( 48.02684528033974942, 69.90336711249833002, 16.52639074396786611 ) ) ;
#22902 = CARTESIAN_POINT ( 'NONE',  ( -15.66719571743413475, 12.43196305300237903, 5.779535427900761135 ) ) ;
#22903 = CARTESIAN_POINT ( 'NONE',  ( -4.775770841707820402, 16.34206821731734038, 7.272049892295485485 ) ) ;
#22904 = VERTEX_POINT ( 'NONE', #10795 ) ;
#22905 = DIRECTION ( 'NONE',  ( 0.000000000000000000, 1.000000000000000000, 1.193512090021232842E-16 ) ) ;
#22906 = CARTESIAN_POINT ( 'NONE',  ( -13.21131958021091179, 10.75991052173262474, 5.676815824193226945 ) ) ;
#22907 = EDGE_CURVE ( 'NONE', #14013, #29295, #20309, .T. ) ;
#22908 = DIRECTION ( 'NONE',  ( -0.000000000000000000, -0.000000000000000000, 1.000000000000000000 ) ) ;
#22909 = ORIENTED_EDGE ( 'NONE', *, *, #3618, .F. ) ;
#22910 = EDGE_CURVE ( 'NONE', #5078, #20897, #15465, .T. ) ;
#22911 = EDGE_CURVE ( 'NONE', #29885, #18473, #21432, .T. ) ;
#22912 = CARTESIAN_POINT ( 'NONE',  ( 15.41296542101254552, 5.939519782021115191, 1.500000000000000000 ) ) ;
#22913 = CIRCLE ( 'NONE', #9989, 0.7500000000000006661 ) ;
#22914 = EDGE_CURVE ( 'NONE', #19687, #27309, #8478, .T. ) ;
#22915 = DIRECTION ( 'NONE',  ( -0.000000000000000000, -0.000000000000000000, -1.000000000000000000 ) ) ;
#22916 = VERTEX_POINT ( 'NONE', #7836 ) ;
#22917 = CARTESIAN_POINT ( 'NONE',  ( 0.000000000000000000, -2.435693370351110282E-15, 21.50000000000000355 ) ) ;
#22918 = ORIENTED_EDGE ( 'NONE', *, *, #14549, .T. ) ;
#22919 = EDGE_CURVE ( 'NONE', #21897, #6185, #5499, .T. ) ;
#22920 = PRODUCT_DEFINITION_CONTEXT ( 'detailed design', #8205, 'design' ) ;
#22921 = ORIENTED_EDGE ( 'NONE', *, *, #17393, .T. ) ;
#22922 = ORIENTED_EDGE ( 'NONE', *, *, #23253, .F. ) ;
#22923 = ADVANCED_FACE ( 'NONE', ( #24513 ), #13899, .T. ) ;
#22924 = EDGE_CURVE ( 'NONE', #4162, #21118, #4378, .T. ) ;
#22925 = CARTESIAN_POINT ( 'NONE',  ( 3.424309912165884207, 16.71834993634870159, 5.872146474157316831 ) ) ;
#22926 = CARTESIAN_POINT ( 'NONE',  ( 8.757878075398934925, -7.394122547431893011, 1.500000000000000000 ) ) ;
#22927 = CARTESIAN_POINT ( 'NONE',  ( -39.52380524535562500, 7.028748154183637631, -6.500000000000000888 ) ) ;
#22928 = ORIENTED_EDGE ( 'NONE', *, *, #16048, .F. ) ;
#22929 = CARTESIAN_POINT ( 'NONE',  ( 19.89647750965486495, 2.201534687727671802, 19.22654678686458141 ) ) ;
#22930 = ORIENTED_EDGE ( 'NONE', *, *, #17668, .T. ) ;
#22931 = DIRECTION ( 'NONE',  ( 1.000000000000000000, 2.396195514597832977E-15, 0.000000000000000000 ) ) ;
#22932 = CARTESIAN_POINT ( 'NONE',  ( 17.93426220341855526, -8.892634148397206673, 6.420335371522007506 ) ) ;
#22933 = CARTESIAN_POINT ( 'NONE',  ( -13.66451197432776432, 10.21236830578559562, 5.749491821935610147 ) ) ;
#22934 = CARTESIAN_POINT ( 'NONE',  ( 4.313865120791887442, 19.54726060313607050, 19.25672174529527325 ) ) ;
#22935 = ORIENTED_EDGE ( 'NONE', *, *, #6049, .F. ) ;
#22936 = EDGE_LOOP ( 'NONE', ( #26031, #10085, #8722, #24042 ) ) ;
#22937 = CARTESIAN_POINT ( 'NONE',  ( 1.530808498934192310E-15, -12.50000000000000888, -16.50000000000000000 ) ) ;
#22938 = LINE ( 'NONE', #20901, #10639 ) ;
#22939 = EDGE_CURVE ( 'NONE', #28942, #26950, #29862, .T. ) ;
#22940 = CARTESIAN_POINT ( 'NONE',  ( 15.05429537369196069, 13.16750578773771352, 18.37250658438899009 ) ) ;
#22941 = CARTESIAN_POINT ( 'NONE',  ( -4.568010850242215426, 16.39675899511904689, 19.33715507985239412 ) ) ;
#22942 = DIRECTION ( 'NONE',  ( 0.000000000000000000, 0.000000000000000000, 1.000000000000000000 ) ) ;
#22943 = CYLINDRICAL_SURFACE ( 'NONE', #14095, 20.00000000000000355 ) ;
#22944 = CARTESIAN_POINT ( 'NONE',  ( 0.000000000000000000, -2.435693370351110282E-15, 21.50000000000000355 ) ) ;
#22945 = EDGE_CURVE ( 'NONE', #2495, #30824, #8755, .T. ) ;
#22946 = DIRECTION ( 'NONE',  ( -0.000000000000000000, -0.000000000000000000, 1.000000000000000000 ) ) ;
#22947 = VERTEX_POINT ( 'NONE', #6718 ) ;
#22948 = EDGE_CURVE ( 'NONE', #2627, #24377, #11561, .T. ) ;
#22949 = DIRECTION ( 'NONE',  ( -1.000000000000000000, 0.000000000000000000, 0.000000000000000000 ) ) ;
#22950 = DIRECTION ( 'NONE',  ( -0.000000000000000000, 0.000000000000000000, 1.000000000000000000 ) ) ;
#22951 = FACE_OUTER_BOUND ( 'NONE', #24009, .T. ) ;
#22952 = ORIENTED_EDGE ( 'NONE', *, *, #13636, .T. ) ;
#22953 = ORIENTED_EDGE ( 'NONE', *, *, #9534, .F. ) ;
#22954 = CARTESIAN_POINT ( 'NONE',  ( -19.82747825358060467, 2.624647641736344461, 5.651480102388687143 ) ) ;
#22955 = CIRCLE ( 'NONE', #24965, 7.500000000000013323 ) ;
#22956 = CARTESIAN_POINT ( 'NONE',  ( 0.000000000000000000, -2.435693370351110282E-15, 21.50000000000000355 ) ) ;
#22957 = ORIENTED_EDGE ( 'NONE', *, *, #3164, .F. ) ;
#22958 = CARTESIAN_POINT ( 'NONE',  ( 0.2207535014603130841, -19.99921160563567923, 7.652108011868850923 ) ) ;
#22959 = FACE_OUTER_BOUND ( 'NONE', #17949, .T. ) ;
#22960 = CARTESIAN_POINT ( 'NONE',  ( -7.057542262939595190, -41.80922458147114895, 20.29292036719578363 ) ) ;
#22961 = CARTESIAN_POINT ( 'NONE',  ( 0.000000000000000000, 0.000000000000000000, 21.50000000000000000 ) ) ;
#22962 = CARTESIAN_POINT ( 'NONE',  ( -6.193882932557621679, 19.03538945389874470, 18.37415474056476938 ) ) ;
#22963 = CARTESIAN_POINT ( 'NONE',  ( 32.19782014694308003, -14.25394737442115201, 39.78814634291934738 ) ) ;
#22964 = CARTESIAN_POINT ( 'NONE',  ( 1.638502901550993540, -16.99392728441680234, 7.196036389296800451 ) ) ;
#22965 = CARTESIAN_POINT ( 'NONE',  ( -25.48568755041063838, -12.36160011285428517, 24.50000000000000000 ) ) ;
#22966 = ORIENTED_EDGE ( 'NONE', *, *, #13989, .T. ) ;
#22967 = CARTESIAN_POINT ( 'NONE',  ( 9.062880100047298271, 0.6210184355499750453, 13.22130136205108819 ) ) ;
#22968 = DIRECTION ( 'NONE',  ( -1.000000000000000000, 0.000000000000000000, 0.000000000000000000 ) ) ;
#22969 = CARTESIAN_POINT ( 'NONE',  ( -5.544451646083596863, 16.11829163520482311, 7.652108011868850035 ) ) ;
#22970 = CYLINDRICAL_SURFACE ( 'NONE', #5834, 10.00000000000000178 ) ;
#22971 = EDGE_CURVE ( 'NONE', #4164, #14021, #7692, .T. ) ;
#22972 = CARTESIAN_POINT ( 'NONE',  ( -37.98493438988125348, -11.12428508575252728, -1.500000000000000000 ) ) ;
#22973 = ADVANCED_FACE ( 'NONE', ( #4082 ), #1448, .F. ) ;
#22974 = CARTESIAN_POINT ( 'NONE',  ( -5.604556300746500241, -15.53790034020399169, 1.500000000000000000 ) ) ;
#22975 = ORIENTED_EDGE ( 'NONE', *, *, #17536, .F. ) ;
#22976 = DIRECTION ( 'NONE',  ( -0.000000000000000000, -0.000000000000000000, 1.000000000000000000 ) ) ;
#22977 = CARTESIAN_POINT ( 'NONE',  ( -25.19442432475839055, 35.44676296258369064, -19.50000000000000355 ) ) ;
#22978 = CARTESIAN_POINT ( 'NONE',  ( 29.48815749055103552, -23.29943950550710952, 37.50000000016476775 ) ) ;
#22980 = CARTESIAN_POINT ( 'NONE',  ( 8.499586724479435418, 2.959227181723830036, 1.500000000000001332 ) ) ;
#22979 = B_SPLINE_CURVE_WITH_KNOTS ( 'NONE', 3,
 ( #17201, #26724, #24378, #12541 ),
 .UNSPECIFIED., .F., .F.,
 ( 4, 4 ),
 ( 3.022186913405034649E-07, 0.007932103869840197510 ),
 .UNSPECIFIED. ) ;
#22981 = ORIENTED_EDGE ( 'NONE', *, *, #13785, .T. ) ;
#22982 = VERTEX_POINT ( 'NONE', #13610 ) ;
#22983 = CARTESIAN_POINT ( 'NONE',  ( -13.22505861668184046, -42.10773672057003125, -19.50000000000000355 ) ) ;
#22984 = FACE_OUTER_BOUND ( 'NONE', #5031, .T. ) ;
#22985 = EDGE_LOOP ( 'NONE', ( #11787, #7386 ) ) ;
#22986 = CIRCLE ( 'NONE', #9541, 6.999999999999999112 ) ;
#22987 = LINE ( 'NONE', #29563, #7374 ) ;
#22988 = CARTESIAN_POINT ( 'NONE',  ( -10.03589362353479686, -36.13692893856508448, 37.49999999997990585 ) ) ;
#22989 = ORIENTED_EDGE ( 'NONE', *, *, #7646, .T. ) ;
#22990 = CARTESIAN_POINT ( 'NONE',  ( -5.349779314757642901, -7.341751895053217680, -1.500000000000002665 ) ) ;
#22991 = CARTESIAN_POINT ( 'NONE',  ( -8.546421331151641709, -14.74799399427946689, 5.652196082364321583 ) ) ;
#22992 = AXIS2_PLACEMENT_3D ( 'NONE', #10686, #22393, #17413 ) ;
#22993 = CARTESIAN_POINT ( 'NONE',  ( 31.57687401261851434, -15.10620312102103213, 39.99603010801624237 ) ) ;
#22994 = FACE_OUTER_BOUND ( 'NONE', #12433, .T. ) ;
#22995 = ORIENTED_EDGE ( 'NONE', *, *, #4253, .F. ) ;
#22996 = CARTESIAN_POINT ( 'NONE',  ( 7.730328572437743517, -4.608906612435629491, 21.50000000000000000 ) ) ;
#22997 = CARTESIAN_POINT ( 'NONE',  ( 39.99999999999998579, 70.00000000000000000, 12.49999999999999112 ) ) ;
#22998 = CARTESIAN_POINT ( 'NONE',  ( 6.900000000000000355, 0.000000000000000000, 0.000000000000000000 ) ) ;
#22999 = CARTESIAN_POINT ( 'NONE',  ( 32.19782014694307293, 14.25394737442116444, 35.54550565580007770 ) ) ;
#23000 = CARTESIAN_POINT ( 'NONE',  ( -15.49859937932966680, -7.047316568154765370, 19.96344307082652847 ) ) ;
#23001 = CYLINDRICAL_SURFACE ( 'NONE', #23790, 4.999999999999997335 ) ;
#23002 = CARTESIAN_POINT ( 'NONE',  ( 16.65122935894595813, 13.93942108199718888, 1.500000000000000000 ) ) ;
#23003 = CARTESIAN_POINT ( 'NONE',  ( -32.24119420145671455, 26.76047160551536663, -16.50000600000000262 ) ) ;
#23004 = AXIS2_PLACEMENT_3D ( 'NONE', #15415, #22437, #16720 ) ;
#23005 = FACE_OUTER_BOUND ( 'NONE', #30457, .T. ) ;
#23006 = EDGE_CURVE ( 'NONE', #9226, #25866, #1736, .T. ) ;
#23007 = ORIENTED_EDGE ( 'NONE', *, *, #21603, .T. ) ;
#23008 = ORIENTED_EDGE ( 'NONE', *, *, #482, .F. ) ;
#23009 = FACE_BOUND ( 'NONE', #25088, .T. ) ;
#23010 = CARTESIAN_POINT ( 'NONE',  ( 20.65888525914375862, -38.75220717792901581, -19.50000000000000355 ) ) ;
#23011 = DIRECTION ( 'NONE',  ( -0.000000000000000000, -0.000000000000000000, 1.000000000000000000 ) ) ;
#23012 = ORIENTED_EDGE ( 'NONE', *, *, #22275, .F. ) ;
#23013 =( NAMED_UNIT ( * ) SI_UNIT ( $, .STERADIAN. ) SOLID_ANGLE_UNIT ( ) );
#23014 = CARTESIAN_POINT ( 'NONE',  ( 0.000000000000000000, -7.794228634059938265, -4.500000000000013323 ) ) ;
#23015 = CARTESIAN_POINT ( 'NONE',  ( 9.860909914091285700, -13.90333503830274253, 20.34789198813115263 ) ) ;
#23016 = EDGE_LOOP ( 'NONE', ( #11609, #6025, #20049, #1216 ) ) ;
#23017 = ORIENTED_EDGE ( 'NONE', *, *, #10693, .T. ) ;
#23018 = CARTESIAN_POINT ( 'NONE',  ( -16.96555893295483841, 1.647560171216676750, 5.652196082367002106 ) ) ;
#23019 = DIRECTION ( 'NONE',  ( -1.000000000000000000, 0.000000000000000000, 0.000000000000000000 ) ) ;
#23020 = CARTESIAN_POINT ( 'NONE',  ( -5.206534544686763688, -43.71581230463343104, -16.50000000000000000 ) ) ;
#23021 = CARTESIAN_POINT ( 'NONE',  ( -0.5205051961121548443, 42.60095040672530331, 34.61591466868899403 ) ) ;
#23022 = VERTEX_POINT ( 'NONE', #18446 ) ;
#23023 = DIRECTION ( 'NONE',  ( 0.000000000000000000, -1.132880637372608986E-16, 1.000000000000000000 ) ) ;
#23024 = AXIS2_PLACEMENT_3D ( 'NONE', #13028, #25334, #1166 ) ;
#23025 = ORIENTED_EDGE ( 'NONE', *, *, #251, .F. ) ;
#23026 = CIRCLE ( 'NONE', #3118, 17.00000000000000000 ) ;
#23027 = CARTESIAN_POINT ( 'NONE',  ( -14.71622834325375351, -8.664216105401095547, 6.917457548096559883 ) ) ;
#23028 = DIRECTION ( 'NONE',  ( 1.000000000000000000, 0.000000000000000000, 0.000000000000000000 ) ) ;
#23029 = ORIENTED_EDGE ( 'NONE', *, *, #25180, .T. ) ;
#23030 = CARTESIAN_POINT ( 'NONE',  ( -39.52380524535903561, -7.028748154198949827, -11.49999999999999645 ) ) ;
#23031 = CARTESIAN_POINT ( 'NONE',  ( 33.42393154775842135, -22.05663106644447424, 30.87484722992571307 ) ) ;
#23032 = CARTESIAN_POINT ( 'NONE',  ( 26.12047388987419794, -6.311255530320351248, 48.12792051007059513 ) ) ;
#23033 = EDGE_CURVE ( 'NONE', #9360, #25532, #26874, .T. ) ;
#23034 = CARTESIAN_POINT ( 'NONE',  ( 0.000000000000000000, 0.000000000000000000, -87.50000000000000000 ) ) ;
#23035 = CARTESIAN_POINT ( 'NONE',  ( -19.95549607358725908, 1.576375212833064143, 18.92976555901915603 ) ) ;
#23036 = CARTESIAN_POINT ( 'NONE',  ( 0.000000000000000000, 0.000000000000000000, 1.500000000000000000 ) ) ;
#23037 = EDGE_LOOP ( 'NONE', ( #4342, #8189, #6842, #24125 ) ) ;
#23038 = CARTESIAN_POINT ( 'NONE',  ( 33.16313691975489064, 0.000000000000000000, -1.500000000000000000 ) ) ;
#23039 = CARTESIAN_POINT ( 'NONE',  ( 23.69412710310940540, -29.84645176427128987, 34.80090346875809360 ) ) ;
#23040 = ORIENTED_EDGE ( 'NONE', *, *, #30760, .F. ) ;
#23041 = ORIENTED_EDGE ( 'NONE', *, *, #25163, .F. ) ;
#23042 = VECTOR ( 'NONE', #29926, 1000.000000000000000 ) ;
#23043 = CARTESIAN_POINT ( 'NONE',  ( 10.89102995336899937, -16.77499580993352524, 5.676722608126683944 ) ) ;
#23044 = EDGE_CURVE ( 'NONE', #4677, #25657, #19380, .T. ) ;
#23045 = CIRCLE ( 'NONE', #634, 7.500000000000013323 ) ;
#23046 = CARTESIAN_POINT ( 'NONE',  ( -38.00000000000000711, 80.00000000000000000, 17.91742430504400119 ) ) ;
#23047 = ORIENTED_EDGE ( 'NONE', *, *, #15854, .T. ) ;
#23048 = CARTESIAN_POINT ( 'NONE',  ( 5.738360882149951436, 7.548823014270661602, 1.500000000000001332 ) ) ;
#23049 = EDGE_CURVE ( 'NONE', #26988, #10311, #30359, .T. ) ;
#23050 = DIRECTION ( 'NONE',  ( -0.000000000000000000, 1.132880637372608986E-16, -1.000000000000000000 ) ) ;
#23051 = PLANE ( 'NONE',  #8968 ) ;
#23052 = ORIENTED_EDGE ( 'NONE', *, *, #29404, .F. ) ;
#23053 = CARTESIAN_POINT ( 'NONE',  ( -8.249114229549590505, 0.1262659238205133538, -1.500000000000001776 ) ) ;
#23054 = FACE_OUTER_BOUND ( 'NONE', #28106, .T. ) ;
#23055 = ORIENTED_EDGE ( 'NONE', *, *, #13004, .F. ) ;
#23056 = EDGE_CURVE ( 'NONE', #5977, #15053, #13438, .T. ) ;
#23057 = EDGE_LOOP ( 'NONE', ( #7031, #28228, #10924, #22267 ) ) ;
#23058 = DIRECTION ( 'NONE',  ( 1.000000000000000000, 0.000000000000000000, 0.000000000000000000 ) ) ;
#23059 = ORIENTED_EDGE ( 'NONE', *, *, #29111, .T. ) ;
#23060 = VERTEX_POINT ( 'NONE', #30277 ) ;
#23061 = CARTESIAN_POINT ( 'NONE',  ( -18.06093776605887058, -8.632162463936113639, 7.652108011868850035 ) ) ;
#23062 = VECTOR ( 'NONE', #28399, 1000.000000000000000 ) ;
#23063 = CARTESIAN_POINT ( 'NONE',  ( 9.216505592218814158, -7.781333699927420966, 1.500000000000000000 ) ) ;
#23064 = DIRECTION ( 'NONE',  ( -0.000000000000000000, -0.000000000000000000, 1.000000000000000000 ) ) ;
#23065 = ORIENTED_EDGE ( 'NONE', *, *, #22488, .T. ) ;
#23066 = EDGE_CURVE ( 'NONE', #20277, #160, #13902, .T. ) ;
#23067 = CARTESIAN_POINT ( 'NONE',  ( -28.55068628633583216, -24.19494186940697134, 27.50000000000000355 ) ) ;
#23068 = CYLINDRICAL_SURFACE ( 'NONE', #10332, 1.999999999999998224 ) ;
#23069 = DIRECTION ( 'NONE',  ( -1.000000000000000000, 0.000000000000000000, 0.000000000000000000 ) ) ;
#23070 = EDGE_CURVE ( 'NONE', #13268, #18557, #1970, .T. ) ;
#23071 = VERTEX_POINT ( 'NONE', #27949 ) ;
#23072 = EDGE_CURVE ( 'NONE', #19902, #18416, #8616, .T. ) ;
#23073 = DIRECTION ( 'NONE',  ( -0.000000000000000000, 1.000000000000000000, -0.000000000000000000 ) ) ;
#23074 = CARTESIAN_POINT ( 'NONE',  ( 15.47797589786117634, -7.092492006142043337, 7.272049892295485485 ) ) ;
#23075 = CARTESIAN_POINT ( 'NONE',  ( -13.92530307126622269, 9.878387810998201957, 6.131018562779544823 ) ) ;
#23076 = CARTESIAN_POINT ( 'NONE',  ( 3.146565092309292933, 16.78275473100423554, 18.92976555901915603 ) ) ;
#23077 = ORIENTED_EDGE ( 'NONE', *, *, #14740, .T. ) ;
#23078 = ORIENTED_EDGE ( 'NONE', *, *, #3472, .F. ) ;
#23079 = CARTESIAN_POINT ( 'NONE',  ( -40.00000000000002842, 80.00000000000001421, 57.50000000000015632 ) ) ;
#23080 = EDGE_CURVE ( 'NONE', #681, #14465, #7297, .T. ) ;
#23081 = DIRECTION ( 'NONE',  ( -0.000000000000000000, -0.000000000000000000, -1.000000000000000000 ) ) ;
#23082 = EDGE_CURVE ( 'NONE', #23209, #15949, #13668, .T. ) ;
#23083 = B_SPLINE_SURFACE_WITH_KNOTS ( 'NONE', 3, 1, ( 
 ( #23610, #20965 ),
 ( #6637, #9448 ),
 ( #25669, #13818 ),
 ( #2253, #6950 ),
 ( #27866, #20669 ),
 ( #30191, #28324 ),
 ( #6784, #11773 ),
 ( #23320, #25521 ),
 ( #16307, #11482 ),
 ( #13674, #23158 ),
 ( #30489, #11328 ),
 ( #21274, #20825 ),
 ( #8989, #18504 ),
 ( #28006, #18650 ),
 ( #4458, #13966 ),
 ( #23464, #11625 ),
 ( #24233, #22050 ),
 ( #19712, #19566 ),
 ( #9739, #26747 ),
 ( #531, #19415 ),
 ( #225, #21903 ),
 ( #29083, #16921 ),
 ( #7877, #17384 ),
 ( #26436, #2578 ),
 ( #7724, #14250 ),
 ( #12238, #17223 ),
 ( #2885, #14582 ),
 ( #19105, #21741 ),
 ( #24084, #9595 ),
 ( #19251, #28774 ),
 ( #17071, #23769 ) ),
 .UNSPECIFIED., .F., .F., .F.,
 ( 4, 3, 3, 3, 3, 3, 3, 3, 3, 3, 4 ),
 ( 2, 2 ),
 ( 0.000000000000000000, 0.05425176834609614362, 0.1085332949128348518, 0.1623767749169379715, 0.2157504826133058717, 0.2688657508888169789, 0.3218907763505471364, 0.3749548578363334772, 0.4282048033836237666, 0.4818374082110496448, 0.4999999999131651274 ),
 ( 0.000000000000000000, 1.000000000000000000 ),
 .UNSPECIFIED. ) ;
#23084 = CARTESIAN_POINT ( 'NONE',  ( 32.19782014694307293, 14.25394737442116444, 39.78814634291936159 ) ) ;
#23085 = LINE ( 'NONE', #3723, #21246 ) ;
#23086 = VECTOR ( 'NONE', #30479, 1000.000000000000000 ) ;
#23087 = CARTESIAN_POINT ( 'NONE',  ( 12.00027744587103840, 12.12900492888020665, 5.759928666072752890 ) ) ;
#23088 = DIRECTION ( 'NONE',  ( -1.000000000000000000, 0.000000000000000000, 0.000000000000000000 ) ) ;
#23089 = AXIS2_PLACEMENT_3D ( 'NONE', #13065, #29907, #8689 ) ;
#23090 = CARTESIAN_POINT ( 'NONE',  ( 37.16608720827707657, 36.86186943028246787, 12.49999999999999112 ) ) ;
#23091 = EDGE_CURVE ( 'NONE', #22640, #9013, #9990, .T. ) ;
#23092 = VECTOR ( 'NONE', #3427, 1000.000000000000000 ) ;
#23093 = ORIENTED_EDGE ( 'NONE', *, *, #15085, .T. ) ;
#23094 = CARTESIAN_POINT ( 'NONE',  ( 1.236176367852860336, -19.96182836857062171, 7.161525567826881655 ) ) ;
#23095 = EDGE_CURVE ( 'NONE', #14352, #12655, #4996, .T. ) ;
#23096 = CARTESIAN_POINT ( 'NONE',  ( -34.70577939416727276, 10.49309206033987785, 34.49999999999999289 ) ) ;
#23097 = DIRECTION ( 'NONE',  ( 1.000000000000000000, 0.000000000000000000, 0.000000000000000000 ) ) ;
#23098 = ORIENTED_EDGE ( 'NONE', *, *, #6296, .T. ) ;
#23099 = ADVANCED_FACE ( 'NONE', ( #25901 ), #30724, .F. ) ;
#23100 = CARTESIAN_POINT ( 'NONE',  ( -4.163336342344337027E-14, 1.387778780781445676E-14, 24.50000000000000000 ) ) ;
#23101 = VERTEX_POINT ( 'NONE', #18892 ) ;
#23102 = DIRECTION ( 'NONE',  ( -0.000000000000000000, -0.000000000000000000, 1.000000000000000000 ) ) ;
#23103 = LINE ( 'NONE', #29992, #12529 ) ;
#23104 = ORIENTED_EDGE ( 'NONE', *, *, #6085, .F. ) ;
#23105 = CARTESIAN_POINT ( 'NONE',  ( 0.3518703668723787148, -19.99690444156084723, 7.652108011868850035 ) ) ;
#23106 = CARTESIAN_POINT ( 'NONE',  ( 0.9819813860070594203, 49.99276302178526521, -69.97593018308113244 ) ) ;
#23107 = CARTESIAN_POINT ( 'NONE',  ( 28.37932450449293853, 10.51822134874671022, 1.500000000000000000 ) ) ;
#23108 = FACE_OUTER_BOUND ( 'NONE', #23366, .T. ) ;
#23109 = AXIS2_PLACEMENT_3D ( 'NONE', #14153, #16660, #11671 ) ;
#23110 = DIRECTION ( 'NONE',  ( 0.000000000000000000, 0.000000000000000000, 1.000000000000000000 ) ) ;
#23111 = CARTESIAN_POINT ( 'NONE',  ( 1.342146863054722639, -19.97260970722469509, 6.892848776733236704 ) ) ;
#23112 = DIRECTION ( 'NONE',  ( -1.000000000000000000, 0.000000000000000000, 0.000000000000000000 ) ) ;
#23113 = EDGE_CURVE ( 'NONE', #6919, #19482, #7026, .T. ) ;
#23114 = ORIENTED_EDGE ( 'NONE', *, *, #17973, .T. ) ;
#23115 = EDGE_CURVE ( 'NONE', #11459, #25155, #28871, .T. ) ;
#23116 = DIRECTION ( 'NONE',  ( -1.000000000000000000, -0.000000000000000000, -0.000000000000000000 ) ) ;
#23117 = CARTESIAN_POINT ( 'NONE',  ( -7.488956955540436056, -5.141690706682852330, 13.22130136205108819 ) ) ;
#23118 = CYLINDRICAL_SURFACE ( 'NONE', #30216, 9.482273699623480212 ) ;
#23119 = ADVANCED_FACE ( 'NONE', ( #11869 ), #10633, .T. ) ;
#23120 = VERTEX_POINT ( 'NONE', #13108 ) ;
#23121 = LINE ( 'NONE', #11282, #7076 ) ;
#23122 = CARTESIAN_POINT ( 'NONE',  ( -17.73231296732453188, -9.288543855440106967, 18.64703902303423178 ) ) ;
#23123 = EDGE_CURVE ( 'NONE', #30496, #3050, #17777, .T. ) ;
#23124 = EDGE_CURVE ( 'NONE', #24186, #466, #5766, .T. ) ;
#23125 =( NAMED_UNIT ( * ) PLANE_ANGLE_UNIT ( ) SI_UNIT ( $, .RADIAN. ) );
#23126 = CARTESIAN_POINT ( 'NONE',  ( -50.00000000000000000, -50.00000000000000000, 12.49999999999999112 ) ) ;
#23127 = EDGE_LOOP ( 'NONE', ( #6741, #20467, #28867, #13127 ) ) ;
#23128 = CARTESIAN_POINT ( 'NONE',  ( 7.562559277181973627, -5.881244434206257310, 1.500000000000001332 ) ) ;
#23129 = CARTESIAN_POINT ( 'NONE',  ( -19.64114023396061981, 37.13592150528867109, -1.500000000000000000 ) ) ;
#23130 = CARTESIAN_POINT ( 'NONE',  ( 38.48713303109791894, -7.360220187875558651, 35.02549194227622564 ) ) ;
#23131 = EDGE_CURVE ( 'NONE', #9013, #19648, #26670, .T. ) ;
#23132 = CARTESIAN_POINT ( 'NONE',  ( -40.00000000000002842, 80.00000000000001421, 17.49999999999982947 ) ) ;
#23133 = ORIENTED_EDGE ( 'NONE', *, *, #22111, .F. ) ;
#23134 = DIRECTION ( 'NONE',  ( 1.000000000000000000, 0.000000000000000000, 0.000000000000000000 ) ) ;
#23135 = CARTESIAN_POINT ( 'NONE',  ( -35.76344986165608475, 22.29344514668535027, -19.50000000000000355 ) ) ;
#23136 = CARTESIAN_POINT ( 'NONE',  ( -14.41708049311053053, 17.22181377296911720, -1.500000000000000000 ) ) ;
#23137 = CIRCLE ( 'NONE', #30138, 1.447898107987198646 ) ;
#23138 = VERTEX_POINT ( 'NONE', #29161 ) ;
#23139 = CARTESIAN_POINT ( 'NONE',  ( -10.59559327413201046, -40.90840839550211427, 28.97918858187435021 ) ) ;
#23140 = ORIENTED_EDGE ( 'NONE', *, *, #1623, .F. ) ;
#23141 = CARTESIAN_POINT ( 'NONE',  ( -32.14095006730909176, -14.40137518142634576, 39.78046893946850560 ) ) ;
#23142 = EDGE_CURVE ( 'NONE', #18090, #7470, #24357, .T. ) ;
#23143 = CARTESIAN_POINT ( 'NONE',  ( -10.32985675426555616, -17.14655349859504341, 5.678370764302467677 ) ) ;
#23144 = CONICAL_SURFACE ( 'NONE', #27153, 5.035999999999999588, 0.7853981633974388421 ) ;
#23145 = EDGE_CURVE ( 'NONE', #26358, #8889, #22138, .T. ) ;
#23146 = DIRECTION ( 'NONE',  ( 0.000000000000000000, 0.000000000000000000, 1.000000000000000000 ) ) ;
#23147 = VERTEX_POINT ( 'NONE', #8267 ) ;
#23148 = DIRECTION ( 'NONE',  ( 0.7557495743542582689, -0.6548607339452849896, 0.000000000000000000 ) ) ;
#23149 = CARTESIAN_POINT ( 'NONE',  ( 16.55530288949897866, 4.194058762902721504, 6.783738457429058677 ) ) ;
#23150 = DIRECTION ( 'NONE',  ( 0.000000000000000000, 0.000000000000000000, 1.000000000000000000 ) ) ;
#23151 = CARTESIAN_POINT ( 'NONE',  ( -46.43819574214524692, 69.68628862962340520, 14.81935245954445435 ) ) ;
#23152 = CARTESIAN_POINT ( 'NONE',  ( 31.29501345865701012, -26.27841684422097401, -6.499999999999999112 ) ) ;
#23153 = CARTESIAN_POINT ( 'NONE',  ( -12.84881549446081017, 11.17046077483154853, 19.96344307082653202 ) ) ;
#23154 = CIRCLE ( 'NONE', #1773, 0.7500000000000006661 ) ;
#23155 = DIRECTION ( 'NONE',  ( -0.000000000000000000, 0.000000000000000000, 1.000000000000000000 ) ) ;
#23156 = CARTESIAN_POINT ( 'NONE',  ( 3.188743458504121442, 16.77324615162856958, 18.84329447212444464 ) ) ;
#23157 = DIRECTION ( 'NONE',  ( 0.000000000000000000, 1.000000000000000000, 0.000000000000000000 ) ) ;
#23158 = CARTESIAN_POINT ( 'NONE',  ( -15.51938817160314876, -6.998174447281577670, 19.87181966307587544 ) ) ;
#23159 = FACE_OUTER_BOUND ( 'NONE', #15934, .T. ) ;
#23160 = ORIENTED_EDGE ( 'NONE', *, *, #20899, .F. ) ;
#23161 = CARTESIAN_POINT ( 'NONE',  ( 0.000000000000000000, -2.435693370351110282E-15, 21.50000000000000355 ) ) ;
#23162 = CARTESIAN_POINT ( 'NONE',  ( 34.07766914600081520, 21.40380666527109810, -1.500000000000000000 ) ) ;
#23163 = DIRECTION ( 'NONE',  ( 1.000000000000000000, 0.000000000000000000, 0.000000000000000000 ) ) ;
#23164 = ORIENTED_EDGE ( 'NONE', *, *, #10090, .T. ) ;
#23165 = DIRECTION ( 'NONE',  ( 1.000000000000000000, 0.000000000000000000, 0.000000000000000000 ) ) ;
#23166 = CARTESIAN_POINT ( 'NONE',  ( -6.312773474853920597, 15.86096687809345696, 19.96568007040468729 ) ) ;
#23167 = CARTESIAN_POINT ( 'NONE',  ( 37.16608720827707657, 65.00000000000000000, 50.49999999999998579 ) ) ;
#23168 = ORIENTED_EDGE ( 'NONE', *, *, #18702, .T. ) ;
#23169 = DIRECTION ( 'NONE',  ( 1.000000000000000000, -0.000000000000000000, 0.000000000000000000 ) ) ;
#23170 = CARTESIAN_POINT ( 'NONE',  ( -10.82521593960875528, 5.400395169024524655, 1.500000000000001332 ) ) ;
#23171 = FACE_OUTER_BOUND ( 'NONE', #30819, .T. ) ;
#23172 = ORIENTED_EDGE ( 'NONE', *, *, #7568, .T. ) ;
#23173 = DIRECTION ( 'NONE',  ( 1.000000000000000000, 0.000000000000000000, 0.000000000000000000 ) ) ;
#23174 = CIRCLE ( 'NONE', #24695, 0.7500000000000002220 ) ;
#23175 = ORIENTED_EDGE ( 'NONE', *, *, #9642, .F. ) ;
#23176 = CARTESIAN_POINT ( 'NONE',  ( -15.16307827826492627, -7.786259562520722710, 5.652196082368482699 ) ) ;
#23177 = DIRECTION ( 'NONE',  ( 0.6707505147970127535, 0.7416830501633041584, 0.000000000000000000 ) ) ;
#23178 = EDGE_CURVE ( 'NONE', #3110, #2473, #2975, .T. ) ;
#23179 = EDGE_LOOP ( 'NONE', ( #25430, #28968, #5198, #14080 ) ) ;
#23180 = EDGE_CURVE ( 'NONE', #29503, #24153, #22150, .T. ) ;
#23181 = DIRECTION ( 'NONE',  ( 1.000000000000000000, 0.000000000000000000, 0.000000000000000000 ) ) ;
#23182 = CARTESIAN_POINT ( 'NONE',  ( -25.47847050916410439, -26.57182937991348481, 26.54355021145563143 ) ) ;
#23183 = CYLINDRICAL_SURFACE ( 'NONE', #12116, 0.7500000000000002220 ) ;
#23184 = CARTESIAN_POINT ( 'NONE',  ( 19.74942470869275368, 3.267558643021993170, 7.652108011868850035 ) ) ;
#23185 = AXIS2_PLACEMENT_3D ( 'NONE', #6629, #30183, #25660 ) ;
#23186 = DIRECTION ( 'NONE',  ( 1.000000000000000000, 0.000000000000000000, 0.000000000000000000 ) ) ;
#23187 = CARTESIAN_POINT ( 'NONE',  ( -17.05026832885478072, 0.8441673869077329639, 18.73314399819311760 ) ) ;
#23188 = CARTESIAN_POINT ( 'NONE',  ( 3.196529495465388226, 8.413215745755008967, 1.500000000000001332 ) ) ;
#23189 = ORIENTED_EDGE ( 'NONE', *, *, #7075, .T. ) ;
#23190 = CARTESIAN_POINT ( 'NONE',  ( 9.984725267469515941, -13.82013960671582531, 20.33971507717571114 ) ) ;
#23191 = DIRECTION ( 'NONE',  ( -0.000000000000000000, -0.000000000000000000, 1.000000000000000000 ) ) ;
#23192 = ORIENTED_EDGE ( 'NONE', *, *, #8469, .F. ) ;
#23193 = VERTEX_POINT ( 'NONE', #15424 ) ;
#23194 = B_SPLINE_CURVE_WITH_KNOTS ( 'NONE', 3,
 ( #1526, #14405, #4012, #2398, #18208, #15701, #15866, #29915, #28451, #27722, #21095, #9262, #10882, #14082, #23590, #11035 ),
 .UNSPECIFIED., .F., .F.,
 ( 4, 2, 2, 2, 2, 2, 2, 4 ),
 ( 2.980374332640320740E-07, 0.0009280375596593466898, 0.001391907320772395144, 0.001855777081885443599, 0.002319646842998492053, 0.002783516604111547880, 0.003247386365224604141, 0.003711256126337660836 ),
 .UNSPECIFIED. ) ;
#23195 = VECTOR ( 'NONE', #9662, 1000.000000000000000 ) ;
#23196 = DIRECTION ( 'NONE',  ( -0.000000000000000000, -0.000000000000000000, 1.000000000000000000 ) ) ;
#23197 =( NAMED_UNIT ( * ) PLANE_ANGLE_UNIT ( ) SI_UNIT ( $, .RADIAN. ) );
#23198 = ORIENTED_EDGE ( 'NONE', *, *, #6167, .F. ) ;
#23199 = VECTOR ( 'NONE', #16523, 1000.000000000000000 ) ;
#23200 = CARTESIAN_POINT ( 'NONE',  ( -12.97606618380807220, 11.02883152178847936, 5.848946451764558851 ) ) ;
#23201 = ORIENTED_EDGE ( 'NONE', *, *, #26926, .F. ) ;
#23202 = B_SPLINE_CURVE_WITH_KNOTS ( 'NONE', 3,
 ( #1279, #8750, #15612, #4373, #9062, #20303, #16081, #23232, #20594, #11409, #15770, #30425, #1886, #3936, #13456, #25451 ),
 .UNSPECIFIED., .F., .F.,
 ( 4, 2, 2, 2, 2, 2, 2, 4 ),
 ( 0.4999999999999997224, 0.6249999999999995559, 0.6874999999999995559, 0.7187499999999995559, 0.7499999999999995559, 0.8124999999999995559, 0.8749999999999997780, 1.000000000000000000 ),
 .UNSPECIFIED. ) ;
#23203 = CARTESIAN_POINT ( 'NONE',  ( -40.00000000000000000, 90.00000000000001421, 22.49999999999999289 ) ) ;
#23204 = VECTOR ( 'NONE', #28960, 1000.000000000000000 ) ;
#23205 = LINE ( 'NONE', #8729, #2025 ) ;
#23206 = ORIENTED_EDGE ( 'NONE', *, *, #10926, .F. ) ;
#23207 = LINE ( 'NONE', #11386, #17810 ) ;
#23208 = AXIS2_PLACEMENT_3D ( 'NONE', #651, #9551, #9863 ) ;
#23209 = VERTEX_POINT ( 'NONE', #1250 ) ;
#23210 = CARTESIAN_POINT ( 'NONE',  ( -26.41394434536923441, 32.09691347257119531, -6.500000000000000888 ) ) ;
#23211 = ORIENTED_EDGE ( 'NONE', *, *, #19086, .T. ) ;
#23212 = ORIENTED_EDGE ( 'NONE', *, *, #15462, .F. ) ;
#23213 = AXIS2_PLACEMENT_3D ( 'NONE', #7676, #26696, #5327 ) ;
#23214 = EDGE_CURVE ( 'NONE', #27034, #26243, #24361, .T. ) ;
#23215 = AXIS2_PLACEMENT_3D ( 'NONE', #23640, #2282, #11804 ) ;
#23216 = LINE ( 'NONE', #16673, #10096 ) ;
#23217 = CARTESIAN_POINT ( 'NONE',  ( 0.3570196857253589706, -9.540868182094921934, -1.474731560294328947 ) ) ;
#23218 = AXIS2_PLACEMENT_3D ( 'NONE', #28598, #4579, #16735 ) ;
#23219 = CARTESIAN_POINT ( 'NONE',  ( -27.03943647958861263, -26.20092231554396278, 27.50000000000000355 ) ) ;
#23220 = CARTESIAN_POINT ( 'NONE',  ( 9.411519254647286559, -14.19511874370440907, 18.49267272388512140 ) ) ;
#23221 = CARTESIAN_POINT ( 'NONE',  ( 16.87696675355429576, 2.215034284604904702, 19.11611934778430921 ) ) ;
#23222 = ORIENTED_EDGE ( 'NONE', *, *, #30716, .T. ) ;
#23223 = CARTESIAN_POINT ( 'NONE',  ( -19.75759631649036763, 3.218781778493906121, 20.05479082170252525 ) ) ;
#23224 = CARTESIAN_POINT ( 'NONE',  ( 15.59193442375635819, -6.853442328767825664, 5.796888747622817029 ) ) ;
#23225 = CARTESIAN_POINT ( 'NONE',  ( -15.98876933090331498, 12.04425525511917527, 6.560937769032974209 ) ) ;
#23226 = VECTOR ( 'NONE', #26269, 1000.000000000000000 ) ;
#23227 = CARTESIAN_POINT ( 'NONE',  ( 1.000000000000008438, 15.73749217771910125, 24.50000000000000000 ) ) ;
#23228 = ORIENTED_EDGE ( 'NONE', *, *, #6720, .T. ) ;
#23229 = SHAPE_REPRESENTATION ( 'Slotted Rotor Drive Shaft', ( #7396 ), #11893 ) ;
#23230 = VERTEX_POINT ( 'NONE', #26995 ) ;
#23231 = CYLINDRICAL_SURFACE ( 'NONE', #12809, 6.000000000000005329 ) ;
#23232 = CARTESIAN_POINT ( 'NONE',  ( 10.68714603012076303, -13.32085008213842769, 6.521906765011492801 ) ) ;
#23233 = CARTESIAN_POINT ( 'NONE',  ( 12.98116905408885557, 11.01127998641985428, 6.973843882838225205 ) ) ;
#23234 = LINE ( 'NONE', #7025, #16118 ) ;
#23235 = CIRCLE ( 'NONE', #27242, 6.000000000000005329 ) ;
#23236 = CARTESIAN_POINT ( 'NONE',  ( -16.53781638505575557, 35.10828276421680272, 27.49999999999999645 ) ) ;
#23237 = CIRCLE ( 'NONE', #26231, 0.7499999999999997780 ) ;
#23238 = ITEM_DEFINED_TRANSFORMATION ( 'NONE', 'NONE', #17869,  #7396 ) ;
#23239 = CARTESIAN_POINT ( 'NONE',  ( 24.03057240117691862, 26.57182937991349903, -6.499999999999999112 ) ) ;
#23240 = ORIENTED_EDGE ( 'NONE', *, *, #9962, .F. ) ;
#23241 = VECTOR ( 'NONE', #6370, 1000.000000000000000 ) ;
#23242 = CARTESIAN_POINT ( 'NONE',  ( -19.95735252415838445, 1.552219945263930700, 6.995624166085161910 ) ) ;
#23243 = CARTESIAN_POINT ( 'NONE',  ( -6.974883619896829146, -5.687793815610328707, -1.500000000000002220 ) ) ;
#23244 = CARTESIAN_POINT ( 'NONE',  ( -6.630478080506954974, -6.778663211761442930, 1.500000000000001332 ) ) ;
#23245 = ORIENTED_EDGE ( 'NONE', *, *, #12865, .F. ) ;
#23246 = DIRECTION ( 'NONE',  ( -1.000000000000000000, 0.000000000000000000, 0.000000000000000000 ) ) ;
#23247 = ADVANCED_FACE ( 'NONE', ( #24947 ), #12953, .F. ) ;
#23248 = ORIENTED_EDGE ( 'NONE', *, *, #587, .F. ) ;
#23249 = EDGE_CURVE ( 'NONE', #10311, #15107, #17310, .T. ) ;
#23250 = DIRECTION ( 'NONE',  ( 1.000000000000000000, 0.000000000000000000, 0.000000000000000000 ) ) ;
#23251 = DIRECTION ( 'NONE',  ( -0.4154150130018840481, 0.9096319953545194403, 0.000000000000000000 ) ) ;
#23252 = AXIS2_PLACEMENT_3D ( 'NONE', #23848, #16842, #7017 ) ;
#23253 = EDGE_CURVE ( 'NONE', #12636, #34, #8118, .T. ) ;
#23254 = VERTEX_POINT ( 'NONE', #22599 ) ;
#23255 = CARTESIAN_POINT ( 'NONE',  ( -0.2664633505551967652, -19.99844781589863274, 7.454139397117730326 ) ) ;
#23256 = EDGE_CURVE ( 'NONE', #8747, #8832, #19494, .T. ) ;
#23257 = DIRECTION ( 'NONE',  ( 0.000000000000000000, 0.000000000000000000, 1.000000000000000000 ) ) ;
#23258 = EDGE_CURVE ( 'NONE', #14232, #5725, #25256, .T. ) ;
#23259 = PLANE ( 'NONE',  #5601 ) ;
#23260 = CYLINDRICAL_SURFACE ( 'NONE', #10371, 2.061368542273053883 ) ;
#23261 = VECTOR ( 'NONE', #13432, 1000.000000000000114 ) ;
#23262 = DIRECTION ( 'NONE',  ( 0.000000000000000000, 0.000000000000000000, 1.000000000000000000 ) ) ;
#23263 = CIRCLE ( 'NONE', #6338, 0.7499999999999997780 ) ;
#23264 = CARTESIAN_POINT ( 'NONE',  ( -18.04365185506138047, -8.627086862512674870, 20.34789198813115263 ) ) ;
#23265 = CARTESIAN_POINT ( 'NONE',  ( 0.000000000000000000, -1.324687536737320328E-14, 29.43090101791767665 ) ) ;
#23266 = EDGE_CURVE ( 'NONE', #15211, #21613, #9038, .T. ) ;
#23267 = ORIENTED_EDGE ( 'NONE', *, *, #12144, .F. ) ;
#23268 = AXIS2_PLACEMENT_3D ( 'NONE', #18579, #8749, #16080 ) ;
#23269 = EDGE_CURVE ( 'NONE', #20491, #12536, #22869, .T. ) ;
#23270 = CARTESIAN_POINT ( 'NONE',  ( 5.374868878255610660, 44.10336124695606230, -19.50000000000000355 ) ) ;
#23271 = DIRECTION ( 'NONE',  ( -1.000000000000000000, 0.000000000000000000, 0.000000000000000000 ) ) ;
#23272 = VERTEX_POINT ( 'NONE', #8583 ) ;
#23273 = DIRECTION ( 'NONE',  ( -0.000000000000000000, -0.000000000000000000, -1.000000000000000000 ) ) ;
#23274 = EDGE_CURVE ( 'NONE', #16043, #22829, #21372, .T. ) ;
#23275 = CARTESIAN_POINT ( 'NONE',  ( -17.66624025659153574, -9.413543259203217772, 18.82680253904184298 ) ) ;
#23276 = CARTESIAN_POINT ( 'NONE',  ( -19.64114023396299302, -37.13592150529018454, -1.500000000000000000 ) ) ;
#23277 = CIRCLE ( 'NONE', #9841, 0.7500000000000006661 ) ;
#23278 = ADVANCED_BREP_SHAPE_REPRESENTATION ( '', ( #3432, #7396 ), #15375 ) ;
#23279 = DIRECTION ( 'NONE',  ( 0.000000000000000000, 0.000000000000000000, -1.000000000000000000 ) ) ;
#23280 = VECTOR ( 'NONE', #17569, 1000.000000000000000 ) ;
#23281 = ORIENTED_EDGE ( 'NONE', *, *, #10695, .F. ) ;
#23282 = CARTESIAN_POINT ( 'NONE',  ( -9.033033306777449312, 0.9621688436940325495, -1.500000000000001554 ) ) ;
#23283 = CARTESIAN_POINT ( 'NONE',  ( 11.40980092660686118, 6.310027164379057751, 24.50000000000000000 ) ) ;
#23284 = CARTESIAN_POINT ( 'NONE',  ( 17.34672660037420044, -33.26777931996199555, 37.50000000003682032 ) ) ;
#23285 = LINE ( 'NONE', #1928, #630 ) ;
#23286 = ORIENTED_EDGE ( 'NONE', *, *, #3506, .T. ) ;
#23287 = DIRECTION ( 'NONE',  ( 0.000000000000000000, 0.000000000000000000, 1.000000000000000000 ) ) ;
#23288 = AXIS2_PLACEMENT_3D ( 'NONE', #3401, #2124, #11352 ) ;
#23289 = DIRECTION ( 'NONE',  ( 1.000000000000000000, 0.000000000000000000, 0.000000000000000000 ) ) ;
#23290 = DIRECTION ( 'NONE',  ( 1.000000000000000000, 0.000000000000000000, 0.000000000000000000 ) ) ;
#23291 = AXIS2_PLACEMENT_3D ( 'NONE', #21302, #23344, #25689 ) ;
#23292 = EDGE_CURVE ( 'NONE', #19042, #17054, #19898, .T. ) ;
#23293 = ORIENTED_EDGE ( 'NONE', *, *, #7815, .T. ) ;
#23294 = ADVANCED_FACE ( 'NONE', ( #15736 ), #8726, .F. ) ;
#23295 = ADVANCED_FACE ( 'NONE', ( #15584, #20712 ), #13714, .T. ) ;
#23296 = ADVANCED_FACE ( 'NONE', ( #6681 ), #16196, .T. ) ;
#23297 = CARTESIAN_POINT ( 'NONE',  ( -8.413215745754975217, 3.196529495465474380, 21.50000000000000000 ) ) ;
#23298 = VERTEX_POINT ( 'NONE', #27761 ) ;
#23299 = CARTESIAN_POINT ( 'NONE',  ( -24.58208797071834439, -7.298293523701636865, 45.11515778355300199 ) ) ;
#23300 = CIRCLE ( 'NONE', #8873, 53.00000000000000711 ) ;
#23301 = EDGE_CURVE ( 'NONE', #16368, #1375, #3903, .T. ) ;
#23302 = DIRECTION ( 'NONE',  ( -2.312964634635740689E-15, 1.000000000000000000, 0.000000000000000000 ) ) ;
#23303 = CIRCLE ( 'NONE', #18339, 2.061368542273053883 ) ;
#23304 = CARTESIAN_POINT ( 'NONE',  ( 31.10500197267672462, -15.38309308716404722, 40.29910134388152443 ) ) ;
#23305 = VECTOR ( 'NONE', #20249, 1000.000000000000000 ) ;
#23306 = ORIENTED_EDGE ( 'NONE', *, *, #1089, .F. ) ;
#23307 = EDGE_CURVE ( 'NONE', #17402, #1784, #10216, .T. ) ;
#23308 = CARTESIAN_POINT ( 'NONE',  ( 23.21076833940160000, 12.23288291591659771, 44.52046879181326489 ) ) ;
#23309 = CARTESIAN_POINT ( 'NONE',  ( 16.65321191609847418, 3.713086718183620683, 7.545655578832111132 ) ) ;
#23310 = CARTESIAN_POINT ( 'NONE',  ( -10.47960520055065636, -7.757439966934454034, 1.500000000000001332 ) ) ;
#23311 = CARTESIAN_POINT ( 'NONE',  ( -13.33237335330699125, 10.61702797731129877, 18.34969686940296185 ) ) ;
#23312 = ADVANCED_FACE ( 'NONE', ( #4044 ), #23051, .F. ) ;
#23313 = CARTESIAN_POINT ( 'NONE',  ( -43.31339426922971114, 68.85174796075946801, 13.05946217696219236 ) ) ;
#23314 = CIRCLE ( 'NONE', #9871, 21.71568325578202163 ) ;
#23315 = CARTESIAN_POINT ( 'NONE',  ( -14.44122519041009234, -13.83658248990211348, 24.50000000000000000 ) ) ;
#23316 = DIRECTION ( 'NONE',  ( -0.000000000000000000, 1.132880637372608986E-16, -1.000000000000000000 ) ) ;
#23317 = LINE ( 'NONE', #20822, #17510 ) ;
#23318 = CARTESIAN_POINT ( 'NONE',  ( 13.72236183117461295, 39.79315620192736702, 21.95836815899282612 ) ) ;
#23319 = CARTESIAN_POINT ( 'NONE',  ( 49.99999999999998579, 209.2686044187655909, -75.50000000000001421 ) ) ;
#23320 = CARTESIAN_POINT ( 'NONE',  ( -18.36135251343598185, -7.973951480934446501, 20.05479082170252525 ) ) ;
#23321 = FACE_OUTER_BOUND ( 'NONE', #7756, .T. ) ;
#23322 = ORIENTED_EDGE ( 'NONE', *, *, #29812, .T. ) ;
#23323 = VERTEX_POINT ( 'NONE', #10923 ) ;
#23324 = LINE ( 'NONE', #11487, #2000 ) ;
#23325 = CARTESIAN_POINT ( 'NONE',  ( -34.07766914599911701, 21.40380666528009002, -1.500000000000000000 ) ) ;
#23326 = EDGE_CURVE ( 'NONE', #2857, #10874, #13611, .T. ) ;
#23327 = CARTESIAN_POINT ( 'NONE',  ( -44.99999999999955236, -4.926614671774132148E-13, 57.49999999999999289 ) ) ;
#23328 = ORIENTED_EDGE ( 'NONE', *, *, #5768, .T. ) ;
#23329 = AXIS2_PLACEMENT_3D ( 'NONE', #16449, #30477, #30337 ) ;
#23330 = EDGE_CURVE ( 'NONE', #4711, #18115, #8475, .T. ) ;
#23331 = CARTESIAN_POINT ( 'NONE',  ( 18.09058649146511044, -8.570415951004784816, 18.55820869691756769 ) ) ;
#23332 = AXIS2_PLACEMENT_3D ( 'NONE', #6668, #11367, #14142 ) ;
#23333 = DIRECTION ( 'NONE',  ( 0.000000000000000000, 1.000000000000000000, 1.193512090021232842E-16 ) ) ;
#23334 = ORIENTED_EDGE ( 'NONE', *, *, #127, .F. ) ;
#23335 = DIRECTION ( 'NONE',  ( -0.000000000000000000, -0.000000000000000000, 1.000000000000000000 ) ) ;
#23336 = LINE ( 'NONE', #24796, #15706 ) ;
#23337 = VECTOR ( 'NONE', #86, 1000.000000000000000 ) ;
#23338 = CARTESIAN_POINT ( 'NONE',  ( 4.510281037539698445E-13, -4.926614671774132148E-13, 62.49999999999999289 ) ) ;
#23339 = EDGE_CURVE ( 'NONE', #19467, #19119, #15427, .T. ) ;
#23340 = CARTESIAN_POINT ( 'NONE',  ( -8.549050687778191104, -4.102102735472429096, 21.50000000000000000 ) ) ;
#23341 = ORIENTED_EDGE ( 'NONE', *, *, #232, .F. ) ;
#23342 = CYLINDRICAL_SURFACE ( 'NONE', #8885, 15.00000000000000000 ) ;
#23343 = DIRECTION ( 'NONE',  ( -0.000000000000000000, -0.000000000000000000, -1.000000000000000000 ) ) ;
#23344 = DIRECTION ( 'NONE',  ( 0.000000000000000000, 0.000000000000000000, 1.000000000000000000 ) ) ;
#23345 = ORIENTED_EDGE ( 'NONE', *, *, #18174, .T. ) ;
#23346 = DIRECTION ( 'NONE',  ( 1.000000000000000000, 0.000000000000000000, 0.000000000000000000 ) ) ;
#23347 = PRODUCT_DEFINITION_FORMATION_WITH_SPECIFIED_SOURCE ( 'ANY', '', #4943, .NOT_KNOWN. ) ;
#23348 = B_SPLINE_CURVE_WITH_KNOTS ( 'NONE', 3,
 ( #11326, #30635, #29778, #11478 ),
 .UNSPECIFIED., .F., .F.,
 ( 4, 4 ),
 ( 0.000000000000000000, 0.005028157979160071712 ),
 .UNSPECIFIED. ) ;
#23349 = DIRECTION ( 'NONE',  ( -0.000000000000000000, -0.000000000000000000, -1.000000000000000000 ) ) ;
#23350 = PRODUCT_DEFINITION_SHAPE ( 'NONE', 'NONE',  #12777 ) ;
#23351 = CARTESIAN_POINT ( 'NONE',  ( 35.00000000000000000, 90.00000000000001421, -22.50000000000002487 ) ) ;
#23352 = AXIS2_PLACEMENT_3D ( 'NONE', #10275, #8682, #20373 ) ;
#23353 = AXIS2_PLACEMENT_3D ( 'NONE', #16693, #10244, #7932 ) ;
#23354 = DIRECTION ( 'NONE',  ( 0.000000000000000000, 0.000000000000000000, 1.000000000000000000 ) ) ;
#23355 = CARTESIAN_POINT ( 'NONE',  ( -16.99143801116384722, 1.432169416036907617, 20.32367522806703874 ) ) ;
#23356 = CARTESIAN_POINT ( 'NONE',  ( -12.54846374865995706, -9.550116103605043705, 24.50000000000000000 ) ) ;
#23357 = ORIENTED_EDGE ( 'NONE', *, *, #25955, .T. ) ;
#23358 = CARTESIAN_POINT ( 'NONE',  ( 4.622016212553096359, -12.19167610014704906, 1.500000000000001332 ) ) ;
#23359 = AXIS2_PLACEMENT_3D ( 'NONE', #28479, #12101, #12412 ) ;
#23360 = CARTESIAN_POINT ( 'NONE',  ( 32.31576317091162309, 17.59561277345964214, 27.49999999999999645 ) ) ;
#23361 = VERTEX_POINT ( 'NONE', #14628 ) ;
#23362 = VERTEX_POINT ( 'NONE', #6993 ) ;
#23363 = CARTESIAN_POINT ( 'NONE',  ( -49.48635302761310584, 69.99362080440305078, 55.68038323789210864 ) ) ;
#23364 = ADVANCED_FACE ( 'NONE', ( #30540 ), #4504, .T. ) ;
#23365 = CARTESIAN_POINT ( 'NONE',  ( -3.196529495465446402, -8.413215745754985875, -1.500000000000002665 ) ) ;
#23366 = EDGE_LOOP ( 'NONE', ( #3150, #14497, #14411, #3319 ) ) ;
#23367 = VECTOR ( 'NONE', #30605, 1000.000000000000000 ) ;
#23368 = CARTESIAN_POINT ( 'NONE',  ( -12.79825419737478676, 11.22575876280636642, 7.156916968540300239 ) ) ;
#23369 = CARTESIAN_POINT ( 'NONE',  ( 23.26155266345718431, 12.35118985415806847, 48.66282223823449726 ) ) ;
#23370 = ORIENTED_EDGE ( 'NONE', *, *, #20075, .F. ) ;
#23371 = CARTESIAN_POINT ( 'NONE',  ( -8.197313248159920462, 3.914781618004780306, -1.500000000000001332 ) ) ;
#23372 = DIRECTION ( 'NONE',  ( 0.000000000000000000, -1.132880637372608986E-16, 1.000000000000000000 ) ) ;
#23373 = ORIENTED_EDGE ( 'NONE', *, *, #16587, .T. ) ;
#23374 = DIRECTION ( 'NONE',  ( 1.000000000000000000, 0.000000000000000000, 0.000000000000000000 ) ) ;
#23375 = ORIENTED_EDGE ( 'NONE', *, *, #13952, .F. ) ;
#23376 = CARTESIAN_POINT ( 'NONE',  ( -29.15452456067305675, 29.11038375075762730, -6.500000000000000888 ) ) ;
#23377 = MANIFOLD_SOLID_BREP ( 'HeadFillet', #2359 ) ;
#23378 = ORIENTED_EDGE ( 'NONE', *, *, #23471, .F. ) ;
#23379 = AXIS2_PLACEMENT_3D ( 'NONE', #9874, #22026, #9563 ) ;
#23380 = ORIENTED_EDGE ( 'NONE', *, *, #7140, .T. ) ;
#23381 = CARTESIAN_POINT ( 'NONE',  ( 1.073881485057738949, -0.9711784013061123266, 1.500000000000000000 ) ) ;
#23382 = DIRECTION ( 'NONE',  ( -0.000000000000000000, 0.000000000000000000, 1.000000000000000000 ) ) ;
#23383 = AXIS2_PLACEMENT_3D ( 'NONE', #26062, #2352, #11883 ) ;
#23384 = DIRECTION ( 'NONE',  ( 0.000000000000000000, 1.000000000000000000, 1.193512090021232842E-16 ) ) ;
#23385 = DIRECTION ( 'NONE',  ( 0.000000000000000000, 0.000000000000000000, 1.000000000000000000 ) ) ;
#23386 = CARTESIAN_POINT ( 'NONE',  ( -6.187077094091591789, 11.47693674426096955, 1.500000000000001332 ) ) ;
#23387 = ORIENTED_EDGE ( 'NONE', *, *, #17557, .T. ) ;
#23388 = CARTESIAN_POINT ( 'NONE',  ( 10.65605551513794502, -16.94611923951457655, 7.500898271101006820 ) ) ;
#23389 = CARTESIAN_POINT ( 'NONE',  ( 24.03448224033878944, -8.660042335149841009, 45.23564988763768469 ) ) ;
#23390 = CARTESIAN_POINT ( 'NONE',  ( -7.730328572437709767, 4.608906612435681005, -3.621320343559650379 ) ) ;
#23391 = CARTESIAN_POINT ( 'NONE',  ( 3.062389757841097904, 16.80148204205676876, 19.36813350477385143 ) ) ;
#23392 = ORIENTED_EDGE ( 'NONE', *, *, #18332, .F. ) ;
#23393 = ORIENTED_EDGE ( 'NONE', *, *, #10139, .F. ) ;
#23394 = DIRECTION ( 'NONE',  ( 0.000000000000000000, 0.000000000000000000, -1.000000000000000000 ) ) ;
#23395 = CARTESIAN_POINT ( 'NONE',  ( -12.56641067637752229, 40.32935944495016400, -1.500000000000009992 ) ) ;
#23396 = CARTESIAN_POINT ( 'NONE',  ( -5.655446062488476144, 19.20259930434394846, 18.39701043959520987 ) ) ;
#23397 = CARTESIAN_POINT ( 'NONE',  ( 24.03057240117691862, -26.57182937991349903, -6.500000000000000888 ) ) ;
#23398 = AXIS2_PLACEMENT_3D ( 'NONE', #24202, #16898, #26414 ) ;
#23399 = ADVANCED_FACE ( 'NONE', ( #14154 ), #28828, .F. ) ;
#23400 = CARTESIAN_POINT ( 'NONE',  ( -2.468401054669552952, 39.50000000000001421, 27.50000000000001421 ) ) ;
#23401 = CARTESIAN_POINT ( 'NONE',  ( 23.20389136007291953, -12.24563090271730736, 48.76343458319715296 ) ) ;
#23402 = ORIENTED_EDGE ( 'NONE', *, *, #8248, .F. ) ;
#23403 = AXIS2_PLACEMENT_3D ( 'NONE', #29906, #6186, #8222 ) ;
#23404 = CARTESIAN_POINT ( 'NONE',  ( -19.86072491926578110, 2.502642356747510899, 7.652108011868850035 ) ) ;
#23405 = DIRECTION ( 'NONE',  ( 0.000000000000000000, -1.132880637372608986E-16, 1.000000000000000000 ) ) ;
#23406 = CARTESIAN_POINT ( 'NONE',  ( 19.78395057425408865, 2.934310293824241356, 20.32243167357989577 ) ) ;
#23407 = VERTEX_POINT ( 'NONE', #7464 ) ;
#23408 = FACE_OUTER_BOUND ( 'NONE', #13376, .T. ) ;
#23409 = VERTEX_POINT ( 'NONE', #23512 ) ;
#23410 = CARTESIAN_POINT ( 'NONE',  ( -4.163336342344337027E-14, -1.387778780781445676E-14, -1.500000000000000000 ) ) ;
#23411 = EDGE_CURVE ( 'NONE', #18893, #8846, #14439, .T. ) ;
#23412 = DIRECTION ( 'NONE',  ( 0.000000000000000000, 0.000000000000000000, 1.000000000000000000 ) ) ;
#23413 = EDGE_LOOP ( 'NONE', ( #9090, #16410, #5620, #13210 ) ) ;
#23414 = LINE ( 'NONE', #25075, #16822 ) ;
#23415 = LINE ( 'NONE', #13915, #18983 ) ;
#23416 = DIRECTION ( 'NONE',  ( 0.000000000000000000, 1.000000000000000000, 0.000000000000000000 ) ) ;
#23417 = CARTESIAN_POINT ( 'NONE',  ( -6.460166075217649961, 15.80732207284229673, 19.03762469184452755 ) ) ;
#23418 = LINE ( 'NONE', #2674, #24289 ) ;
#23419 = CARTESIAN_POINT ( 'NONE',  ( 50.00000000000045475, -4.865382331816764069E-13, 65.49999999999998579 ) ) ;
#23420 = ORIENTED_EDGE ( 'NONE', *, *, #13002, .T. ) ;
#23421 = CARTESIAN_POINT ( 'NONE',  ( 5.296161872597624942, 19.28602264385379428, 20.34789198813115263 ) ) ;
#23422 = CARTESIAN_POINT ( 'NONE',  ( 0.000000000000000000, -2.435693370351110282E-15, 21.50000000000000355 ) ) ;
#23423 = ADVANCED_FACE ( 'NONE', ( #276, #21327, #16661, #2156, #2302, #4961 ), #19005, .F. ) ;
#23424 = ORIENTED_EDGE ( 'NONE', *, *, #18763, .F. ) ;
#23425 = DIRECTION ( 'NONE',  ( -1.000000000000000000, 0.000000000000000000, 0.000000000000000000 ) ) ;
#23426 = LINE ( 'NONE', #2843, #20739 ) ;
#23427 = LINE ( 'NONE', #30456, #22049 ) ;
#23428 = ADVANCED_FACE ( 'NONE', ( #9794 ), #10898, .T. ) ;
#23429 = ORIENTED_EDGE ( 'NONE', *, *, #27289, .T. ) ;
#23430 = CARTESIAN_POINT ( 'NONE',  ( -3.515970705488605130, 17.06554576617236307, 1.500000000000000000 ) ) ;
#23431 = LINE ( 'NONE', #27979, #22607 ) ;
#23432 = CARTESIAN_POINT ( 'NONE',  ( 31.98172739339260673, -24.47984296869126908, 34.62180873253410596 ) ) ;
#23433 = EDGE_CURVE ( 'NONE', #7456, #4466, #1490, .T. ) ;
#23434 = CARTESIAN_POINT ( 'NONE',  ( -12.24063095261064227, 4.490763173670005770, 1.500000000000001332 ) ) ;
#23435 = ORIENTED_EDGE ( 'NONE', *, *, #436, .F. ) ;
#23436 = VECTOR ( 'NONE', #25534, 1000.000000000000000 ) ;
#23437 = CARTESIAN_POINT ( 'NONE',  ( -39.52380524535562500, 7.028748154183637631, -6.500000000000000888 ) ) ;
#23438 = VERTEX_POINT ( 'NONE', #11000 ) ;
#23439 = PLANE ( 'NONE',  #230 ) ;
#23440 = CARTESIAN_POINT ( 'NONE',  ( 0.000000000000000000, 0.000000000000000000, 1.500000000000001332 ) ) ;
#23441 = VERTEX_POINT ( 'NONE', #8802 ) ;
#23442 = PLANE ( 'NONE',  #26326 ) ;
#23443 = ORIENTED_EDGE ( 'NONE', *, *, #23256, .T. ) ;
#23444 = FACE_OUTER_BOUND ( 'NONE', #30615, .T. ) ;
#23445 = EDGE_CURVE ( 'NONE', #12801, #19418, #19922, .T. ) ;
#23446 = CARTESIAN_POINT ( 'NONE',  ( -7.759781818727213398, -15.20954222608249395, 7.098451512883313441 ) ) ;
#23447 = CARTESIAN_POINT ( 'NONE',  ( 29.61203839202725518, -15.40012917324033381, 41.62281023987508632 ) ) ;
#23448 = CARTESIAN_POINT ( 'NONE',  ( 1.512395753140455934, -17.00118538373298804, 18.64703902303423178 ) ) ;
#23449 = VERTEX_POINT ( 'NONE', #15820 ) ;
#23450 = DIRECTION ( 'NONE',  ( 1.000000000000000000, 0.000000000000000000, 0.000000000000000000 ) ) ;
#23451 = CARTESIAN_POINT ( 'NONE',  ( 3.118309183252346628, 17.14266753270391774, 1.500000000000000000 ) ) ;
#23452 = CARTESIAN_POINT ( 'NONE',  ( 0.000000000000000000, 39.50000000000000000, 34.49999999999999289 ) ) ;
#23453 = CARTESIAN_POINT ( 'NONE',  ( 19.54426622602687758, -37.07991288358297055, 1.499999999999999778 ) ) ;
#23454 = VERTEX_POINT ( 'NONE', #18777 ) ;
#23455 = DIRECTION ( 'NONE',  ( 0.000000000000000000, -1.132880637372608986E-16, 1.000000000000000000 ) ) ;
#23456 = VECTOR ( 'NONE', #18225, 1000.000000000000000 ) ;
#23457 = CARTESIAN_POINT ( 'NONE',  ( 30.26724724045159931, -27.72993536917819313, -6.500000000000000000 ) ) ;
#23458 = CARTESIAN_POINT ( 'NONE',  ( -12.97413174816959724, 11.03100730464097090, 20.14907003336613300 ) ) ;
#23459 = DIRECTION ( 'NONE',  ( -0.000000000000000000, 1.132880637372608986E-16, -1.000000000000000000 ) ) ;
#23460 = CARTESIAN_POINT ( 'NONE',  ( 8.806817561695535090, 41.44469761738502456, 20.59405133752780870 ) ) ;
#23461 = DIRECTION ( 'NONE',  ( 0.000000000000000000, 1.132880637372608986E-16, -1.000000000000000000 ) ) ;
#23462 = ADVANCED_FACE ( 'NONE', ( #16432 ), #20797, .F. ) ;
#23463 = ADVANCED_FACE ( 'NONE', ( #16131 ), #25947, .F. ) ;
#23464 = CARTESIAN_POINT ( 'NONE',  ( -18.47028637364417136, -7.717842544976234009, 19.22654678686458141 ) ) ;
#23465 = DIRECTION ( 'NONE',  ( 0.000000000000000000, 1.000000000000000000, -0.000000000000000000 ) ) ;
#23466 = ORIENTED_EDGE ( 'NONE', *, *, #3100, .F. ) ;
#23467 = VERTEX_POINT ( 'NONE', #13941 ) ;
#23468 = CARTESIAN_POINT ( 'NONE',  ( 37.16608720827707657, 65.00000000000000000, 97.07879600563551037 ) ) ;
#23469 = CARTESIAN_POINT ( 'NONE',  ( -7.786278744133511509, -15.19480685133639497, 7.158811349119585721 ) ) ;
#23470 = CARTESIAN_POINT ( 'NONE',  ( -37.16608720827707657, 65.00000000000000000, 50.49999999999998579 ) ) ;
#23471 = EDGE_CURVE ( 'NONE', #11174, #6254, #2076, .T. ) ;
#23472 = VERTEX_POINT ( 'NONE', #1933 ) ;
#23473 = DIRECTION ( 'NONE',  ( 0.000000000000000000, 0.000000000000000000, -1.000000000000000000 ) ) ;
#23474 = CARTESIAN_POINT ( 'NONE',  ( -6.501324370946574227, 15.79217903278910740, 19.21769074125272780 ) ) ;
#23475 = CARTESIAN_POINT ( 'NONE',  ( 0.000000000000000000, 1.699320956058915452E-16, -1.500000000000001776 ) ) ;
#23476 = EDGE_CURVE ( 'NONE', #14300, #6600, #14079, .T. ) ;
#23477 = EDGE_CURVE ( 'NONE', #946, #8162, #7474, .T. ) ;
#23478 = ORIENTED_EDGE ( 'NONE', *, *, #17182, .T. ) ;
#23479 = CARTESIAN_POINT ( 'NONE',  ( -10.62668044795003297, -16.94375577056504412, 20.34789198813115618 ) ) ;
#23480 = CARTESIAN_POINT ( 'NONE',  ( 33.42925964089141644, -11.06161099612213228, -16.55003854064094426 ) ) ;
#23481 = CIRCLE ( 'NONE', #17530, 0.7500000000000002220 ) ;
#23482 = LINE ( 'NONE', #9464, #6378 ) ;
#23483 = CARTESIAN_POINT ( 'NONE',  ( -15.76609453206417832, 34.02993354821598615, 37.50000000001164580 ) ) ;
#23484 = ORIENTED_EDGE ( 'NONE', *, *, #17497, .F. ) ;
#23485 = DIRECTION ( 'NONE',  ( -1.000000000000000000, 0.000000000000000000, 0.000000000000000000 ) ) ;
#23486 = EDGE_CURVE ( 'NONE', #9666, #9137, #29882, .T. ) ;
#23487 = CARTESIAN_POINT ( 'NONE',  ( -15.05112753843571483, -8.020416455010169088, 7.652108011868853588 ) ) ;
#23488 = CARTESIAN_POINT ( 'NONE',  ( 33.42925964089140933, 11.06161099612213405, 35.54550565580007060 ) ) ;
#23489 = ORIENTED_EDGE ( 'NONE', *, *, #7314, .F. ) ;
#23490 = CARTESIAN_POINT ( 'NONE',  ( 8.499586724479435418, 2.959227181723830036, -3.621320343559650379 ) ) ;
#23491 = LINE ( 'NONE', #11650, #19257 ) ;
#23492 = CIRCLE ( 'NONE', #6591, 2.898871837527149609 ) ;
#23493 = CARTESIAN_POINT ( 'NONE',  ( 6.780059429077784472, -43.46078076613360253, -16.50000000000000000 ) ) ;
#23494 = DIRECTION ( 'NONE',  ( 1.000000000000000000, 0.000000000000000000, 0.000000000000000000 ) ) ;
#23495 = CARTESIAN_POINT ( 'NONE',  ( 24.50429677314015819, -7.442113211156453190, 49.39104550111578362 ) ) ;
#23496 = DIRECTION ( 'NONE',  ( 1.000000000000000000, 0.000000000000000000, 0.000000000000000000 ) ) ;
#23497 = CARTESIAN_POINT ( 'NONE',  ( -19.91121867491064279, 2.064381093144386004, 20.25542030744407640 ) ) ;
#23498 = DIRECTION ( 'NONE',  ( 1.000000000000000000, 0.000000000000000000, 0.000000000000000000 ) ) ;
#23499 = EDGE_LOOP ( 'NONE', ( #27599, #11442, #16555, #11208 ) ) ;
#23500 = ADVANCED_FACE ( 'NONE', ( #22984, #18938, #11599 ), #2230, .T. ) ;
#23501 = EDGE_CURVE ( 'NONE', #23911, #6597, #9259, .T. ) ;
#23502 = CARTESIAN_POINT ( 'NONE',  ( 10.50949999207124286, -13.45141484214874517, 19.97651184436794125 ) ) ;
#23503 = AXIS2_PLACEMENT_3D ( 'NONE', #29021, #21847, #16866 ) ;
#23504 = CARTESIAN_POINT ( 'NONE',  ( 0.000000000000000000, 39.50000000000000000, 27.50000000000000355 ) ) ;
#23505 = ORIENTED_EDGE ( 'NONE', *, *, #26972, .T. ) ;
#23506 = EDGE_CURVE ( 'NONE', #5775, #9872, #1493, .T. ) ;
#23507 = ORIENTED_EDGE ( 'NONE', *, *, #28866, .F. ) ;
#23508 = CARTESIAN_POINT ( 'NONE',  ( -15.42727847259665452, 12.72856271945105888, 7.652108011868850923 ) ) ;
#23509 = DIRECTION ( 'NONE',  ( 0.000000000000000000, 1.000000000000000000, 0.000000000000000000 ) ) ;
#23510 = ORIENTED_EDGE ( 'NONE', *, *, #10730, .F. ) ;
#23511 = DIRECTION ( 'NONE',  ( -0.000000000000000000, -0.000000000000000000, 1.000000000000000000 ) ) ;
#23512 = CARTESIAN_POINT ( 'NONE',  ( 66.99999999999998579, -50.00000000000000000, 62.49999999999999289 ) ) ;
#23513 = ORIENTED_EDGE ( 'NONE', *, *, #22557, .T. ) ;
#23514 = AXIS2_PLACEMENT_3D ( 'NONE', #6183, #1808, #15377 ) ;
#23515 = CARTESIAN_POINT ( 'NONE',  ( -16.69721919944057831, 13.88429941593312122, -1.500000000000000000 ) ) ;
#23516 = CARTESIAN_POINT ( 'NONE',  ( 39.99999999999998579, 80.00000000000001421, 22.49999999999999289 ) ) ;
#23517 = ORIENTED_EDGE ( 'NONE', *, *, #25695, .T. ) ;
#23518 = DIRECTION ( 'NONE',  ( -0.000000000000000000, -0.000000000000000000, 1.000000000000000000 ) ) ;
#23519 = VERTEX_POINT ( 'NONE', #28298 ) ;
#23520 = DIRECTION ( 'NONE',  ( -0.000000000000000000, 0.000000000000000000, 1.000000000000000000 ) ) ;
#23521 = ORIENTED_EDGE ( 'NONE', *, *, #9078, .T. ) ;
#23522 = ORIENTED_EDGE ( 'NONE', *, *, #7473, .F. ) ;
#23523 = EDGE_CURVE ( 'NONE', #23828, #29162, #18917, .T. ) ;
#23524 = CYLINDRICAL_SURFACE ( 'NONE', #1132, 5.000000000000004441 ) ;
#23525 = FACE_OUTER_BOUND ( 'NONE', #15726, .T. ) ;
#23526 = EDGE_CURVE ( 'NONE', #16767, #3169, #10453, .T. ) ;
#23527 = CARTESIAN_POINT ( 'NONE',  ( -14.93254240682317047, -8.254432589069386594, 20.24143955528809613 ) ) ;
#23528 = CIRCLE ( 'NONE', #9101, 0.7499999999999997780 ) ;
#23529 = CARTESIAN_POINT ( 'NONE',  ( -23.15749938697695143, 12.07134380388759709, 48.88521798569314569 ) ) ;
#23530 = FACE_BOUND ( 'NONE', #6925, .T. ) ;
#23531 = ORIENTED_EDGE ( 'NONE', *, *, #26915, .T. ) ;
#23532 = VECTOR ( 'NONE', #20932, 1000.000000000000000 ) ;
#23533 = CARTESIAN_POINT ( 'NONE',  ( -16.96078254943347829, 1.685604580053747803, 18.34777357837152323 ) ) ;
#23534 = CARTESIAN_POINT ( 'NONE',  ( 18.33777834721833955, -8.027392848387997049, 5.651989602109219746 ) ) ;
#23535 = CARTESIAN_POINT ( 'NONE',  ( -13.47385700491362215, 10.44730466805193103, 7.643931100913408550 ) ) ;
#23536 = DIRECTION ( 'NONE',  ( -0.000000000000000000, -0.000000000000000000, 1.000000000000000000 ) ) ;
#23537 = VERTEX_POINT ( 'NONE', #13502 ) ;
#23538 = ORIENTED_EDGE ( 'NONE', *, *, #13051, .F. ) ;
#23539 = LINE ( 'NONE', #2183, #24765 ) ;
#23540 = CARTESIAN_POINT ( 'NONE',  ( -19.84404562991029763, 2.492760124447686465, 5.652196082369965069 ) ) ;
#23541 = LINE ( 'NONE', #23689, #26817 ) ;
#23542 = DIRECTION ( 'NONE',  ( 1.000000000000000000, 0.000000000000000000, 0.000000000000000000 ) ) ;
#23543 = CARTESIAN_POINT ( 'NONE',  ( -18.12723876908564691, 34.13071258496300686, 27.50000000000000711 ) ) ;
#23544 = CARTESIAN_POINT ( 'NONE',  ( -19.18576292979354037, 22.55620591602727387, 1.500000000000001332 ) ) ;
#23545 = ORIENTED_EDGE ( 'NONE', *, *, #8977, .T. ) ;
#23546 = CARTESIAN_POINT ( 'NONE',  ( -19.96222469201676475, 1.488090962520939531, 6.560937769032974209 ) ) ;
#23547 = CARTESIAN_POINT ( 'NONE',  ( 14.53509801925589784, 13.73847344395387005, 18.47531940416306284 ) ) ;
#23548 = CARTESIAN_POINT ( 'NONE',  ( 49.99999999999998579, 209.2686044187655909, -75.50000000000001421 ) ) ;
#23549 = ORIENTED_EDGE ( 'NONE', *, *, #17100, .T. ) ;
#23550 = DIRECTION ( 'NONE',  ( 0.000000000000000000, 0.000000000000000000, 1.000000000000000000 ) ) ;
#23551 = AXIS2_PLACEMENT_3D ( 'NONE', #30518, #13850, #5212 ) ;
#23552 = ORIENTED_EDGE ( 'NONE', *, *, #17188, .F. ) ;
#23553 = DIRECTION ( 'NONE',  ( -0.000000000000000000, 0.000000000000000000, 1.000000000000000000 ) ) ;
#23554 = CIRCLE ( 'NONE', #25064, 7.500000000000000000 ) ;
#23555 = CARTESIAN_POINT ( 'NONE',  ( 8.499586724479435418, 2.959227181723830036, 1.500000000000001332 ) ) ;
#23556 = EDGE_LOOP ( 'NONE', ( #7925, #21324, #17596, #28894 ) ) ;
#23557 = CARTESIAN_POINT ( 'NONE',  ( 34.90527075214175312, -9.744570251167933961, 27.50000000000000711 ) ) ;
#23558 = CARTESIAN_POINT ( 'NONE',  ( 0.8038475772933700858, -5.196152422706651564, 9.000000000000001776 ) ) ;
#23559 = DIRECTION ( 'NONE',  ( -0.000000000000000000, -0.000000000000000000, 1.000000000000000000 ) ) ;
#23560 = CYLINDRICAL_SURFACE ( 'NONE', #13795, 21.71568325578193637 ) ;
#23561 = CARTESIAN_POINT ( 'NONE',  ( -6.403603917672689327, 18.96607824920917906, 18.44527579819791185 ) ) ;
#23562 = EDGE_CURVE ( 'NONE', #25305, #24319, #4266, .T. ) ;
#23563 = CARTESIAN_POINT ( 'NONE',  ( 11.64054540341803978, 16.26338533980433709, 24.50000000000000000 ) ) ;
#23564 = DIRECTION ( 'NONE',  ( -0.000000000000000000, 1.132880637372608986E-16, -1.000000000000000000 ) ) ;
#23565 = DIRECTION ( 'NONE',  ( 0.000000000000000000, 0.000000000000000000, -1.000000000000000000 ) ) ;
#23566 = VERTEX_POINT ( 'NONE', #20647 ) ;
#23567 = CARTESIAN_POINT ( 'NONE',  ( 15.81416692036122917, -6.360574302898113430, 5.652196082368483587 ) ) ;
#23568 = AXIS2_PLACEMENT_3D ( 'NONE', #26033, #25585, #11544 ) ;
#23569 = DIRECTION ( 'NONE',  ( 0.000000000000000000, -0.000000000000000000, -1.000000000000000000 ) ) ;
#23570 = CARTESIAN_POINT ( 'NONE',  ( -9.216505592218814158, -7.781333699927420966, -1.500000000000000000 ) ) ;
#23571 = EDGE_LOOP ( 'NONE', ( #7499, #15389, #18577, #22139 ) ) ;
#23572 = LINE ( 'NONE', #2062, #12069 ) ;
#23573 = AXIS2_PLACEMENT_3D ( 'NONE', #29786, #16044, #30395 ) ;
#23574 = CARTESIAN_POINT ( 'NONE',  ( -14.70423443302405708, -8.686234331489295357, 19.47783254395485031 ) ) ;
#23575 = FACE_OUTER_BOUND ( 'NONE', #13789, .T. ) ;
#23576 = VECTOR ( 'NONE', #3742, 1000.000000000000000 ) ;
#23577 = CARTESIAN_POINT ( 'NONE',  ( -34.07766914599911701, 21.40380666528009002, -1.500000000000000000 ) ) ;
#23578 = CARTESIAN_POINT ( 'NONE',  ( 32.74775157611827581, 27.21557300921217859, -19.50000000000000355 ) ) ;
#23579 = ORIENTED_EDGE ( 'NONE', *, *, #4218, .T. ) ;
#23580 = CARTESIAN_POINT ( 'NONE',  ( -4.163336342344337027E-14, 1.387778780781445676E-14, 24.50000000000000000 ) ) ;
#23581 = CARTESIAN_POINT ( 'NONE',  ( -5.105024945673440229, 42.22604126506271172, -1.500000000000000000 ) ) ;
#23582 = CARTESIAN_POINT ( 'NONE',  ( 28.09938986509257930, 29.50836898064226688, 34.53879572982188506 ) ) ;
#23583 = DIRECTION ( 'NONE',  ( 0.000000000000000000, -0.5000000000000015543, 0.8660254037844378194 ) ) ;
#23584 = VERTEX_POINT ( 'NONE', #30167 ) ;
#23585 = DIRECTION ( 'NONE',  ( -0.5503133621338230919, 0.8349582046168344540, 0.000000000000000000 ) ) ;
#23586 = CARTESIAN_POINT ( 'NONE',  ( -19.64114023396061981, 37.13592150528867109, -1.500000000000000000 ) ) ;
#23587 = DIRECTION ( 'NONE',  ( 1.000000000000000000, 0.000000000000000000, 0.000000000000000000 ) ) ;
#23588 = ORIENTED_EDGE ( 'NONE', *, *, #19268, .F. ) ;
#23589 = ORIENTED_EDGE ( 'NONE', *, *, #29903, .T. ) ;
#23590 = CARTESIAN_POINT ( 'NONE',  ( -32.14095006730909176, -14.40137518142634576, 35.53782825234922171 ) ) ;
#23591 = PRODUCT ( 'Rotor', 'Rotor', '', ( #15039 ) ) ;
#23592 = ORIENTED_EDGE ( 'NONE', *, *, #30503, .T. ) ;
#23593 = CARTESIAN_POINT ( 'NONE',  ( -0.6524377400371712543, -20.00727110999511993, 19.22654678686458141 ) ) ;
#23594 = AXIS2_PLACEMENT_3D ( 'NONE', #14929, #21791, #7761 ) ;
#23595 = CARTESIAN_POINT ( 'NONE',  ( -9.736160311572508164, -17.49040459468424658, 7.098451512883313441 ) ) ;
#23596 = CARTESIAN_POINT ( 'NONE',  ( 8.413215745754998309, -3.196529495465417980, 1.500000000000001332 ) ) ;
#23597 = CARTESIAN_POINT ( 'NONE',  ( 0.4236634240584221112, -20.01342612130735787, 20.34789198813115263 ) ) ;
#23598 = ORIENTED_EDGE ( 'NONE', *, *, #11452, .T. ) ;
#23599 = CARTESIAN_POINT ( 'NONE',  ( -1.096289798481170570E-10, -7.028748153765593365, -16.50000000000000000 ) ) ;
#23600 = CARTESIAN_POINT ( 'NONE',  ( -13.00999358272542494, -0.8602714556717691030, 1.500000000000001332 ) ) ;
#23601 = CARTESIAN_POINT ( 'NONE',  ( 14.59199839715918046, 13.70371665158259944, 18.44527579819791185 ) ) ;
#23602 = CARTESIAN_POINT ( 'NONE',  ( 26.36764545593177544, -31.31467416275353344, -1.500000000000000000 ) ) ;
#23603 = VERTEX_POINT ( 'NONE', #13652 ) ;
#23604 = EDGE_CURVE ( 'NONE', #18363, #15822, #15941, .T. ) ;
#23605 = CARTESIAN_POINT ( 'NONE',  ( -15.34307810681595896, 12.82926163924266660, 7.652108011868850035 ) ) ;
#23606 = DIRECTION ( 'NONE',  ( 1.000000000000000000, 0.000000000000000000, 0.000000000000000000 ) ) ;
#23607 = FACE_OUTER_BOUND ( 'NONE', #2014, .T. ) ;
#23608 = DIRECTION ( 'NONE',  ( 1.000000000000000000, 0.000000000000000000, 0.000000000000000000 ) ) ;
#23609 = CARTESIAN_POINT ( 'NONE',  ( 9.163215745754998309, -3.196529495465417980, 1.500000000000001332 ) ) ;
#23610 = CARTESIAN_POINT ( 'NONE',  ( -18.06093776605888479, -8.632162463936117192, 20.34789198813115263 ) ) ;
#23611 = CARTESIAN_POINT ( 'NONE',  ( 32.89824568090541845, -8.841523719485381960, 36.69179515804835034 ) ) ;
#23612 = ORIENTED_EDGE ( 'NONE', *, *, #4209, .T. ) ;
#23613 = EDGE_LOOP ( 'NONE', ( #13144, #27156 ) ) ;
#23614 = CARTESIAN_POINT ( 'NONE',  ( -8.413215745754975217, 3.196529495465474380, -3.621320343559650379 ) ) ;
#23615 = AXIS2_PLACEMENT_3D ( 'NONE', #20567, #8724, #18239 ) ;
#23616 = CARTESIAN_POINT ( 'NONE',  ( -2.552544031601109875, 42.50000000001772094, -1.500000000000000000 ) ) ;
#23617 = CARTESIAN_POINT ( 'NONE',  ( -26.80246859415415273, -7.028748154183645624, -1.499999999999999556 ) ) ;
#23618 = DIRECTION ( 'NONE',  ( 1.000000000000000000, 0.000000000000000000, 0.000000000000000000 ) ) ;
#23619 = ORIENTED_EDGE ( 'NONE', *, *, #28250, .F. ) ;
#23620 = DIRECTION ( 'NONE',  ( 1.000000000000000000, 0.000000000000000000, 0.000000000000000000 ) ) ;
#23621 = CARTESIAN_POINT ( 'NONE',  ( 17.93426220341855171, -8.892634148397208449, 19.11611934778430921 ) ) ;
#23622 = CARTESIAN_POINT ( 'NONE',  ( 5.913643690471324987, 19.12442985200254597, 7.429667576816606278 ) ) ;
#23623 = ORIENTED_EDGE ( 'NONE', *, *, #25043, .F. ) ;
#23624 = CARTESIAN_POINT ( 'NONE',  ( 0.000000000000000000, 0.000000000000000000, 0.000000000000000000 ) ) ;
#23625 = CARTESIAN_POINT ( 'NONE',  ( 14.79741041486972541, 13.48156734445487714, 7.643931100913408550 ) ) ;
#23626 = CARTESIAN_POINT ( 'NONE',  ( -13.28078564537778838, -41.66453699854426418, -16.49999999999999289 ) ) ;
#23627 = CARTESIAN_POINT ( 'NONE',  ( -37.01201912122522231, 13.45809432592687038, 31.66270403581487258 ) ) ;
#23628 = ORIENTED_EDGE ( 'NONE', *, *, #10956, .F. ) ;
#23629 = PLANE ( 'NONE',  #10859 ) ;
#23630 = EDGE_CURVE ( 'NONE', #6239, #26662, #25800, .T. ) ;
#23631 = EDGE_CURVE ( 'NONE', #7923, #26638, #5468, .T. ) ;
#23632 = FACE_OUTER_BOUND ( 'NONE', #25368, .T. ) ;
#23633 = CARTESIAN_POINT ( 'NONE',  ( -4.163336342344337027E-14, -1.387778780781445676E-14, -1.500000000000000000 ) ) ;
#23634 = ORIENTED_EDGE ( 'NONE', *, *, #7446, .F. ) ;
#23635 = CARTESIAN_POINT ( 'NONE',  ( -15.53738272950673682, -6.955830428693971612, 6.211014596808754007 ) ) ;
#23636 = AXIS2_PLACEMENT_3D ( 'NONE', #30166, #27677, #18021 ) ;
#23637 = DIRECTION ( 'NONE',  ( 1.000000000000000000, 0.000000000000000000, 0.000000000000000000 ) ) ;
#23638 = PRESENTATION_STYLE_ASSIGNMENT (( #25545 ) ) ;
#23639 = EDGE_CURVE ( 'NONE', #8694, #24029, #16931, .T. ) ;
#23640 = CARTESIAN_POINT ( 'NONE',  ( 0.000000000000000000, 0.000000000000000000, -52.50000000000000000 ) ) ;
#23641 = LINE ( 'NONE', #1682, #22220 ) ;
#23642 = CARTESIAN_POINT ( 'NONE',  ( 5.524309650260767590, -7.706848733600972778, 13.00000000000000178 ) ) ;
#23643 = CARTESIAN_POINT ( 'NONE',  ( -17.03429152191316831, 1.023117790763816037, 20.13759033520874908 ) ) ;
#23644 = DIRECTION ( 'NONE',  ( 0.1423148382732746797, -0.9898214418809342385, 0.000000000000000000 ) ) ;
#23645 = EDGE_LOOP ( 'NONE', ( #21090, #8542, #28777, #10757 ) ) ;
#23646 = ADVANCED_FACE ( 'NONE', ( #14555 ), #26245, .F. ) ;
#23647 = CARTESIAN_POINT ( 'NONE',  ( 11.39002951368468430, -16.46174851469274003, 20.29915277494337644 ) ) ;
#23648 = CARTESIAN_POINT ( 'NONE',  ( 11.52197458429827037, 37.50933785548059518, 27.50000000000000355 ) ) ;
#23649 = ADVANCED_FACE ( 'NONE', ( #7698 ), #5347, .F. ) ;
#23650 = ORIENTED_EDGE ( 'NONE', *, *, #10988, .F. ) ;
#23651 = EDGE_LOOP ( 'NONE', ( #17475, #7415, #29526, #24633 ) ) ;
#23652 = ADVANCED_FACE ( 'NONE', ( #10033 ), #5121, .F. ) ;
#23653 = DIRECTION ( 'NONE',  ( -0.000000000000000000, 1.000000000000000000, -1.224646799147353207E-16 ) ) ;
#23654 = ORIENTED_EDGE ( 'NONE', *, *, #30356, .F. ) ;
#23655 = B_SPLINE_CURVE_WITH_KNOTS ( 'NONE', 3,
 ( #7590, #28497, #19437, #28954, #21924, #10074, #7127, #11968, #14277, #16639 ),
 .UNSPECIFIED., .F., .F.,
 ( 4, 2, 2, 2, 4 ),
 ( 0.000000000000000000, 0.007809271317857106529, 0.01561854263571419571, 0.03123708527142839142, 0.03978722987217712947 ),
 .UNSPECIFIED. ) ;
#23656 = CARTESIAN_POINT ( 'NONE',  ( 2.270234684139677217, -8.795879380940572645, -1.500000000000002887 ) ) ;
#23657 = CIRCLE ( 'NONE', #12212, 0.7499999999999997780 ) ;
#23658 = DIRECTION ( 'NONE',  ( -1.000000000000000000, 0.000000000000000000, 0.000000000000000000 ) ) ;
#23659 = ORIENTED_EDGE ( 'NONE', *, *, #3451, .F. ) ;
#23660 = CARTESIAN_POINT ( 'NONE',  ( 18.72527277698615222, -7.076062192109020543, 19.58863275299554019 ) ) ;
#23661 = CARTESIAN_POINT ( 'NONE',  ( 16.55532831589957254, 4.193940174973931789, 19.36813350477385143 ) ) ;
#23662 = DIRECTION ( 'NONE',  ( 0.000000000000000000, 0.000000000000000000, 1.000000000000000000 ) ) ;
#23663 = VERTEX_POINT ( 'NONE', #21711 ) ;
#23664 = CARTESIAN_POINT ( 'NONE',  ( 12.37236664230077743, -12.04390635323149716, -0.6213203435596476032 ) ) ;
#23665 = ADVANCED_FACE ( 'NONE', ( #19222 ), #10177, .F. ) ;
#23666 = EDGE_LOOP ( 'NONE', ( #10276, #16463, #16135, #2620, #16243, #23435, #11692 ) ) ;
#23667 = ADVANCED_FACE ( 'NONE', ( #24052 ), #2698, .F. ) ;
#23668 = COLOUR_RGB ( '',0.7921568627450980005, 0.8196078431372548767, 0.9333333333333333481 ) ;
#23669 = EDGE_CURVE ( 'NONE', #7211, #15632, #28379, .T. ) ;
#23670 = ORIENTED_EDGE ( 'NONE', *, *, #28125, .T. ) ;
#23671 = EDGE_CURVE ( 'NONE', #346, #119, #21412, .T. ) ;
#23672 = DIRECTION ( 'NONE',  ( 0.000000000000000000, 0.000000000000000000, 1.000000000000000000 ) ) ;
#23673 = CARTESIAN_POINT ( 'NONE',  ( 52.16608720827707657, 51.86186943028246787, 57.49999999999999289 ) ) ;
#23674 = AXIS2_PLACEMENT_3D ( 'NONE', #16775, #28339, #21295 ) ;
#23675 = CARTESIAN_POINT ( 'NONE',  ( -7.658030750032036593, -41.69611546128646751, 28.90941362898500699 ) ) ;
#23676 = CARTESIAN_POINT ( 'NONE',  ( 20.46975788395958418, -26.57181885929544407, -16.50000600000000262 ) ) ;
#23677 = CARTESIAN_POINT ( 'NONE',  ( 5.204170427930421283E-15, -44.07656352898514740, -16.50000000000000000 ) ) ;
#23678 = ORIENTED_EDGE ( 'NONE', *, *, #29975, .F. ) ;
#23679 = EDGE_CURVE ( 'NONE', #115, #25416, #23907, .T. ) ;
#23680 = CARTESIAN_POINT ( 'NONE',  ( -19.80175191879421703, 2.933369436805208785, 18.44501272782439827 ) ) ;
#23681 = CARTESIAN_POINT ( 'NONE',  ( 10.94975753521667095, -37.63148039617637153, 34.49999999999998579 ) ) ;
#23682 = CARTESIAN_POINT ( 'NONE',  ( -4.163336342344337027E-14, 1.387778780781445676E-14, 24.50000000000000000 ) ) ;
#23683 = FACE_OUTER_BOUND ( 'NONE', #25098, .T. ) ;
#23684 = ORIENTED_EDGE ( 'NONE', *, *, #15271, .T. ) ;
#23685 = VERTEX_POINT ( 'NONE', #196 ) ;
#23686 = FACE_OUTER_BOUND ( 'NONE', #21381, .T. ) ;
#23687 = LINE ( 'NONE', #12015, #20100 ) ;
#23688 = DIRECTION ( 'NONE',  ( 1.000000000000000000, 0.000000000000000000, 0.000000000000000000 ) ) ;
#23689 = CARTESIAN_POINT ( 'NONE',  ( -9.041888939645131629, 0.8750451464063457863, 13.22130136205108819 ) ) ;
#23690 = LINE ( 'NONE', #27946, #18615 ) ;
#23691 = AXIS2_PLACEMENT_3D ( 'NONE', #9120, #28147, #18186 ) ;
#23692 = LINE ( 'NONE', #21511, #4433 ) ;
#23693 = CARTESIAN_POINT ( 'NONE',  ( -19.18576292979354037, 22.55620591602727387, 24.50000000000000000 ) ) ;
#23694 = EDGE_CURVE ( 'NONE', #25239, #28858, #16948, .T. ) ;
#23695 = ORIENTED_EDGE ( 'NONE', *, *, #28242, .T. ) ;
#23696 = ADVANCED_FACE ( 'NONE', ( #351 ), #24370, .F. ) ;
#23697 = CARTESIAN_POINT ( 'NONE',  ( -15.65263381497855200, -35.63608703567959424, 34.50000000000000000 ) ) ;
#23698 = DIRECTION ( 'NONE',  ( -2.312964634635740689E-15, 1.000000000000000000, 0.000000000000000000 ) ) ;
#23699 = FACE_OUTER_BOUND ( 'NONE', #14377, .T. ) ;
#23700 = ORIENTED_EDGE ( 'NONE', *, *, #9947, .T. ) ;
#23701 = AXIS2_PLACEMENT_3D ( 'NONE', #11853, #4822, #23847 ) ;
#23702 = LINE ( 'NONE', #6879, #28238 ) ;
#23703 = ORIENTED_EDGE ( 'NONE', *, *, #16063, .T. ) ;
#23704 = PLANE ( 'NONE',  #23383 ) ;
#23705 = CIRCLE ( 'NONE', #10271, 20.00000000000000355 ) ;
#23706 = CIRCLE ( 'NONE', #10273, 20.00000000000000000 ) ;
#23707 = CARTESIAN_POINT ( 'NONE',  ( 11.10715495309693601, -16.63223102436629830, 20.34789198813115263 ) ) ;
#23708 = ORIENTED_EDGE ( 'NONE', *, *, #2724, .T. ) ;
#23709 = CARTESIAN_POINT ( 'NONE',  ( 24.34596477403963277, 29.10061797482480017, 27.50000000000001066 ) ) ;
#23710 = APPLICATION_CONTEXT ( 'automotive_design' ) ;
#23711 = CARTESIAN_POINT ( 'NONE',  ( -7.730328572437709767, 4.608906612435681005, 21.50000000000000000 ) ) ;
#23712 = CARTESIAN_POINT ( 'NONE',  ( 10.65056555576078701, -13.34799940468896473, 19.02573955821369367 ) ) ;
#23713 = B_SPLINE_CURVE_WITH_KNOTS ( 'NONE', 3,
 ( #8976, #30034, #1650, #8819, #13666, #21106, #9271, #18344, #11317, #23149, #1797, #27855, #22852, #23309, #30625, #6939 ),
 .UNSPECIFIED., .F., .F.,
 ( 4, 2, 2, 2, 2, 2, 2, 4 ),
 ( 0.4999999999999997780, 0.6249999999999998890, 0.6875000000000000000, 0.7187500000000000000, 0.7499999999999998890, 0.8124999999999997780, 0.8749999999999997780, 1.000000000000000000 ),
 .UNSPECIFIED. ) ;
#23714 = CARTESIAN_POINT ( 'NONE',  ( 0.07568653364412844531, -1.751902528157471828, -9.000000000000000000 ) ) ;
#23715 = AXIS2_PLACEMENT_3D ( 'NONE', #713, #260, #19289 ) ;
#23716 = AXIS2_PLACEMENT_3D ( 'NONE', #15648, #13168, #3507 ) ;
#23717 = DIRECTION ( 'NONE',  ( 1.000000000000000000, 0.000000000000000000, 0.000000000000000000 ) ) ;
#23718 = LINE ( 'NONE', #4401, #18797 ) ;
#23719 = CARTESIAN_POINT ( 'NONE',  ( 11.10715495309693424, -16.63223102436629475, 20.34789198813115263 ) ) ;
#23720 = ORIENTED_EDGE ( 'NONE', *, *, #990, .T. ) ;
#23721 = CARTESIAN_POINT ( 'NONE',  ( 15.57266529552203416, 38.96488032230103471, 1.500000000000000000 ) ) ;
#23722 = AXIS2_PLACEMENT_3D ( 'NONE', #5670, #5361, #22192 ) ;
#23723 = CARTESIAN_POINT ( 'NONE',  ( 0.000000000000000000, 44.39187623478217404, -19.50000000000000355 ) ) ;
#23724 = CARTESIAN_POINT ( 'NONE',  ( -33.42925964089141644, 11.06161099612212695, -16.55003854064094426 ) ) ;
#23725 = VERTEX_POINT ( 'NONE', #7388 ) ;
#23726 = DIRECTION ( 'NONE',  ( -0.000000000000000000, -0.000000000000000000, -1.000000000000000000 ) ) ;
#23727 = VECTOR ( 'NONE', #21383, 1000.000000000000000 ) ;
#23728 = CYLINDRICAL_SURFACE ( 'NONE', #17795, 7.500000000000000000 ) ;
#23729 = LINE ( 'NONE', #9862, #30181 ) ;
#23730 = CARTESIAN_POINT ( 'NONE',  ( -4.163336342344337027E-14, 1.387778780781445676E-14, 1.500000000000000000 ) ) ;
#23731 = AXIS2_PLACEMENT_3D ( 'NONE', #26116, #5220, #78 ) ;
#23732 = FACE_OUTER_BOUND ( 'NONE', #23571, .T. ) ;
#23733 = VERTEX_POINT ( 'NONE', #7070 ) ;
#23734 = CARTESIAN_POINT ( 'NONE',  ( -12.56641067637752229, 40.32935944495016400, -1.500000000000000000 ) ) ;
#23735 = CARTESIAN_POINT ( 'NONE',  ( 37.46474186269768580, -2.090463118055147618, 37.49999999995337419 ) ) ;
#23736 = CARTESIAN_POINT ( 'NONE',  ( 69.99999999999998579, 70.00000000000000000, 12.49999999999999112 ) ) ;
#23737 = ORIENTED_EDGE ( 'NONE', *, *, #3486, .T. ) ;
#23738 = DIRECTION ( 'NONE',  ( 1.000000000000000000, 0.000000000000000000, 0.000000000000000000 ) ) ;
#23739 = ORIENTED_EDGE ( 'NONE', *, *, #14349, .T. ) ;
#23740 = AXIS2_PLACEMENT_3D ( 'NONE', #15336, #1004, #683 ) ;
#23741 = CARTESIAN_POINT ( 'NONE',  ( 5.105024945673418912, -42.22604126506271882, -1.500000000000000000 ) ) ;
#23742 = DIRECTION ( 'NONE',  ( 0.000000000000000000, 0.000000000000000000, 1.000000000000000000 ) ) ;
#23743 = ORIENTED_EDGE ( 'NONE', *, *, #25370, .F. ) ;
#23744 = ORIENTED_EDGE ( 'NONE', *, *, #4928, .T. ) ;
#23745 = CARTESIAN_POINT ( 'NONE',  ( 46.99999999999998579, 87.00000000000001421, 0.000000000000000000 ) ) ;
#23746 = AXIS2_PLACEMENT_3D ( 'NONE', #2268, #242, #6964 ) ;
#23747 = EDGE_LOOP ( 'NONE', ( #17517, #23773, #16893, #25574 ) ) ;
#23748 = ORIENTED_EDGE ( 'NONE', *, *, #30735, .F. ) ;
#23749 = CARTESIAN_POINT ( 'NONE',  ( 0.4421796641654207050, -17.03052986487778497, 20.29090034784956131 ) ) ;
#23750 = AXIS2_PLACEMENT_3D ( 'NONE', #9582, #4445, #23450 ) ;
#23751 = CARTESIAN_POINT ( 'NONE',  ( -7.995704773938818732, -15.07639970738306801, 5.872146474157316831 ) ) ;
#23752 = AXIS2_PLACEMENT_3D ( 'NONE', #24940, #20260, #10915 ) ;
#23753 = DIRECTION ( 'NONE',  ( 0.000000000000000000, 1.132880637372608986E-16, -1.000000000000000000 ) ) ;
#23754 = VERTEX_POINT ( 'NONE', #12210 ) ;
#23755 = CARTESIAN_POINT ( 'NONE',  ( 18.53278507915170437, -7.520016387818809100, 7.528076282304597022 ) ) ;
#23756 = CARTESIAN_POINT ( 'NONE',  ( 0.000000000000000000, 0.000000000000000000, 0.000000000000000000 ) ) ;
#23757 = CARTESIAN_POINT ( 'NONE',  ( 12.05308393316171234, 12.07205540120322595, 18.44527579819791185 ) ) ;
#23758 = PLANE ( 'NONE',  #25577 ) ;
#23759 = AXIS2_PLACEMENT_3D ( 'NONE', #20683, #11037, #6043 ) ;
#23760 = VERTEX_POINT ( 'NONE', #511 ) ;
#23761 = AXIS2_PLACEMENT_3D ( 'NONE', #10946, #27931, #1580 ) ;
#23762 = CIRCLE ( 'NONE', #11823, 7.500000000000000000 ) ;
#23763 = CARTESIAN_POINT ( 'NONE',  ( 39.99999999999998579, 90.00000000000001421, 22.49999999999999289 ) ) ;
#23764 = CARTESIAN_POINT ( 'NONE',  ( -18.05883735157481951, -8.636530476581215865, 5.652196082364323360 ) ) ;
#23765 = CARTESIAN_POINT ( 'NONE',  ( -13.20835299076127711, 10.76336294900085733, 20.32222155561919053 ) ) ;
#23766 = CARTESIAN_POINT ( 'NONE',  ( -19.84404562991029763, 2.492760124447686465, 5.652196082369965069 ) ) ;
#23767 = CARTESIAN_POINT ( 'NONE',  ( 42.49999999999998579, -50.00000000000000000, 12.49999999999999112 ) ) ;
#23768 = VECTOR ( 'NONE', #12509, 1000.000000000000114 ) ;
#23769 = CARTESIAN_POINT ( 'NONE',  ( -15.16307466657772807, -7.786257835515859149, 18.34798005862930381 ) ) ;
#23770 = CARTESIAN_POINT ( 'NONE',  ( -26.80246859415415273, -7.028748154183637631, -1.499999999999999556 ) ) ;
#23771 = CIRCLE ( 'NONE', #2364, 0.7499999999999997780 ) ;
#23772 = ORIENTED_EDGE ( 'NONE', *, *, #18240, .F. ) ;
#23773 = ORIENTED_EDGE ( 'NONE', *, *, #7295, .F. ) ;
#23774 = VECTOR ( 'NONE', #16784, 1000.000000000000000 ) ;
#23775 = DIRECTION ( 'NONE',  ( -0.000000000000000000, -0.000000000000000000, -1.000000000000000000 ) ) ;
#23776 = CARTESIAN_POINT ( 'NONE',  ( -34.07766914599908148, -21.40380666528021081, -1.500000000000000000 ) ) ;
#23777 = DIRECTION ( 'NONE',  ( 0.000000000000000000, -1.132880637372608986E-16, 1.000000000000000000 ) ) ;
#23778 = CARTESIAN_POINT ( 'NONE',  ( 0.000000000000000000, 0.000000000000000000, 1.500000000000001332 ) ) ;
#23779 = VERTEX_POINT ( 'NONE', #26569 ) ;
#23780 = CARTESIAN_POINT ( 'NONE',  ( 0.000000000000000000, 0.000000000000000000, 0.000000000000000000 ) ) ;
#23781 = VECTOR ( 'NONE', #1500, 1000.000000000000000 ) ;
#23782 = CARTESIAN_POINT ( 'NONE',  ( 18.25868057198135830, -8.206406842115287148, 20.32842677360128292 ) ) ;
#23783 = EDGE_CURVE ( 'NONE', #8903, #27691, #2855, .T. ) ;
#23784 = CARTESIAN_POINT ( 'NONE',  ( 6.247918173525850882, 19.01788707503811438, 6.864725433338323413 ) ) ;
#23785 = CIRCLE ( 'NONE', #10357, 3.000000000000002665 ) ;
#23786 = EDGE_LOOP ( 'NONE', ( #6540, #12945, #7174, #13686 ) ) ;
#23787 = CARTESIAN_POINT ( 'NONE',  ( 6.124711512895119725, 19.05797279266333888, 18.80699882434806369 ) ) ;
#23788 = AXIS2_PLACEMENT_3D ( 'NONE', #18384, #16487, #23181 ) ;
#23789 = CARTESIAN_POINT ( 'NONE',  ( 11.77016209912416578, 12.36695356451125782, 7.196036389296800451 ) ) ;
#23790 = AXIS2_PLACEMENT_3D ( 'NONE', #8826, #1042, #1507 ) ;
#23791 = CARTESIAN_POINT ( 'NONE',  ( 0.000000000000000000, 0.000000000000000000, -1.500000000000001332 ) ) ;
#23792 = CARTESIAN_POINT ( 'NONE',  ( -29.09978263823398237, 28.32965845976518082, 30.22324450238831872 ) ) ;
#23793 = EDGE_LOOP ( 'NONE', ( #13311, #11486, #11799, #28258 ) ) ;
#23794 = CARTESIAN_POINT ( 'NONE',  ( -27.86235613436986114, -14.72519157938688750, 43.48653168448685591 ) ) ;
#23795 = DIRECTION ( 'NONE',  ( 0.000000000000000000, 1.000000000000000000, 0.000000000000000000 ) ) ;
#23796 = CARTESIAN_POINT ( 'NONE',  ( 4.147066042697082011, 43.86011627092103993, -16.49999999999999645 ) ) ;
#23797 = AXIS2_PLACEMENT_3D ( 'NONE', #27109, #17914, #24755 ) ;
#23798 = ORIENTED_EDGE ( 'NONE', *, *, #2515, .T. ) ;
#23799 = CARTESIAN_POINT ( 'NONE',  ( -18.47348503376728601, -7.710222065540590641, 6.755862304746362845 ) ) ;
#23800 = DIRECTION ( 'NONE',  ( 0.000000000000000000, 0.000000000000000000, 1.000000000000000000 ) ) ;
#23801 = DIRECTION ( 'NONE',  ( 1.000000000000000000, 0.000000000000000000, 0.000000000000000000 ) ) ;
#23802 = CARTESIAN_POINT ( 'NONE',  ( -13.00999358272542494, -0.8602714556717691030, 1.500000000000001332 ) ) ;
#23803 = CYLINDRICAL_SURFACE ( 'NONE', #14753, 0.7499999999999997780 ) ;
#23804 = CARTESIAN_POINT ( 'NONE',  ( 10.50506478158603407, 13.32952022457704544, 24.50000000000000000 ) ) ;
#23805 = CARTESIAN_POINT ( 'NONE',  ( 35.04158764634705392, -18.66738852729897502, 17.56791008632125184 ) ) ;
#23806 = CARTESIAN_POINT ( 'NONE',  ( -8.268028093133393597, -3.763133143576407047, -1.500000000000002220 ) ) ;
#23807 = ORIENTED_EDGE ( 'NONE', *, *, #21361, .F. ) ;
#23808 = VECTOR ( 'NONE', #23817, 1000.000000000000000 ) ;
#23809 = CIRCLE ( 'NONE', #24328, 20.00000000000000000 ) ;
#23810 = DIRECTION ( 'NONE',  ( -0.000000000000000000, -1.000000000000000000, -0.000000000000000000 ) ) ;
#23811 = DIRECTION ( 'NONE',  ( -0.000000000000000000, -0.000000000000000000, 1.000000000000000000 ) ) ;
#23812 = AXIS2_PLACEMENT_3D ( 'NONE', #2211, #9692, #25774 ) ;
#23813 = ORIENTED_EDGE ( 'NONE', *, *, #6403, .F. ) ;
#23814 = ORIENTED_EDGE ( 'NONE', *, *, #5239, .F. ) ;
#23815 = CARTESIAN_POINT ( 'NONE',  ( -15.89566665641788745, 12.13797781250046270, 7.161525567826887873 ) ) ;
#23816 = CARTESIAN_POINT ( 'NONE',  ( -13.45329425514681532, 48.15668267613188647, -48.34811677753233283 ) ) ;
#23817 = DIRECTION ( 'NONE',  ( 0.9898214418809327952, -0.1423148382732850048, 0.000000000000000000 ) ) ;
#23818 = EDGE_LOOP ( 'NONE', ( #14480, #3225 ) ) ;
#23819 = AXIS2_PLACEMENT_3D ( 'NONE', #24680, #29063, #15012 ) ;
#23820 = EDGE_CURVE ( 'NONE', #4151, #2298, #16579, .T. ) ;
#23821 = CARTESIAN_POINT ( 'NONE',  ( 6.974883619896790954, 5.687793815610376669, -1.500000000000000888 ) ) ;
#23822 = DIRECTION ( 'NONE',  ( 0.000000000000000000, 0.000000000000000000, 1.000000000000000000 ) ) ;
#23823 = ORIENTED_EDGE ( 'NONE', *, *, #27648, .T. ) ;
#23824 = EDGE_CURVE ( 'NONE', #7501, #12057, #25422, .T. ) ;
#23825 = CARTESIAN_POINT ( 'NONE',  ( 18.59976559251667183, -7.400385892474094618, 18.56793045041961321 ) ) ;
#23826 = CARTESIAN_POINT ( 'NONE',  ( 16.58777033243660526, 4.040313317649107283, 19.89182036555910571 ) ) ;
#23827 = CARTESIAN_POINT ( 'NONE',  ( -33.16313691975489064, 0.000000000000000000, -1.500000000000000000 ) ) ;
#23828 = VERTEX_POINT ( 'NONE', #15006 ) ;
#23829 = CARTESIAN_POINT ( 'NONE',  ( -32.81350286003733885, -7.028748154183637631, -6.500000000000000888 ) ) ;
#23830 = EDGE_LOOP ( 'NONE', ( #28453, #29641, #26045, #19226 ) ) ;
#23831 = PRODUCT_DEFINITION_FORMATION_WITH_SPECIFIED_SOURCE ( 'ANY', '', #26888, .NOT_KNOWN. ) ;
#23832 = VECTOR ( 'NONE', #7668, 1000.000000000000000 ) ;
#23833 = EDGE_CURVE ( 'NONE', #8898, #22640, #15470, .T. ) ;
#23834 = VECTOR ( 'NONE', #16494, 1000.000000000000000 ) ;
#23835 = AXIS2_PLACEMENT_3D ( 'NONE', #30050, #15387, #17727 ) ;
#23836 = VERTEX_POINT ( 'NONE', #10491 ) ;
#23837 = EDGE_CURVE ( 'NONE', #30377, #3296, #19495, .T. ) ;
#23838 = CARTESIAN_POINT ( 'NONE',  ( 24.03057240117690441, -26.57182937991349903, -1.500000000000001332 ) ) ;
#23839 = CARTESIAN_POINT ( 'NONE',  ( -0.02788623088963465904, -17.02558298240835555, 19.96344307082652492 ) ) ;
#23840 = CIRCLE ( 'NONE', #17380, 15.00000000000000000 ) ;
#23841 = CARTESIAN_POINT ( 'NONE',  ( 1.219801289189188287, -17.01504883035041260, 7.559636331181775581 ) ) ;
#23842 = CARTESIAN_POINT ( 'NONE',  ( -14.70309389971831848, -8.688337726274234285, 19.47952243369110903 ) ) ;
#23843 = CARTESIAN_POINT ( 'NONE',  ( -3.993622308618940853, -8.159193615868383986, -1.500000000000002665 ) ) ;
#23844 = FACE_OUTER_BOUND ( 'NONE', #16513, .T. ) ;
#23845 = ORIENTED_EDGE ( 'NONE', *, *, #27715, .T. ) ;
#23846 = LINE ( 'NONE', #7170, #1294 ) ;
#23847 = DIRECTION ( 'NONE',  ( -1.000000000000000000, 0.000000000000000000, 0.000000000000000000 ) ) ;
#23848 = CARTESIAN_POINT ( 'NONE',  ( -4.163336342344337027E-14, 1.387778780781445676E-14, 1.500000000000000000 ) ) ;
#23849 = ORIENTED_EDGE ( 'NONE', *, *, #6510, .F. ) ;
#23850 = ORIENTED_EDGE ( 'NONE', *, *, #26503, .T. ) ;
#23851 = DIRECTION ( 'NONE',  ( 0.000000000000000000, 0.000000000000000000, 1.000000000000000000 ) ) ;
#23852 = EDGE_CURVE ( 'NONE', #10722, #7638, #17447, .T. ) ;
#23853 = CARTESIAN_POINT ( 'NONE',  ( 25.10662277403243436, -23.12558862862892184, -16.50001200000000168 ) ) ;
#23854 = ADVANCED_FACE ( 'NONE', ( #10337 ), #10802, .F. ) ;
#23855 = CARTESIAN_POINT ( 'NONE',  ( 1.000000000000008438, 13.00000000000001421, 24.50000000000000000 ) ) ;
#23856 = PRODUCT ( 'hex bolt gradeab_iso_ISO 4014 - M12 x 120 x 30-N', 'hex bolt gradeab_iso_ISO 4014 - M12 x 120 x 30-N', '', ( #19722 ) ) ;
#23857 = CARTESIAN_POINT ( 'NONE',  ( 18.33793066653144876, -7.982499537706464920, 18.34798005863226678 ) ) ;
#23858 = CARTESIAN_POINT ( 'NONE',  ( 0.000000000000000000, 0.000000000000000000, 21.50000000000000000 ) ) ;
#23859 = AXIS2_PLACEMENT_3D ( 'NONE', #6949, #9280, #6783 ) ;
#23860 = EDGE_CURVE ( 'NONE', #18904, #28337, #7994, .T. ) ;
#23861 = CARTESIAN_POINT ( 'NONE',  ( -35.78592255317990123, -4.958958154555994646, 27.50000000000000355 ) ) ;
#23862 = CARTESIAN_POINT ( 'NONE',  ( -3.395021109945014270, 30.50000000000000355, 1.500000000000001332 ) ) ;
#23863 = VERTEX_POINT ( 'NONE', #8161 ) ;
#23864 = ADVANCED_FACE ( 'NONE', ( #3783 ), #17663, .F. ) ;
#23865 = CARTESIAN_POINT ( 'NONE',  ( -1.025177369996997268, -39.49999999999999289, 34.49999999999998579 ) ) ;
#23866 = AXIS2_PLACEMENT_3D ( 'NONE', #20425, #18411, #15907 ) ;
#23867 = CARTESIAN_POINT ( 'NONE',  ( -17.98413878735053828, -8.751483025296222351, 18.34869673959212122 ) ) ;
#23868 = CARTESIAN_POINT ( 'NONE',  ( 19.76377475971901632, 3.067715173639368853, 18.34726407865098707 ) ) ;
#23869 = EDGE_CURVE ( 'NONE', #20390, #21023, #20921, .T. ) ;
#23870 = ORIENTED_EDGE ( 'NONE', *, *, #28636, .T. ) ;
#23871 = CARTESIAN_POINT ( 'NONE',  ( 14.89738168138696217, 13.37085340703111491, 7.652108011868850035 ) ) ;
#23872 = VERTEX_POINT ( 'NONE', #1456 ) ;
#23873 = EDGE_CURVE ( 'NONE', #4071, #13443, #20154, .T. ) ;
#23874 = DIRECTION ( 'NONE',  ( -0.000000000000000000, -0.000000000000000000, 1.000000000000000000 ) ) ;
#23875 = VECTOR ( 'NONE', #23102, 1000.000000000000000 ) ;
#23876 = LINE ( 'NONE', #21524, #22480 ) ;
#23877 = ORIENTED_EDGE ( 'NONE', *, *, #4387, .T. ) ;
#23878 = CARTESIAN_POINT ( 'NONE',  ( 27.62938074698936219, -25.35013884327572242, 27.49999999999999645 ) ) ;
#23879 = CARTESIAN_POINT ( 'NONE',  ( -39.87350638640939593, 4.706224724266459880, -11.49999999999999645 ) ) ;
#23880 = CARTESIAN_POINT ( 'NONE',  ( 10.29553672485768523, -13.60582241711869322, 20.24143955528809613 ) ) ;
#23881 = CYLINDRICAL_SURFACE ( 'NONE', #20743, 3.000000000000002665 ) ;
#23882 = CARTESIAN_POINT ( 'NONE',  ( -7.500000000000000000, 0.000000000000000000, -16.50000000000000000 ) ) ;
#23883 = CARTESIAN_POINT ( 'NONE',  ( -31.10500197267670330, 15.38309308716404900, 40.29910134388162390 ) ) ;
#23884 = VERTEX_POINT ( 'NONE', #24842 ) ;
#23885 = ADVANCED_FACE ( 'NONE', ( #3479 ), #24987, .F. ) ;
#23886 = CARTESIAN_POINT ( 'NONE',  ( 15.47543066133721901, -7.098048983968496373, 7.267659094423558841 ) ) ;
#23887 = VECTOR ( 'NONE', #11151, 1000.000000000000000 ) ;
#23888 = CARTESIAN_POINT ( 'NONE',  ( 5.105024945673418912, -42.22604126506271882, -1.500000000000000000 ) ) ;
#23889 = PLANE ( 'NONE',  #30739 ) ;
#23890 = VERTEX_POINT ( 'NONE', #7844 ) ;
#23891 = FACE_OUTER_BOUND ( 'NONE', #28829, .T. ) ;
#23892 = DIRECTION ( 'NONE',  ( 3.642919299551291743E-14, 1.000000000000000000, 0.000000000000000000 ) ) ;
#23893 = ADVANCED_FACE ( 'NONE', ( #5660 ), #15157, .T. ) ;
#23894 = LINE ( 'NONE', #11737, #24172 ) ;
#23895 = ADVANCED_FACE ( 'NONE', ( #20318 ), #19849, .F. ) ;
#23896 = DIRECTION ( 'NONE',  ( 0.6707505147970024284, -0.7416830501633134842, 0.000000000000000000 ) ) ;
#23897 = PRESENTATION_LAYER_ASSIGNMENT (  '', '', ( #6476 ) ) ;
#23898 = CARTESIAN_POINT ( 'NONE',  ( 40.89187623478217404, -5.790488632116400858, -19.50000000000000355 ) ) ;
#23899 = VERTEX_POINT ( 'NONE', #6582 ) ;
#23900 =( NAMED_UNIT ( * ) SI_UNIT ( $, .STERADIAN. ) SOLID_ANGLE_UNIT ( ) );
#23901 = CARTESIAN_POINT ( 'NONE',  ( 37.45995770769625466, 1.852643206688098232, 37.49999999997684341 ) ) ;
#23902 = FACE_OUTER_BOUND ( 'NONE', #3484, .T. ) ;
#23903 = ORIENTED_EDGE ( 'NONE', *, *, #28194, .F. ) ;
#23904 = CARTESIAN_POINT ( 'NONE',  ( 1.000000000000008438, 16.48749217771910125, 1.500000000000000000 ) ) ;
#23905 = VERTEX_POINT ( 'NONE', #25463 ) ;
#23906 = CARTESIAN_POINT ( 'NONE',  ( -8.860628911697515875, 8.184276679720483116, -1.500000000000000000 ) ) ;
#23907 = LINE ( 'NONE', #14696, #13461 ) ;
#23908 = ORIENTED_EDGE ( 'NONE', *, *, #4791, .T. ) ;
#23909 = VERTEX_POINT ( 'NONE', #2041 ) ;
#23910 = DIRECTION ( 'NONE',  ( 1.000000000000000000, 0.000000000000000000, 0.000000000000000000 ) ) ;
#23911 = VERTEX_POINT ( 'NONE', #18450 ) ;
#23912 = AXIS2_PLACEMENT_3D ( 'NONE', #22802, #22638, #27184 ) ;
#23913 = ORIENTED_EDGE ( 'NONE', *, *, #11084, .T. ) ;
#23914 = ORIENTED_EDGE ( 'NONE', *, *, #15246, .F. ) ;
#23915 = FACE_OUTER_BOUND ( 'NONE', #22363, .T. ) ;
#23916 = LINE ( 'NONE', #2562, #21457 ) ;
#23917 = CARTESIAN_POINT ( 'NONE',  ( 4.303751186633993697, 16.48600304573620789, 20.32222155561919053 ) ) ;
#23918 = CARTESIAN_POINT ( 'NONE',  ( 0.5710336623368660325, -20.00960304012541258, 20.32367522806703874 ) ) ;
#23919 = ORIENTED_EDGE ( 'NONE', *, *, #25723, .T. ) ;
#23920 = CARTESIAN_POINT ( 'NONE',  ( 18.44003002641400712, -7.744679585886125928, 7.626218077512941562 ) ) ;
#23921 = DIRECTION ( 'NONE',  ( -0.000000000000000000, -0.000000000000000000, 1.000000000000000000 ) ) ;
#23922 = CARTESIAN_POINT ( 'NONE',  ( 11.86828576611215347, 12.26598719735377152, 20.06253562465620632 ) ) ;
#23923 = CYLINDRICAL_SURFACE ( 'NONE', #17107, 7.500000000000013323 ) ;
#23924 = EDGE_LOOP ( 'NONE', ( #20415, #12299, #4293, #3892 ) ) ;
#23925 = ADVANCED_FACE ( 'NONE', ( #22951 ), #15948, .F. ) ;
#23926 = EDGE_CURVE ( 'NONE', #20218, #20928, #1309, .T. ) ;
#23927 = DIRECTION ( 'NONE',  ( 0.000000000000000000, -0.000000000000000000, -1.000000000000000000 ) ) ;
#23928 = DIRECTION ( 'NONE',  ( -0.000000000000000000, -0.000000000000000000, 1.000000000000000000 ) ) ;
#23929 = CARTESIAN_POINT ( 'NONE',  ( -6.914714884271990769, 18.78545221144173638, 6.892848776733236704 ) ) ;
#23930 = DIRECTION ( 'NONE',  ( -1.000000000000000000, 0.000000000000000000, 0.000000000000000000 ) ) ;
#23931 = DIRECTION ( 'NONE',  ( 1.000000000000000000, 0.000000000000000000, 0.000000000000000000 ) ) ;
#23932 = CARTESIAN_POINT ( 'NONE',  ( -24.03057240117690441, -26.57182937991348481, 24.50000000000000000 ) ) ;
#23933 = AXIS2_PLACEMENT_3D ( 'NONE', #128, #26173, #14312 ) ;
#23934 = CARTESIAN_POINT ( 'NONE',  ( 3.912171961291952993, 8.637616862297855747, 13.00000000000000178 ) ) ;
#23935 = ORIENTED_EDGE ( 'NONE', *, *, #29002, .T. ) ;
#23936 = EDGE_LOOP ( 'NONE', ( #14340, #22700, #12891, #26909 ) ) ;
#23937 = LINE ( 'NONE', #15033, #15945 ) ;
#23938 = DIRECTION ( 'NONE',  ( 0.000000000000000000, 0.000000000000000000, -1.000000000000000000 ) ) ;
#23939 = CARTESIAN_POINT ( 'NONE',  ( -7.856594496258223259, -4.390207617113929039, -3.621320343559650379 ) ) ;
#23940 = CARTESIAN_POINT ( 'NONE',  ( 11.77028954461707144, -16.17000817291664205, 19.96797677718664588 ) ) ;
#23941 = EDGE_LOOP ( 'NONE', ( #11234, #6116, #22211, #4061 ) ) ;
#23942 = DIRECTION ( 'NONE',  ( -0.000000000000000000, 1.132880637372608986E-16, -1.000000000000000000 ) ) ;
#23943 = CARTESIAN_POINT ( 'NONE',  ( 4.744089322959556654, 16.35312844164165114, 7.359006845440219102 ) ) ;
#23944 = ORIENTED_EDGE ( 'NONE', *, *, #14699, .T. ) ;
#23945 = CARTESIAN_POINT ( 'NONE',  ( 4.996079307276525938, 16.27198743970616235, 19.11611934778430921 ) ) ;
#23946 = CARTESIAN_POINT ( 'NONE',  ( 14.67322144252663740, 13.61684651386558187, 7.603368798681074736 ) ) ;
#23947 = CARTESIAN_POINT ( 'NONE',  ( -18.02176112063609636, -39.50256893433222416, -16.50000000000000000 ) ) ;
#23948 = CARTESIAN_POINT ( 'NONE',  ( -18.10334121439571931, 37.65254011239409948, 34.52361733454125670 ) ) ;
#23949 = ORIENTED_EDGE ( 'NONE', *, *, #18931, .F. ) ;
#23950 = CARTESIAN_POINT ( 'NONE',  ( -26.11179934312166040, -14.04991663536888780, 45.34931131770226642 ) ) ;
#23951 = CIRCLE ( 'NONE', #14490, 0.7500000000000006661 ) ;
#23952 = CARTESIAN_POINT ( 'NONE',  ( 32.90011853910910844, 8.843064278303863546, 36.68958760228017013 ) ) ;
#23953 = AXIS2_PLACEMENT_3D ( 'NONE', #24899, #6023, #15843 ) ;
#23954 = CARTESIAN_POINT ( 'NONE',  ( 17.08170687911586327, 39.99681618153512375, -16.50000000000000711 ) ) ;
#23955 = EDGE_LOOP ( 'NONE', ( #1588, #8124, #13224, #16498 ) ) ;
#23956 = DIRECTION ( 'NONE',  ( -0.000000000000000000, -0.000000000000000000, -1.000000000000000000 ) ) ;
#23957 = CARTESIAN_POINT ( 'NONE',  ( 14.20168120032941950, 14.08243226175161844, 6.392525840300335105 ) ) ;
#23958 = CARTESIAN_POINT ( 'NONE',  ( 0.01636335959932776890, -20.01808238691632624, 5.701226463332907279 ) ) ;
#23959 = LINE ( 'NONE', #2919, #28203 ) ;
#23960 = CARTESIAN_POINT ( 'NONE',  ( -32.98805937973593672, 22.67054169308932643, 18.00000000000000000 ) ) ;
#23961 = CARTESIAN_POINT ( 'NONE',  ( 36.40552445234710888, -15.25516137876289591, 9.339579183450858579 ) ) ;
#23962 = CARTESIAN_POINT ( 'NONE',  ( 6.899999999999999467, 9.000000000000000000, 0.000000000000000000 ) ) ;
#23963 = ORIENTED_EDGE ( 'NONE', *, *, #30716, .F. ) ;
#23964 = CYLINDRICAL_SURFACE ( 'NONE', #14764, 1.999999999999998224 ) ;
#23965 = CARTESIAN_POINT ( 'NONE',  ( 22.58267429318971864, 26.57182937991349903, -6.499999999999999112 ) ) ;
#23966 = EDGE_LOOP ( 'NONE', ( #9879, #10417 ) ) ;
#23967 = ORIENTED_EDGE ( 'NONE', *, *, #8911, .T. ) ;
#23968 = CARTESIAN_POINT ( 'NONE',  ( -48.17766558237416064, 69.91760311152096108, 58.26458773037651895 ) ) ;
#23969 = DIRECTION ( 'NONE',  ( 0.000000000000000000, -1.000000000000000000, 0.000000000000000000 ) ) ;
#23970 =( NAMED_UNIT ( * ) PLANE_ANGLE_UNIT ( ) SI_UNIT ( $, .RADIAN. ) );
#23971 = ORIENTED_EDGE ( 'NONE', *, *, #11146, .T. ) ;
#23972 = CIRCLE ( 'NONE', #8573, 15.00000000000003553 ) ;
#23973 = CARTESIAN_POINT ( 'NONE',  ( 31.29501345865701012, -26.27841684422097401, -6.499999999999999112 ) ) ;
#23974 = VERTEX_POINT ( 'NONE', #29987 ) ;
#23975 = CARTESIAN_POINT ( 'NONE',  ( 16.19545619402287073, -5.420160174983553958, 19.25672174529527325 ) ) ;
#23976 = CARTESIAN_POINT ( 'NONE',  ( 19.70397673731432064, 3.532048315275336581, 18.39992786714538298 ) ) ;
#23977 = CARTESIAN_POINT ( 'NONE',  ( -4.163336342344337027E-14, 1.387778780781445676E-14, 51.25735931288069480 ) ) ;
#23978 = ORIENTED_EDGE ( 'NONE', *, *, #10925, .T. ) ;
#23979 = CARTESIAN_POINT ( 'NONE',  ( 15.44249669567090777, -7.165351778216223266, 19.85270094495842130 ) ) ;
#23980 = ORIENTED_EDGE ( 'NONE', *, *, #21972, .T. ) ;
#23981 = VECTOR ( 'NONE', #13881, 1000.000000000000000 ) ;
#23982 = ORIENTED_EDGE ( 'NONE', *, *, #11266, .F. ) ;
#23983 = CARTESIAN_POINT ( 'NONE',  ( 21.62412008219442683, 35.47471372268120859, 29.49052918880962437 ) ) ;
#23984 = CARTESIAN_POINT ( 'NONE',  ( -17.92868989761418774, -8.864358285757575118, 7.626218077512941562 ) ) ;
#23985 = VECTOR ( 'NONE', #10389, 1000.000000000000000 ) ;
#23986 = CARTESIAN_POINT ( 'NONE',  ( -8.163758309741956154, -14.97879848885351173, 18.44527579819791185 ) ) ;
#23987 = CARTESIAN_POINT ( 'NONE',  ( -14.72786953156221301, -8.642539778700260911, 19.02573955821368656 ) ) ;
#23988 = DIRECTION ( 'NONE',  ( 1.000000000000000000, 0.000000000000000000, 0.000000000000000000 ) ) ;
#23989 = DIRECTION ( 'NONE',  ( 0.000000000000000000, 1.000000000000000000, 0.000000000000000000 ) ) ;
#23990 = VERTEX_POINT ( 'NONE', #8620 ) ;
#23991 = EDGE_CURVE ( 'NONE', #16019, #12864, #25614, .T. ) ;
#23992 = CARTESIAN_POINT ( 'NONE',  ( 9.766261594859265927, -13.96654203752514967, 7.652108011868850035 ) ) ;
#23993 = CARTESIAN_POINT ( 'NONE',  ( 15.81416325002591527, -6.360572704314728654, 5.652196082367003882 ) ) ;
#23994 = CARTESIAN_POINT ( 'NONE',  ( -2.959227181723746547, 8.499586724479465616, -3.621320343559650379 ) ) ;
#23995 = CARTESIAN_POINT ( 'NONE',  ( -5.971396161871752817, 19.08775596758252036, 20.34789198813115263 ) ) ;
#23996 = ORIENTED_EDGE ( 'NONE', *, *, #1006, .T. ) ;
#23997 = ORIENTED_EDGE ( 'NONE', *, *, #9247, .F. ) ;
#23998 = CARTESIAN_POINT ( 'NONE',  ( 39.87350638640253919, -4.706224724400470016, -11.49999999999999645 ) ) ;
#23999 = DIRECTION ( 'NONE',  ( -1.000000000000000000, 1.040834085586084257E-15, 0.000000000000000000 ) ) ;
#24000 = CARTESIAN_POINT ( 'NONE',  ( 69.99999999999998579, -50.00000000000000000, 12.49999999999999112 ) ) ;
#24001 = CARTESIAN_POINT ( 'NONE',  ( -4.786560543001536772, 16.33923032321832025, 18.71435384576123440 ) ) ;
#24002 = CARTESIAN_POINT ( 'NONE',  ( -10.47960520055065636, -7.757439966934454034, 1.500000000000001332 ) ) ;
#24003 = EDGE_CURVE ( 'NONE', #25279, #30269, #4229, .T. ) ;
#24004 = CARTESIAN_POINT ( 'NONE',  ( 0.000000000000000000, -1.502314598737157848E-15, -9.000000000000001776 ) ) ;
#24005 = ORIENTED_EDGE ( 'NONE', *, *, #24082, .T. ) ;
#24006 = CARTESIAN_POINT ( 'NONE',  ( -2.959227181723746547, 8.499586724479465616, 21.50000000000000000 ) ) ;
#24007 = DIRECTION ( 'NONE',  ( -1.000000000000000000, 0.000000000000000000, 0.000000000000000000 ) ) ;
#24008 = CARTESIAN_POINT ( 'NONE',  ( -32.24119442679361214, -26.76047168400493703, -16.50000600000000262 ) ) ;
#24009 = EDGE_LOOP ( 'NONE', ( #17779, #14076, #18943, #7215 ) ) ;
#24010 = CARTESIAN_POINT ( 'NONE',  ( 15.36220013476732404, 12.83425670785759110, 5.940635272151477686 ) ) ;
#24011 = CARTESIAN_POINT ( 'NONE',  ( -15.26435939152463384, 8.070345032481604619, 24.50000000000000000 ) ) ;
#24012 = CARTESIAN_POINT ( 'NONE',  ( -33.46566279634613039, 23.92259740141228264, -11.49999999999999645 ) ) ;
#24013 = EDGE_CURVE ( 'NONE', #7851, #26358, #8356, .T. ) ;
#24014 = DIRECTION ( 'NONE',  ( 1.000000000000000000, 0.000000000000000000, 0.000000000000000000 ) ) ;
#24015 = VERTEX_POINT ( 'NONE', #18285 ) ;
#24016 = CIRCLE ( 'NONE', #8670, 20.32284676574538906 ) ;
#24017 = AXIS2_PLACEMENT_3D ( 'NONE', #11843, #13725, #18867 ) ;
#24018 = EDGE_CURVE ( 'NONE', #27621, #6819, #21416, .T. ) ;
#24019 = CARTESIAN_POINT ( 'NONE',  ( 5.080682615984644990, 19.36225455879193902, 5.678370764302467677 ) ) ;
#24020 = EDGE_CURVE ( 'NONE', #7300, #11919, #13750, .T. ) ;
#24021 = AXIS2_PLACEMENT_3D ( 'NONE', #82, #25670, #11484 ) ;
#24022 = CARTESIAN_POINT ( 'NONE',  ( 0.8038475772933806329, -10.39230484541329247, 6.144194323733775069E-17 ) ) ;
#24023 = LINE ( 'NONE', #2990, #23768 ) ;
#24024 = CARTESIAN_POINT ( 'NONE',  ( -18.37606348208443663, -7.894877446839462465, 6.033082186765047261 ) ) ;
#24025 = CARTESIAN_POINT ( 'NONE',  ( 0.000000000000000000, 0.000000000000000000, 1.500000000000001332 ) ) ;
#24026 = CARTESIAN_POINT ( 'NONE',  ( 0.000000000000000000, 15.00000000000003375, -87.50000000000000000 ) ) ;
#24027 = EDGE_CURVE ( 'NONE', #977, #10854, #29901, .T. ) ;
#24028 = CARTESIAN_POINT ( 'NONE',  ( -31.22647667302024388, 15.32805873036034505, 40.21452297286847966 ) ) ;
#24029 = VERTEX_POINT ( 'NONE', #23244 ) ;
#24030 = EDGE_CURVE ( 'NONE', #13582, #16299, #21912, .T. ) ;
#24031 = CARTESIAN_POINT ( 'NONE',  ( 15.75996277362376752, -6.485024779661078043, 7.652108011868851811 ) ) ;
#24032 = CARTESIAN_POINT ( 'NONE',  ( -34.07766914599908148, -21.40380666528021081, -1.500000000000000000 ) ) ;
#24033 = DIRECTION ( 'NONE',  ( -0.000000000000000000, -0.000000000000000000, -1.000000000000000000 ) ) ;
#24034 = ORIENTED_EDGE ( 'NONE', *, *, #6342, .F. ) ;
#24035 = LINE ( 'NONE', #5915, #4580 ) ;
#24036 = CARTESIAN_POINT ( 'NONE',  ( -14.77756128048222983, -8.549967187541072988, 19.89182036555910571 ) ) ;
#24038 = EDGE_CURVE ( 'NONE', #4502, #6184, #24051, .T. ) ;
#24037 = DIRECTION ( 'NONE',  ( 1.000000000000000000, 0.000000000000000000, 0.000000000000000000 ) ) ;
#24039 = LINE ( 'NONE', #14844, #10788 ) ;
#24040 = CARTESIAN_POINT ( 'NONE',  ( -5.105024945675580739, -42.22604126506273303, -1.500000000000000000 ) ) ;
#24041 = EDGE_CURVE ( 'NONE', #17088, #27593, #3918, .T. ) ;
#24042 = ORIENTED_EDGE ( 'NONE', *, *, #29953, .F. ) ;
#24043 = DIRECTION ( 'NONE',  ( 1.000000000000000000, 0.000000000000000000, 0.000000000000000000 ) ) ;
#24044 = EDGE_CURVE ( 'NONE', #30524, #27003, #7496, .T. ) ;
#24045 = AXIS2_PLACEMENT_3D ( 'NONE', #22197, #17212, #3182 ) ;
#24046 = CARTESIAN_POINT ( 'NONE',  ( 22.33591402143825277, 34.95758375282650832, 34.50523401540510804 ) ) ;
#24047 = DIRECTION ( 'NONE',  ( 0.000000000000000000, 1.000000000000000000, 1.193512090021232842E-16 ) ) ;
#24048 = VERTEX_POINT ( 'NONE', #7505 ) ;
#24049 = ORIENTED_EDGE ( 'NONE', *, *, #23820, .F. ) ;
#24050 = CARTESIAN_POINT ( 'NONE',  ( -23.21352257770656990, -10.78826658734919519, -16.55003854064094426 ) ) ;
#24051 =( BOUNDED_CURVE ( )  B_SPLINE_CURVE ( 3, ( #6723, #30284, #11114, #1895 ),
 .UNSPECIFIED., .F., .T. ) 
 B_SPLINE_CURVE_WITH_KNOTS ( ( 4, 4 ),
 ( 3.669394294047855443, 5.755383666721523461 ),
 .UNSPECIFIED. ) 
 CURVE ( )  GEOMETRIC_REPRESENTATION_ITEM ( )  RATIONAL_B_SPLINE_CURVE ( ( 1.000000000000000000, 0.6690902406732677221, 0.6690902406732677221, 1.000000000000000000 ) ) 
 REPRESENTATION_ITEM ( '' )  );
#24052 = FACE_OUTER_BOUND ( 'NONE', #1569, .T. ) ;
#24053 = VERTEX_POINT ( 'NONE', #17155 ) ;
#24054 = ORIENTED_EDGE ( 'NONE', *, *, #27092, .T. ) ;
#24055 = CARTESIAN_POINT ( 'NONE',  ( -10.51100883930069863, -17.01524884273342053, 5.652196082369965069 ) ) ;
#24056 = VERTEX_POINT ( 'NONE', #14816 ) ;
#24057 = ORIENTED_EDGE ( 'NONE', *, *, #15090, .F. ) ;
#24058 = CARTESIAN_POINT ( 'NONE',  ( -0.1272161363927089561, -17.02285684280287725, 18.90679857307105749 ) ) ;
#24059 = EDGE_CURVE ( 'NONE', #14477, #17470, #15452, .T. ) ;
#24060 = DIRECTION ( 'NONE',  ( -1.000000000000000000, 0.000000000000000000, 0.000000000000000000 ) ) ;
#24061 = ADVANCED_FACE ( 'NONE', ( #23699 ), #12338, .T. ) ;
#24062 = AXIS2_PLACEMENT_3D ( 'NONE', #6131, #18150, #6596 ) ;
#24063 = CARTESIAN_POINT ( 'NONE',  ( -7.857295329535767259, -15.15488436941561901, 6.041646659195333058 ) ) ;
#24064 = CARTESIAN_POINT ( 'NONE',  ( 4.537114061097054396, 16.41705816686735986, 20.22273502201483453 ) ) ;
#24065 = CARTESIAN_POINT ( 'NONE',  ( 1.327349630778745793, -17.01025715289075535, 18.50655187082627862 ) ) ;
#24066 = ORIENTED_EDGE ( 'NONE', *, *, #15116, .F. ) ;
#24067 = EDGE_CURVE ( 'NONE', #8165, #23071, #25899, .T. ) ;
#24068 = CARTESIAN_POINT ( 'NONE',  ( 18.39103589699441699, -7.860502636612781480, 5.652912763329822177 ) ) ;
#24069 = AXIS2_PLACEMENT_3D ( 'NONE', #18440, #27634, #13740 ) ;
#24070 = DIRECTION ( 'NONE',  ( -0.000000000000000000, -0.000000000000000000, -1.000000000000000000 ) ) ;
#24071 = CARTESIAN_POINT ( 'NONE',  ( 8.065487902651284458, -43.19822004875265264, -16.49999999999999645 ) ) ;
#24072 = CARTESIAN_POINT ( 'NONE',  ( 11.80864398233534907, 12.32734916534601943, 18.73743063545763121 ) ) ;
#24073 = DIRECTION ( 'NONE',  ( 1.000000000000000000, -0.000000000000000000, 0.000000000000000000 ) ) ;
#24074 = ORIENTED_EDGE ( 'NONE', *, *, #25007, .T. ) ;
#24075 = CIRCLE ( 'NONE', #162, 3.559164065751841743 ) ;
#24076 = EDGE_CURVE ( 'NONE', #24787, #2507, #18461, .T. ) ;
#24077 = DIRECTION ( 'NONE',  ( 0.000000000000000000, 1.000000000000000000, 0.000000000000000000 ) ) ;
#24078 = DIRECTION ( 'NONE',  ( 1.000000000000000000, 0.000000000000000000, 0.000000000000000000 ) ) ;
#24079 = CARTESIAN_POINT ( 'NONE',  ( -6.374050743166105981, 15.83881588044504163, 6.131018562779544823 ) ) ;
#24080 = CARTESIAN_POINT ( 'NONE',  ( -19.91205802435384697, 1.875831072725643089, 5.853797745100181693 ) ) ;
#24081 = FACE_OUTER_BOUND ( 'NONE', #24097, .T. ) ;
#24082 = EDGE_CURVE ( 'NONE', #27073, #21045, #14943, .T. ) ;
#24083 = B_SPLINE_CURVE_WITH_KNOTS ( 'NONE', 3,
 ( #28775, #2733, #8035, #17538 ),
 .UNSPECIFIED., .F., .F.,
 ( 4, 4 ),
 ( 2.143643656964903906E-07, 0.003421830178490235450 ),
 .UNSPECIFIED. ) ;
#24084 = CARTESIAN_POINT ( 'NONE',  ( -18.09182123201597747, -8.567353834808583812, 18.34969686940295830 ) ) ;
#24085 = CARTESIAN_POINT ( 'NONE',  ( 38.00000000000000711, 90.00000000000001421, -22.50000000000002487 ) ) ;
#24086 = ORIENTED_EDGE ( 'NONE', *, *, #11278, .T. ) ;
#24087 = ORIENTED_EDGE ( 'NONE', *, *, #23044, .F. ) ;
#24088 = DIRECTION ( 'NONE',  ( 0.000000000000000000, 0.000000000000000000, 1.000000000000000000 ) ) ;
#24089 = CARTESIAN_POINT ( 'NONE',  ( -5.719992972340611104, 19.16498258860013237, 20.32243167357988867 ) ) ;
#24090 = CARTESIAN_POINT ( 'NONE',  ( -12.96319695304515029, 11.04295072071645478, 7.429667576816606278 ) ) ;
#24091 = DIRECTION ( 'NONE',  ( 0.000000000000000000, -0.000000000000000000, -1.000000000000000000 ) ) ;
#24092 = ORIENTED_EDGE ( 'NONE', *, *, #4703, .T. ) ;
#24093 = FACE_OUTER_BOUND ( 'NONE', #26850, .T. ) ;
#24094 = CARTESIAN_POINT ( 'NONE',  ( 9.406652940105985294, -1.195154792889428608, 1.500000000000001332 ) ) ;
#24095 = CIRCLE ( 'NONE', #4685, 0.7500000000000011102 ) ;
#24096 = EDGE_CURVE ( 'NONE', #15632, #18015, #22913, .T. ) ;
#24097 = EDGE_LOOP ( 'NONE', ( #12371, #25996, #12714, #8816 ) ) ;
#24098 = CARTESIAN_POINT ( 'NONE',  ( 4.930301257365631962, 16.29355789806660582, 19.77662771831109367 ) ) ;
#24099 = AXIS2_PLACEMENT_3D ( 'NONE', #23063, #1428, #3756 ) ;
#24100 = CARTESIAN_POINT ( 'NONE',  ( 12.20938699334973165, 11.90340052968386075, 7.627891251804737927 ) ) ;
#24101 = EDGE_CURVE ( 'NONE', #26855, #9450, #12975, .T. ) ;
#24102 = DIRECTION ( 'NONE',  ( -0.000000000000000000, -0.000000000000000000, -1.000000000000000000 ) ) ;
#24103 = CARTESIAN_POINT ( 'NONE',  ( -25.60051251894998003, 32.07260926886260677, 34.51546816935509554 ) ) ;
#24104 = EDGE_LOOP ( 'NONE', ( #13912, #6649, #5553, #28680 ) ) ;
#24105 = CARTESIAN_POINT ( 'NONE',  ( 0.000000000000000000, 42.50000000000000000, 1.500000000000000000 ) ) ;
#24106 = CARTESIAN_POINT ( 'NONE',  ( -65.00000000000000000, -36.86186943028246787, 12.49999999999999112 ) ) ;
#24107 = CYLINDRICAL_SURFACE ( 'NONE', #28779, 1.447898107987198646 ) ;
#24108 = VERTEX_POINT ( 'NONE', #2815 ) ;
#24109 = LINE ( 'NONE', #16945, #13318 ) ;
#24110 = DIRECTION ( 'NONE',  ( 1.000000000000000000, -0.000000000000000000, 0.000000000000000000 ) ) ;
#24111 = LINE ( 'NONE', #16790, #20267 ) ;
#24112 = CARTESIAN_POINT ( 'NONE',  ( -0.6060441907983112886, -20.00878639882294863, 6.310736198168394928 ) ) ;
#24113 = LINE ( 'NONE', #561, #21217 ) ;
#24114 = DIRECTION ( 'NONE',  ( -0.000000000000000000, -0.000000000000000000, -1.000000000000000000 ) ) ;
#24115 = AXIS2_PLACEMENT_3D ( 'NONE', #19307, #28827, #16813 ) ;
#24116 = CARTESIAN_POINT ( 'NONE',  ( 37.60209722150239742, -11.28033150005075136, 11.06618368930695340 ) ) ;
#24117 = PLANE ( 'NONE',  #5421 ) ;
#24118 = ORIENTED_EDGE ( 'NONE', *, *, #3304, .T. ) ;
#24119 = DIRECTION ( 'NONE',  ( 0.000000000000000000, 0.000000000000000000, 1.000000000000000000 ) ) ;
#24120 = DIRECTION ( 'NONE',  ( 0.6707505147970024284, -0.7416830501633134842, 0.000000000000000000 ) ) ;
#24121 = ORIENTED_EDGE ( 'NONE', *, *, #7324, .T. ) ;
#24122 = ORIENTED_EDGE ( 'NONE', *, *, #15547, .F. ) ;
#24123 = FACE_OUTER_BOUND ( 'NONE', #16220, .T. ) ;
#24124 = LINE ( 'NONE', #14767, #15362 ) ;
#24125 = ORIENTED_EDGE ( 'NONE', *, *, #29575, .F. ) ;
#24126 = CARTESIAN_POINT ( 'NONE',  ( -50.00000000000000000, -67.00000000000000000, 62.49999999999999289 ) ) ;
#24127 = CARTESIAN_POINT ( 'NONE',  ( -9.310272263096074141, -14.25176022191445391, 6.211014596808754007 ) ) ;
#24128 = EDGE_LOOP ( 'NONE', ( #15432, #5237, #13093, #10745 ) ) ;
#24129 = CARTESIAN_POINT ( 'NONE',  ( 15.84452017418781367, -6.290821626254204268, 18.34838970509067479 ) ) ;
#24130 = CARTESIAN_POINT ( 'NONE',  ( 19.58381725123994244, 4.144794415032112767, 19.03762469184452755 ) ) ;
#24131 = EDGE_CURVE ( 'NONE', #3032, #14088, #14192, .T. ) ;
#24132 = CARTESIAN_POINT ( 'NONE',  ( -25.88604317058895532, 6.345278376181626712, 48.34797144667707869 ) ) ;
#24133 = ORIENTED_EDGE ( 'NONE', *, *, #21808, .T. ) ;
#24134 = ADVANCED_FACE ( 'NONE', ( #14513 ), #21840, .F. ) ;
#24135 = CARTESIAN_POINT ( 'NONE',  ( 23.15419545472248686, -10.94206393902796925, 45.14840622133245063 ) ) ;
#24136 = VECTOR ( 'NONE', #17401, 1000.000000000000000 ) ;
#24137 = ORIENTED_EDGE ( 'NONE', *, *, #24255, .T. ) ;
#24138 = ORIENTED_EDGE ( 'NONE', *, *, #27729, .F. ) ;
#24139 = CIRCLE ( 'NONE', #1259, 20.00000000000000000 ) ;
#24140 = LINE ( 'NONE', #17128, #26036 ) ;
#24141 = CARTESIAN_POINT ( 'NONE',  ( -6.240920525956804354, 15.88642679632095600, 18.64703902303423178 ) ) ;
#24142 = CARTESIAN_POINT ( 'NONE',  ( 49.99999999999998579, 87.00000000000001421, 22.49999999999999289 ) ) ;
#24143 = CARTESIAN_POINT ( 'NONE',  ( -9.723733991145053324, -17.49730778217156413, 18.92976555901915603 ) ) ;
#24144 = CARTESIAN_POINT ( 'NONE',  ( -27.37266257347463494, -30.39118854371129075, 30.00740378720065493 ) ) ;
#24145 = DIRECTION ( 'NONE',  ( -0.000000000000000000, -0.000000000000000000, 1.000000000000000000 ) ) ;
#24146 = DIRECTION ( 'NONE',  ( 0.000000000000000000, 0.000000000000000000, 1.000000000000000000 ) ) ;
#24147 = ORIENTED_EDGE ( 'NONE', *, *, #23562, .T. ) ;
#24148 = CARTESIAN_POINT ( 'NONE',  ( 10.66524827722686197, -16.94040236790928944, 5.796888747622817029 ) ) ;
#24149 = CARTESIAN_POINT ( 'NONE',  ( 31.11989886121315863, -19.96255629701192902, 34.50000000000000000 ) ) ;
#24150 = CARTESIAN_POINT ( 'NONE',  ( -15.56646378676711784, 12.58598989586693939, 7.603368798681074736 ) ) ;
#24151 = CYLINDRICAL_SURFACE ( 'NONE', #8823, 2.000000000000001776 ) ;
#24152 = VERTEX_POINT ( 'NONE', #18897 ) ;
#24153 = VERTEX_POINT ( 'NONE', #24008 ) ;
#24154 = CIRCLE ( 'NONE', #15199, 9.084132297865673777 ) ;
#24155 = FACE_OUTER_BOUND ( 'NONE', #23793, .T. ) ;
#24156 = CARTESIAN_POINT ( 'NONE',  ( -5.364573742045088522, 19.28565133533678733, 7.429667576816606278 ) ) ;
#24157 = CARTESIAN_POINT ( 'NONE',  ( 8.840471615930072247, -1.687027447297460236, 1.500000000000001332 ) ) ;
#24158 = CARTESIAN_POINT ( 'NONE',  ( -5.196396160405787334, 19.31337320890706977, 7.267242832833944455 ) ) ;
#24159 = VERTEX_POINT ( 'NONE', #7653 ) ;
#24160 = VERTEX_POINT ( 'NONE', #26676 ) ;
#24161 = CARTESIAN_POINT ( 'NONE',  ( -27.81955209195762180, -25.07120904824700958, 34.50000000000000711 ) ) ;
#24162 = DIRECTION ( 'NONE',  ( 1.000000000000000000, 0.000000000000000000, 0.000000000000000000 ) ) ;
#24163 = CARTESIAN_POINT ( 'NONE',  ( -4.163336342344337027E-14, -1.387778780781445676E-14, 1.500000000000000000 ) ) ;
#24164 = VERTEX_POINT ( 'NONE', #5305 ) ;
#24165 = FACE_OUTER_BOUND ( 'NONE', #3275, .T. ) ;
#24166 = VERTEX_POINT ( 'NONE', #7030 ) ;
#24167 = DIRECTION ( 'NONE',  ( -0.000000000000000000, -0.000000000000000000, -1.000000000000000000 ) ) ;
#24168 = UNCERTAINTY_MEASURE_WITH_UNIT (LENGTH_MEASURE( 1.000000000000000082E-05 ), #1361, 'distance_accuracy_value', 'NONE');
#24169 = DIRECTION ( 'NONE',  ( -0.000000000000000000, -0.000000000000000000, 1.000000000000000000 ) ) ;
#24170 = FACE_OUTER_BOUND ( 'NONE', #30576, .T. ) ;
#24171 = VERTEX_POINT ( 'NONE', #2659 ) ;
#24172 = VECTOR ( 'NONE', #28896, 1000.000000000000000 ) ;
#24173 = CARTESIAN_POINT ( 'NONE',  ( 3.718735505629741311, 16.64535199026476420, 5.704143890883081269 ) ) ;
#24174 = CARTESIAN_POINT ( 'NONE',  ( -23.21352257770656990, 10.78826658734919519, -16.55003854064094426 ) ) ;
#24175 = ORIENTED_EDGE ( 'NONE', *, *, #23095, .T. ) ;
#24176 = CARTESIAN_POINT ( 'NONE',  ( -22.58267429318971864, 26.57182937991348481, -6.499999999999999112 ) ) ;
#24177 = CIRCLE ( 'NONE', #8287, 0.7500000000000004441 ) ;
#24178 = CARTESIAN_POINT ( 'NONE',  ( -13.11527592942575282, -10.04126165406389326, -0.6213203435596476032 ) ) ;
#24179 = CARTESIAN_POINT ( 'NONE',  ( 9.489008252200360261, -14.14611184196830784, 20.25336174263950184 ) ) ;
#24180 = CARTESIAN_POINT ( 'NONE',  ( 33.56327786402390245, 10.46063060613185414, 39.84455206157484497 ) ) ;
#24181 = ORIENTED_EDGE ( 'NONE', *, *, #27114, .T. ) ;
#24182 = FACE_OUTER_BOUND ( 'NONE', #30613, .T. ) ;
#24183 = CARTESIAN_POINT ( 'NONE',  ( -5.105024945675580739, -42.22604126506273303, -1.500000000000000000 ) ) ;
#24184 = AXIS2_PLACEMENT_3D ( 'NONE', #11318, #4280, #18494 ) ;
#24185 = FACE_OUTER_BOUND ( 'NONE', #30609, .T. ) ;
#24186 = VERTEX_POINT ( 'NONE', #16539 ) ;
#24187 = CARTESIAN_POINT ( 'NONE',  ( -17.62838677698389489, -9.483948870226237560, 19.69140814234746273 ) ) ;
#24188 = CARTESIAN_POINT ( 'NONE',  ( -9.062880100047301823, -0.6210184355499139830, 21.50000000000000000 ) ) ;
#24189 = LINE ( 'NONE', #2842, #29777 ) ;
#24190 = CARTESIAN_POINT ( 'NONE',  ( -1.438332125858111432, 8.884323311075791096, -3.621320343559650379 ) ) ;
#24191 = CARTESIAN_POINT ( 'NONE',  ( -2.687479362164884034, -44.39187623478217404, -19.50000000000000355 ) ) ;
#24192 = DIRECTION ( 'NONE',  ( 0.000000000000000000, 0.000000000000000000, 1.000000000000000000 ) ) ;
#24193 = AXIS2_PLACEMENT_3D ( 'NONE', #18574, #21501, #2179 ) ;
#24194 = CARTESIAN_POINT ( 'NONE',  ( 38.72184494665977184, 5.684323948905047885, 32.14431142672166430 ) ) ;
#24195 = EDGE_CURVE ( 'NONE', #1845, #26490, #19443, .T. ) ;
#24196 = CARTESIAN_POINT ( 'NONE',  ( -4.163336342344337027E-14, 1.387778780781445676E-14, 1.500000000000000000 ) ) ;
#24197 = ORIENTED_EDGE ( 'NONE', *, *, #436, .T. ) ;
#24198 = CIRCLE ( 'NONE', #17763, 0.7441270634457319844 ) ;
#24199 = CARTESIAN_POINT ( 'NONE',  ( 9.249586724479433641, 2.959227181723830036, 1.500000000000001332 ) ) ;
#24200 = ORIENTED_EDGE ( 'NONE', *, *, #21361, .T. ) ;
#24201 = CARTESIAN_POINT ( 'NONE',  ( 25.47847050916411504, 26.57182937991349903, 26.54355021145562787 ) ) ;
#24202 = CARTESIAN_POINT ( 'NONE',  ( 0.000000000000000000, -2.435693370351110282E-15, 21.50000000000000355 ) ) ;
#24203 = ORIENTED_EDGE ( 'NONE', *, *, #12625, .T. ) ;
#24204 = EDGE_CURVE ( 'NONE', #30053, #19615, #27409, .T. ) ;
#24205 = ORIENTED_EDGE ( 'NONE', *, *, #22148, .F. ) ;
#24206 = DIRECTION ( 'NONE',  ( 1.000000000000000000, 0.000000000000000000, 0.000000000000000000 ) ) ;
#24207 = EDGE_CURVE ( 'NONE', #25420, #24589, #495, .T. ) ;
#24208 = CIRCLE ( 'NONE', #12275, 0.7500000000000006661 ) ;
#24209 = ORIENTED_EDGE ( 'NONE', *, *, #8049, .F. ) ;
#24210 = EDGE_LOOP ( 'NONE', ( #17500, #29597, #22777, #1856 ) ) ;
#24211 = CARTESIAN_POINT ( 'NONE',  ( -0.3606176111512355287, -20.01462698034515242, 18.63641924841378028 ) ) ;
#24212 = EDGE_CURVE ( 'NONE', #5571, #30328, #17946, .T. ) ;
#24213 = LINE ( 'NONE', #14864, #3327 ) ;
#24214 = FACE_OUTER_BOUND ( 'NONE', #772, .T. ) ;
#24215 = CARTESIAN_POINT ( 'NONE',  ( 5.015798959889849584, 16.26549279019886995, 19.21496526180054332 ) ) ;
#24216 = EDGE_CURVE ( 'NONE', #1741, #28813, #3589, .T. ) ;
#24217 = CARTESIAN_POINT ( 'NONE',  ( -22.21046885174908425, 23.49239644259613158, -16.50001200000000168 ) ) ;
#24218 = VERTEX_POINT ( 'NONE', #19806 ) ;
#24220 = ADVANCED_FACE ( 'NONE', ( #768 ), #29830, .T. ) ;
#24219 = AXIS2_PLACEMENT_3D ( 'NONE', #7920, #26317, #267 ) ;
#24221 = DIRECTION ( 'NONE',  ( 0.000000000000000000, 0.000000000000000000, -1.000000000000000000 ) ) ;
#24222 = FACE_OUTER_BOUND ( 'NONE', #3909, .T. ) ;
#24223 = CARTESIAN_POINT ( 'NONE',  ( 11.75961732103505497, 12.37772240090665932, 18.82680253904184298 ) ) ;
#24224 = CYLINDRICAL_SURFACE ( 'NONE', #21074, 0.7500000000000002220 ) ;
#24225 = ORIENTED_EDGE ( 'NONE', *, *, #30481, .T. ) ;
#24226 = CIRCLE ( 'NONE', #20252, 12.66227964008302287 ) ;
#24227 = AXIS2_PLACEMENT_3D ( 'NONE', #514, #10341, #24206 ) ;
#24228 = CARTESIAN_POINT ( 'NONE',  ( -37.99999999999999289, 70.00000000000000000, -75.50000000000000000 ) ) ;
#24229 = DIRECTION ( 'NONE',  ( 0.000000000000000000, 0.000000000000000000, -1.000000000000000000 ) ) ;
#24230 = CARTESIAN_POINT ( 'NONE',  ( -6.509484584620659930, 15.78915919539661949, 6.560937769032974209 ) ) ;
#24231 = CARTESIAN_POINT ( 'NONE',  ( -19.87571927687823248, 2.229464111918809888, 5.679672709359370408 ) ) ;
#24232 = CARTESIAN_POINT ( 'NONE',  ( -23.15749938697695143, 12.07134380388760242, 44.64257729857385470 ) ) ;
#24233 = CARTESIAN_POINT ( 'NONE',  ( -18.46504858183724096, -7.730374101464834169, 19.11611934778430921 ) ) ;
#24234 = LINE ( 'NONE', #2886, #30536 ) ;
#24235 = VECTOR ( 'NONE', #28427, 1000.000000000000000 ) ;
#24236 = VERTEX_POINT ( 'NONE', #22756 ) ;
#24237 = VERTEX_POINT ( 'NONE', #4192 ) ;
#24238=STYLED_ITEM('',(#30900),#2811);
#24239 = DIRECTION ( 'NONE',  ( -1.000000000000000000, 0.000000000000000000, 0.000000000000000000 ) ) ;
#24240 = EDGE_CURVE ( 'NONE', #699, #6203, #28400, .T. ) ;
#24241 = CARTESIAN_POINT ( 'NONE',  ( -14.68399241520484466, 13.60504237629023017, 6.641371103590088865 ) ) ;
#24242 = ADVANCED_FACE ( 'NONE', ( #10931 ), #27765, .F. ) ;
#24243 = DIRECTION ( 'NONE',  ( -0.000000000000000000, 1.000000000000000000, -0.000000000000000000 ) ) ;
#24244 = ORIENTED_EDGE ( 'NONE', *, *, #2531, .F. ) ;
#24245 = SHAPE_DEFINITION_REPRESENTATION ( #28600, #19685 ) ;
#24246 = EDGE_CURVE ( 'NONE', #19828, #17963, #1702, .T. ) ;
#24247 = DIRECTION ( 'NONE',  ( 0.000000000000000000, 0.000000000000000000, 1.000000000000000000 ) ) ;
#24248 = CIRCLE ( 'NONE', #25259, 0.7500000000000002220 ) ;
#24249 = ADVANCED_FACE ( 'NONE', ( #23054, #29951 ), #15740, .T. ) ;
#24250 = CARTESIAN_POINT ( 'NONE',  ( -10.51513057463695411, -17.01270198993486460, 7.652108011868850035 ) ) ;
#24251 = AXIS2_PLACEMENT_3D ( 'NONE', #20050, #873, #10395 ) ;
#24252 = VERTEX_POINT ( 'NONE', #15911 ) ;
#24253 = CARTESIAN_POINT ( 'NONE',  ( -24.44496207165490276, -7.595930209050158588, 45.15942333309111234 ) ) ;
#24254 = VECTOR ( 'NONE', #10157, 1000.000000000000000 ) ;
#24255 = EDGE_CURVE ( 'NONE', #17054, #12148, #11384, .T. ) ;
#24256 = CARTESIAN_POINT ( 'NONE',  ( -23.07950435457351190, 11.50806656539842798, 44.96784366550151191 ) ) ;
#24257 = AXIS2_PLACEMENT_3D ( 'NONE', #21436, #7564, #23930 ) ;
#24258 = CARTESIAN_POINT ( 'NONE',  ( -9.301547456646385825, 8.591538895647085283, 1.500000000000000000 ) ) ;
#24259 = CARTESIAN_POINT ( 'NONE',  ( -31.76737364660611718, -19.96634320003312268, 37.49999999999806022 ) ) ;
#24260 = ORIENTED_EDGE ( 'NONE', *, *, #21027, .T. ) ;
#24261 = EDGE_CURVE ( 'NONE', #10933, #16535, #21931, .T. ) ;
#24262 = CARTESIAN_POINT ( 'NONE',  ( -23.62400240902268322, 9.724154461249517212, 49.47829057475703962 ) ) ;
#24263 = EDGE_CURVE ( 'NONE', #23828, #30256, #23205, .T. ) ;
#24264 = CARTESIAN_POINT ( 'NONE',  ( 32.60641126234700238, 8.625635766581060793, 37.02940160128806468 ) ) ;
#24265 = CIRCLE ( 'NONE', #25273, 1.447898107987170890 ) ;
#24266 = CARTESIAN_POINT ( 'NONE',  ( 14.24118286736276850, 41.28857907310604958, -16.50000000000000355 ) ) ;
#24267 = AXIS2_PLACEMENT_3D ( 'NONE', #21780, #417, #15204 ) ;
#24268 = ORIENTED_EDGE ( 'NONE', *, *, #5186, .T. ) ;
#24269 = CARTESIAN_POINT ( 'NONE',  ( -15.39003174319561218, -7.295547530644704182, 5.796888747622817029 ) ) ;
#24270 = DIRECTION ( 'NONE',  ( 0.000000000000000000, 1.000000000000000000, 0.000000000000000000 ) ) ;
#24271 = CARTESIAN_POINT ( 'NONE',  ( -0.6388627779519707728, -20.00771244368418067, 6.420335371522007506 ) ) ;
#24272 = CIRCLE ( 'NONE', #11833, 9.482273699623480212 ) ;
#24273 = CARTESIAN_POINT ( 'NONE',  ( 0.000000000000000000, 0.000000000000000000, -52.50000000000000000 ) ) ;
#24274 = AXIS2_PLACEMENT_3D ( 'NONE', #6205, #27431, #5897 ) ;
#24275 = DIRECTION ( 'NONE',  ( -1.000000000000000000, -0.000000000000000000, -0.000000000000000000 ) ) ;
#24276 = CARTESIAN_POINT ( 'NONE',  ( 37.92106016242558297, -9.928229530987605855, 12.17473369872427291 ) ) ;
#24277 = CARTESIAN_POINT ( 'NONE',  ( -4.776122516674677878E-15, -42.50000000000000000, 27.50000000000000355 ) ) ;
#24278 = EDGE_LOOP ( 'NONE', ( #1719, #5714, #18211, #13712, #29244, #4405 ) ) ;
#24279 = EDGE_CURVE ( 'NONE', #20523, #19687, #13967, .T. ) ;
#24280 = EDGE_CURVE ( 'NONE', #15207, #26111, #9183, .T. ) ;
#24281 = CYLINDRICAL_SURFACE ( 'NONE', #27222, 2.061368542273053883 ) ;
#24282 = CIRCLE ( 'NONE', #30727, 0.7500000000000006661 ) ;
#24283 = CARTESIAN_POINT ( 'NONE',  ( 9.184850993605161750E-16, -7.500000000000018652, -1.500000000000002220 ) ) ;
#24284 = VERTEX_POINT ( 'NONE', #20716 ) ;
#24285 = DIRECTION ( 'NONE',  ( 1.000000000000000000, 0.000000000000000000, 0.000000000000000000 ) ) ;
#24286 = EDGE_CURVE ( 'NONE', #4162, #3753, #4345, .T. ) ;
#24287 = AXIS2_PLACEMENT_3D ( 'NONE', #11640, #4930, #25994 ) ;
#24288 = CARTESIAN_POINT ( 'NONE',  ( -0.9972762135841950482, 50.00000000000001421, -40.00000000000002132 ) ) ;
#24289 = VECTOR ( 'NONE', #18913, 1000.000000000000000 ) ;
#24290 = VERTEX_POINT ( 'NONE', #13870 ) ;
#24291 = CIRCLE ( 'NONE', #8879, 0.7500000000000006661 ) ;
#24292 = CARTESIAN_POINT ( 'NONE',  ( 12.64536614603775888, 11.41255465792765378, 18.44501272782439827 ) ) ;
#24293 = CARTESIAN_POINT ( 'NONE',  ( -8.643687819870516265, -14.68753251638875845, 5.657991946698900598 ) ) ;
#24294 = ORIENTED_EDGE ( 'NONE', *, *, #18157, .F. ) ;
#24295 = CARTESIAN_POINT ( 'NONE',  ( 16.14429390779610785, -5.555032456232098959, 18.82680253904184298 ) ) ;
#24296 = CARTESIAN_POINT ( 'NONE',  ( 16.68596330270455752, 3.532048315275336581, 18.39992786714538298 ) ) ;
#24297 = CIRCLE ( 'NONE', #3397, 2.061368542273053883 ) ;
#24298 = FACE_OUTER_BOUND ( 'NONE', #30604, .T. ) ;
#24299 = VERTEX_POINT ( 'NONE', #1562 ) ;
#24300 = VECTOR ( 'NONE', #28458, 1000.000000000000000 ) ;
#24301 = CARTESIAN_POINT ( 'NONE',  ( 15.81416692036122207, -6.360574302898111654, 18.34798005863078885 ) ) ;
#24302 = VERTEX_POINT ( 'NONE', #18696 ) ;
#24303 = ORIENTED_EDGE ( 'NONE', *, *, #23820, .T. ) ;
#24304 = AXIS2_PLACEMENT_3D ( 'NONE', #1852, #30396, #19002 ) ;
#24305 = CARTESIAN_POINT ( 'NONE',  ( -7.706848733600993206, -5.524309650260738280, 21.50000000000000000 ) ) ;
#24306 = CARTESIAN_POINT ( 'NONE',  ( -6.507320782993286201, 15.78995902672676621, 19.36813350477385143 ) ) ;
#24307 = CARTESIAN_POINT ( 'NONE',  ( -14.69323076807464545, 13.59505578765952727, 19.22654678686458141 ) ) ;
#24308 = AXIS2_PLACEMENT_3D ( 'NONE', #9515, #4829, #14345 ) ;
#24309 = CARTESIAN_POINT ( 'NONE',  ( -8.413215745754975217, 3.196529495465474380, -3.621320343559650379 ) ) ;
#24310 = CARTESIAN_POINT ( 'NONE',  ( -25.60834283456843963, 32.16668900101505812, 29.82420505145413969 ) ) ;
#24311 = CARTESIAN_POINT ( 'NONE',  ( 7.724883619896791842, 5.687793815610376669, 1.500000000000001332 ) ) ;
#24312 = CARTESIAN_POINT ( 'NONE',  ( 8.499586724479435418, 2.959227181723830036, 1.500000000000001332 ) ) ;
#24313 = EDGE_CURVE ( 'NONE', #1903, #9741, #28419, .T. ) ;
#24314 = CARTESIAN_POINT ( 'NONE',  ( -16.97503503882430209, 1.572081968053592904, 5.652605728828373977 ) ) ;
#24315 = CARTESIAN_POINT ( 'NONE',  ( -28.06227104053563082, 29.51396674875200077, 13.88771667678369148 ) ) ;
#24316 = VECTOR ( 'NONE', #5402, 1000.000000000000000 ) ;
#24317 = CARTESIAN_POINT ( 'NONE',  ( 19.83258132550259845, 2.584089194578472970, 5.849008070840543638 ) ) ;
#24318 = ORIENTED_EDGE ( 'NONE', *, *, #26386, .F. ) ;
#24319 = VERTEX_POINT ( 'NONE', #11071 ) ;
#24320 = LINE ( 'NONE', #17143, #16318 ) ;
#24321 = CARTESIAN_POINT ( 'NONE',  ( 10.42970548045642509, -17.06546344489797207, 6.033082186765059696 ) ) ;
#24322 = FACE_OUTER_BOUND ( 'NONE', #9081, .T. ) ;
#24323 = DIRECTION ( 'NONE',  ( -1.000000000000000000, 0.000000000000000000, 0.000000000000000000 ) ) ;
#24324 = CARTESIAN_POINT ( 'NONE',  ( 0.000000000000000000, 0.000000000000000000, -87.50000000000000000 ) ) ;
#24325 = CARTESIAN_POINT ( 'NONE',  ( 8.539720164285627899E-15, -30.50000000000000711, 1.500000000000001332 ) ) ;
#24326 = EDGE_CURVE ( 'NONE', #27034, #14242, #28048, .T. ) ;
#24327 = ORIENTED_EDGE ( 'NONE', *, *, #22763, .F. ) ;
#24328 = AXIS2_PLACEMENT_3D ( 'NONE', #7910, #1190, #25041 ) ;
#24329 = DIRECTION ( 'NONE',  ( -0.000000000000000000, -0.000000000000000000, 1.000000000000000000 ) ) ;
#24330 = DIRECTION ( 'NONE',  ( 1.000000000000000000, 0.000000000000000000, 0.000000000000000000 ) ) ;
#24331 = AXIS2_PLACEMENT_3D ( 'NONE', #9518, #10414, #24746 ) ;
#24332 = DIRECTION ( 'NONE',  ( 0.000000000000000000, 0.000000000000000000, 1.000000000000000000 ) ) ;
#24333 = VERTEX_POINT ( 'NONE', #25107 ) ;
#24334 = FACE_OUTER_BOUND ( 'NONE', #12304, .T. ) ;
#24335 = ORIENTED_EDGE ( 'NONE', *, *, #18316, .F. ) ;
#24336 = CARTESIAN_POINT ( 'NONE',  ( 16.08779849516156446, -5.700297231796353614, 7.366751648393900176 ) ) ;
#24337 = DIRECTION ( 'NONE',  ( 0.000000000000000000, 0.000000000000000000, 1.000000000000000000 ) ) ;
#24338 = AXIS2_PLACEMENT_3D ( 'NONE', #30642, #28331, #16007 ) ;
#24339 = CARTESIAN_POINT ( 'NONE',  ( -11.21147646446735102, -30.29926891764210595, -1.500000000000000000 ) ) ;
#24340 = ORIENTED_EDGE ( 'NONE', *, *, #29680, .T. ) ;
#24341 = CARTESIAN_POINT ( 'NONE',  ( 5.298969250677092013, 19.30368332842023094, 5.652196082364323360 ) ) ;
#24342 = DIRECTION ( 'NONE',  ( 0.000000000000000000, -1.132880637372608986E-16, 1.000000000000000000 ) ) ;
#24343 = CARTESIAN_POINT ( 'NONE',  ( -4.163336342344337027E-14, 1.387778780781445676E-14, 24.50000000000000000 ) ) ;
#24344 = CARTESIAN_POINT ( 'NONE',  ( 32.01792732732114644, 18.17191813560462066, 34.49999999999999289 ) ) ;
#24345 = LINE ( 'NONE', #27318, #23832 ) ;
#24346 = DIRECTION ( 'NONE',  ( -0.000000000000000000, -0.000000000000000000, -1.000000000000000000 ) ) ;
#24347 = ORIENTED_EDGE ( 'NONE', *, *, #21757, .F. ) ;
#24348 = CARTESIAN_POINT ( 'NONE',  ( 24.86084284002701850, 6.930828199065646622, 49.19141369485814863 ) ) ;
#24349 = CARTESIAN_POINT ( 'NONE',  ( -8.303920738747237351, -3.683253992019804191, 13.22130136205108819 ) ) ;
#24350 = VECTOR ( 'NONE', #23931, 1000.000000000000000 ) ;
#24351 = EDGE_CURVE ( 'NONE', #29295, #30416, #22473, .T. ) ;
#24352 = CARTESIAN_POINT ( 'NONE',  ( -15.57270467870639052, 12.57827228024024713, 18.39992786714538298 ) ) ;
#24353 = FACE_OUTER_BOUND ( 'NONE', #8264, .T. ) ;
#24354 = ORIENTED_EDGE ( 'NONE', *, *, #24394, .T. ) ;
#24355 = CARTESIAN_POINT ( 'NONE',  ( 30.54239299898967630, -26.43236169747734721, 8.629833734104749965 ) ) ;
#24356 = CARTESIAN_POINT ( 'NONE',  ( -46.04937532021984481, 69.44700638503979917, 60.46533948008040937 ) ) ;
#24357 = B_SPLINE_CURVE_WITH_KNOTS ( 'NONE', 3,
 ( #5301, #17624, #12492, #5623, #14812, #7797, #27296, #934, #3584, #21984, #1092, #5465, #20116, #29634, #17474, #14967, #12795, #10132 ),
 .UNSPECIFIED., .F., .F.,
 ( 4, 2, 2, 2, 2, 2, 2, 2, 4 ),
 ( 0.003174295595554332133, 0.003570702171545570968, 0.003967108747536809803, 0.004363515323528049071, 0.004759921899519287472, 0.005156328475510526740, 0.005552735051501766009, 0.005949141627493005277, 0.006345548203484243678 ),
 .UNSPECIFIED. ) ;
#24358 = CARTESIAN_POINT ( 'NONE',  ( -50.00000000000000000, -50.00000000000000000, 12.49999999999999112 ) ) ;
#24359 = CARTESIAN_POINT ( 'NONE',  ( 4.176140024716620047, 16.52246432929376496, 7.652108011868850035 ) ) ;
#24360 = CARTESIAN_POINT ( 'NONE',  ( -20.65888525914099105, 38.75220717792564784, -19.50000000000000355 ) ) ;
#24361 = CIRCLE ( 'NONE', #10432, 0.7500000000000006661 ) ;
#24362 = DIRECTION ( 'NONE',  ( 0.000000000000000000, -0.000000000000000000, -1.000000000000000000 ) ) ;
#24363 = CARTESIAN_POINT ( 'NONE',  ( 16.87858066272421809, 2.200498455867148984, 6.782064869129510676 ) ) ;
#24364 = CARTESIAN_POINT ( 'NONE',  ( 49.99999999999998579, -70.00000000000000000, -92.50000000000000000 ) ) ;
#24365 = ORIENTED_EDGE ( 'NONE', *, *, #210, .T. ) ;
#24366 = CIRCLE ( 'NONE', #4452, 0.7500000000000002220 ) ;
#24367 = PLANE ( 'NONE',  #21280 ) ;
#24368 = ORIENTED_EDGE ( 'NONE', *, *, #8447, .T. ) ;
#24369 = CARTESIAN_POINT ( 'NONE',  ( -23.07950435457407679, -11.50806656539752737, 44.96784366550136980 ) ) ;
#24370 = CYLINDRICAL_SURFACE ( 'NONE', #4, 9.482273699623480212 ) ;
#24371 = EDGE_LOOP ( 'NONE', ( #29582, #1531 ) ) ;
#24372 = EDGE_LOOP ( 'NONE', ( #7726, #11822, #11307, #13864, #589, #21408 ) ) ;
#24373 = CARTESIAN_POINT ( 'NONE',  ( 1.964582201835851638, -2.267248723062833538, 24.50000000000000000 ) ) ;
#24374 = PRODUCT_DEFINITION_SHAPE ( 'NONE', 'NONE',  #10487 ) ;
#24375 = AXIS2_PLACEMENT_3D ( 'NONE', #26597, #5223, #17686 ) ;
#24376 = ORIENTED_EDGE ( 'NONE', *, *, #4412, .F. ) ;
#24377 = VERTEX_POINT ( 'NONE', #16509 ) ;
#24378 = CARTESIAN_POINT ( 'NONE',  ( -28.78283879316666471, -7.125616703334840984, 45.34931131770227353 ) ) ;
#24379 = CARTESIAN_POINT ( 'NONE',  ( -7.031646814991431071, 38.74271536321815290, 34.49999999999999289 ) ) ;
#24380 = DIRECTION ( 'NONE',  ( 1.000000000000000000, 0.000000000000000000, 0.000000000000000000 ) ) ;
#24381 = CARTESIAN_POINT ( 'NONE',  ( 7.341751895053238108, -5.349779314757616255, 21.50000000000000000 ) ) ;
#24382 = CARTESIAN_POINT ( 'NONE',  ( -28.78283879316666471, 7.125616703334840984, 41.10667063058299675 ) ) ;
#24383 = ORIENTED_EDGE ( 'NONE', *, *, #14898, .T. ) ;
#24384 = EDGE_CURVE ( 'NONE', #17083, #6797, #1039, .T. ) ;
#24385 = DIRECTION ( 'NONE',  ( 0.000000000000000000, 1.000000000000000000, 0.000000000000000000 ) ) ;
#24386 = CARTESIAN_POINT ( 'NONE',  ( 1.424502173535766802, -17.00587888132690395, 5.872146474157316831 ) ) ;
#24387 = CARTESIAN_POINT ( 'NONE',  ( 0.000000000000000000, 0.000000000000000000, 24.50000000000000000 ) ) ;
#24388 = ORIENTED_EDGE ( 'NONE', *, *, #9196, .F. ) ;
#24389 = VECTOR ( 'NONE', #28937, 1000.000000000000000 ) ;
#24390 = DIRECTION ( 'NONE',  ( 1.000000000000000000, 0.000000000000000000, 0.000000000000000000 ) ) ;
#24391 = DIRECTION ( 'NONE',  ( 0.000000000000000000, 0.000000000000000000, 1.000000000000000000 ) ) ;
#24392 = CARTESIAN_POINT ( 'NONE',  ( -37.16608720827707657, -51.86186943028246787, 12.49999999999999112 ) ) ;
#24393 = DIRECTION ( 'NONE',  ( 0.8349582046168341209, -0.5503133621338236470, 0.000000000000000000 ) ) ;
#24394 = EDGE_CURVE ( 'NONE', #14635, #16844, #2476, .T. ) ;
#24395 = CARTESIAN_POINT ( 'NONE',  ( 0.000000000000000000, 7.794228634059939154, 4.500000000000010658 ) ) ;
#24396 = CARTESIAN_POINT ( 'NONE',  ( -9.131494062835631809, -2.555255504830933333, 13.00000000000000178 ) ) ;
#24397 = EDGE_LOOP ( 'NONE', ( #20720, #27108, #4018, #21414 ) ) ;
#24398 = DIRECTION ( 'NONE',  ( 0.000000000000000000, 0.000000000000000000, 1.000000000000000000 ) ) ;
#24399 = DIRECTION ( 'NONE',  ( 1.000000000000000000, 0.000000000000000000, 0.000000000000000000 ) ) ;
#24400 = CARTESIAN_POINT ( 'NONE',  ( -15.20706373417739776, 13.01805446572691594, 7.632642797338977658 ) ) ;
#24401 = DIRECTION ( 'NONE',  ( -0.000000000000000000, -0.000000000000000000, 1.000000000000000000 ) ) ;
#24402 = ORIENTED_EDGE ( 'NONE', *, *, #10521, .F. ) ;
#24403 = PRODUCT_CONTEXT ( 'NONE', #17357, 'mechanical' ) ;
#24404 = VECTOR ( 'NONE', #12376, 1000.000000000000000 ) ;
#24405 = CARTESIAN_POINT ( 'NONE',  ( 15.63429980755321225, -6.761683097800862186, 18.44501272782439827 ) ) ;
#24406 = DIRECTION ( 'NONE',  ( 0.000000000000000000, 0.000000000000000000, -1.000000000000000000 ) ) ;
#24407 = EDGE_CURVE ( 'NONE', #22736, #2857, #1280, .T. ) ;
#24408 = ORIENTED_EDGE ( 'NONE', *, *, #2304, .T. ) ;
#24409 = CARTESIAN_POINT ( 'NONE',  ( 4.155601639749238352, 16.52779251924067339, 18.35377592296120497 ) ) ;
#24410 = CARTESIAN_POINT ( 'NONE',  ( -8.430595340551228389, 4.340342926365043930, 21.50000000000000000 ) ) ;
#24411 = CARTESIAN_POINT ( 'NONE',  ( -50.00000000000000000, -50.00000000000000000, 52.07879600563550326 ) ) ;
#24412 = CARTESIAN_POINT ( 'NONE',  ( -31.71888454229558363, -24.74171469661772704, 34.61963941082733243 ) ) ;
#24413 = ORIENTED_EDGE ( 'NONE', *, *, #27082, .F. ) ;
#24414 = FACE_OUTER_BOUND ( 'NONE', #13024, .T. ) ;
#24415 = CARTESIAN_POINT ( 'NONE',  ( 40.05520497557499482, 7.028746409576331011, -16.50000000000000000 ) ) ;
#24416 = CARTESIAN_POINT ( 'NONE',  ( -19.77413607932157902, 2.999736578675611387, 20.22277707861862339 ) ) ;
#24417 = ORIENTED_EDGE ( 'NONE', *, *, #1936, .F. ) ;
#24418 = CARTESIAN_POINT ( 'NONE',  ( -15.16307466657772451, -7.786257835515858261, 5.652196082367002106 ) ) ;
#24419 = LINE ( 'NONE', #9623, #3389 ) ;
#24420 = EDGE_CURVE ( 'NONE', #321, #21094, #13497, .T. ) ;
#24421 = CARTESIAN_POINT ( 'NONE',  ( 14.45728346696244238, 13.82012126338014468, 5.853797745100180805 ) ) ;
#24422 = EDGE_CURVE ( 'NONE', #9325, #9621, #9493, .T. ) ;
#24423 = DIRECTION ( 'NONE',  ( 1.000000000000000000, 0.000000000000000000, 0.000000000000000000 ) ) ;
#24424 = VECTOR ( 'NONE', #24753, 1000.000000000000000 ) ;
#24425 = CARTESIAN_POINT ( 'NONE',  ( -26.31094384852241319, -8.315730187098489878, -16.55003854064094426 ) ) ;
#24426 = B_SPLINE_CURVE_WITH_KNOTS ( 'NONE', 3,
 ( #15528, #25044, #26939, #15059, #24573, #25818, #11474, #20663, #11167, #20817, #1653, #13811, #27999, #23151, #30036, #15994, #25662, #23313, #18035, #8821, #13359, #4282, #8980, #30629 ),
 .UNSPECIFIED., .F., .F.,
 ( 4, 2, 2, 2, 2, 2, 2, 2, 2, 2, 2, 4 ),
 ( 0.000000000000000000, 0.002009081642066640975, 0.003013622463099961679, 0.004018163284133281950, 0.006027244926199938971, 0.007031785747233264446, 0.008036326568266588186, 0.01004540821033321832, 0.01205448985239984845, 0.01305903067343317826, 0.01406357149446650807, 0.01607265313653316596 ),
 .UNSPECIFIED. ) ;
#24427 = CARTESIAN_POINT ( 'NONE',  ( -8.884323311075783991, -1.438332125858144295, -3.621320343559650379 ) ) ;
#24428 = CARTESIAN_POINT ( 'NONE',  ( 37.98270490079809036, -9.643723784870349647, 13.24503139370895077 ) ) ;
#24429 = ADVANCED_FACE ( 'NONE', ( #19466 ), #16361, .F. ) ;
#24430 = DIRECTION ( 'NONE',  ( -1.000000000000000000, 0.000000000000000000, 0.000000000000000000 ) ) ;
#24431 = VERTEX_POINT ( 'NONE', #19158 ) ;
#24432 = ADVANCED_FACE ( 'NONE', ( #7308 ), #18858, .F. ) ;
#24433 = CARTESIAN_POINT ( 'NONE',  ( -5.544451647051929832, 16.11829164193972019, 7.652108011868850923 ) ) ;
#24434 = DIRECTION ( 'NONE',  ( -0.000000000000000000, -0.000000000000000000, 1.000000000000000000 ) ) ;
#24435 = ORIENTED_EDGE ( 'NONE', *, *, #19707, .T. ) ;
#24436 = ORIENTED_EDGE ( 'NONE', *, *, #10703, .T. ) ;
#24437 = EDGE_CURVE ( 'NONE', #19662, #25948, #28375, .T. ) ;
#24438 = CARTESIAN_POINT ( 'NONE',  ( -24.03057240117691862, 26.57182937991348481, -6.499999999999999112 ) ) ;
#24439 = EDGE_CURVE ( 'NONE', #11684, #6919, #30419, .T. ) ;
#24440 = CARTESIAN_POINT ( 'NONE',  ( 1.868132521858655084E-15, 50.00000000000000000, -40.00000000000000711 ) ) ;
#24441 = VERTEX_POINT ( 'NONE', #28677 ) ;
#24442 = CARTESIAN_POINT ( 'NONE',  ( -12.15241004504941991, -37.27483646721038468, 27.50000000000000000 ) ) ;
#24443 = CARTESIAN_POINT ( 'NONE',  ( 15.51850634784530136, 12.64495090725178983, 19.00652017443069752 ) ) ;
#24444 = EDGE_CURVE ( 'NONE', #19956, #2072, #10009, .T. ) ;
#24445 = CARTESIAN_POINT ( 'NONE',  ( -11.12409513110480397, -16.64241105543193555, 5.940635272151477686 ) ) ;
#24446 = VERTEX_POINT ( 'NONE', #21645 ) ;
#24447 = CARTESIAN_POINT ( 'NONE',  ( -19.81587719261256098, 2.836291464538556628, 7.595116371587256054 ) ) ;
#24448 = AXIS2_PLACEMENT_3D ( 'NONE', #8493, #15635, #1465 ) ;
#24449 = CARTESIAN_POINT ( 'NONE',  ( 18.28362707703099588, -8.107168301167737567, 7.652108011868849147 ) ) ;
#24450 = CARTESIAN_POINT ( 'NONE',  ( 8.499586724479435418, 2.959227181723830036, 21.50000000000000000 ) ) ;
#24451 = EDGE_LOOP ( 'NONE', ( #13751, #25164, #15935, #4962 ) ) ;
#24452 = CARTESIAN_POINT ( 'NONE',  ( 23.07500649350761179, -11.56036165373734725, 44.94877300775547013 ) ) ;
#24453 = ORIENTED_EDGE ( 'NONE', *, *, #23056, .F. ) ;
#24454 = CARTESIAN_POINT ( 'NONE',  ( 35.79322151885497760, -4.895449333909911438, 27.50000000000000711 ) ) ;
#24455 = ORIENTED_EDGE ( 'NONE', *, *, #15251, .T. ) ;
#24456 = EDGE_CURVE ( 'NONE', #14124, #11549, #280, .T. ) ;
#24457 = EDGE_CURVE ( 'NONE', #2397, #4512, #3535, .T. ) ;
#24458 = CARTESIAN_POINT ( 'NONE',  ( 39.00445379423575787, 0.06697950101438043813, 32.23359341845904424 ) ) ;
#24459 = CARTESIAN_POINT ( 'NONE',  ( -5.764374838704560133, 16.04809504443725743, 18.37415474056476938 ) ) ;
#24460 = CARTESIAN_POINT ( 'NONE',  ( -13.37849590052435289, 10.56201291103764284, 20.34789198813115263 ) ) ;
#24461 = EDGE_CURVE ( 'NONE', #19951, #16299, #515, .T. ) ;
#24462 = DIRECTION ( 'NONE',  ( 1.000000000000000000, 0.000000000000000000, 0.000000000000000000 ) ) ;
#24463 = CARTESIAN_POINT ( 'NONE',  ( -32.98872764523831336, -22.67896170318111970, 30.80968328952752699 ) ) ;
#24464 = FACE_OUTER_BOUND ( 'NONE', #22294, .T. ) ;
#24465 = CARTESIAN_POINT ( 'NONE',  ( -27.86235613436986114, -14.72519157938688750, 39.24389099736757203 ) ) ;
#24466 = VERTEX_POINT ( 'NONE', #25876 ) ;
#24467 = CARTESIAN_POINT ( 'NONE',  ( 10.39222174957287770, -17.10906616942579817, 6.111214848085761986 ) ) ;
#24468 = CARTESIAN_POINT ( 'NONE',  ( 29.81396013349119301, -22.14051264938663266, 34.49999999999999289 ) ) ;
#24469 = VECTOR ( 'NONE', #18801, 1000.000000000000000 ) ;
#24470 = DIRECTION ( 'NONE',  ( 1.000000000000000000, 0.000000000000000000, 0.000000000000000000 ) ) ;
#24471 = ORIENTED_EDGE ( 'NONE', *, *, #25611, .T. ) ;
#24472 = ORIENTED_EDGE ( 'NONE', *, *, #25952, .F. ) ;
#24473 = CARTESIAN_POINT ( 'NONE',  ( 18.12921809165262843, -8.446683920555059899, 18.47110296274025387 ) ) ;
#24474 = CARTESIAN_POINT ( 'NONE',  ( 10.68464666747177105, -16.90719797777716948, 5.775318986477953942 ) ) ;
#24475 = EDGE_CURVE ( 'NONE', #8092, #18, #4506, .T. ) ;
#24476 = CARTESIAN_POINT ( 'NONE',  ( 8.499586724479435418, 2.959227181723830036, 21.50000000000000000 ) ) ;
#24477 = CARTESIAN_POINT ( 'NONE',  ( 11.65964093050818917, 12.47882650181265163, 6.588756557121052460 ) ) ;
#24478 = DIRECTION ( 'NONE',  ( 0.000000000000000000, 0.000000000000000000, 1.000000000000000000 ) ) ;
#24479 = CARTESIAN_POINT ( 'NONE',  ( -31.29501345865529061, -26.27841684422010360, -6.500000000000000888 ) ) ;
#24480 = ORIENTED_EDGE ( 'NONE', *, *, #18563, .T. ) ;
#24481 = AXIS2_PLACEMENT_3D ( 'NONE', #23034, #15566, #13408 ) ;
#24482 = CARTESIAN_POINT ( 'NONE',  ( -9.815074746724004484, -17.42621888692031717, 18.73377938172347967 ) ) ;
#24483 = LINE ( 'NONE', #5469, #7749 ) ;
#24484 = CARTESIAN_POINT ( 'NONE',  ( 19.76665705046225696, 3.161078882829541747, 5.651989602109218858 ) ) ;
#24485 = VERTEX_POINT ( 'NONE', #5120 ) ;
#24486 = CARTESIAN_POINT ( 'NONE',  ( 15.54774248266353176, 12.60889669900781129, 6.530762810602277924 ) ) ;
#24487 = EDGE_CURVE ( 'NONE', #20113, #11497, #25919, .T. ) ;
#24488 = CARTESIAN_POINT ( 'NONE',  ( 16.05603743463489863, -5.780788835868666986, 7.441806358946449151 ) ) ;
#24489 = EDGE_CURVE ( 'NONE', #20736, #17664, #27107, .T. ) ;
#24490 = FACE_OUTER_BOUND ( 'NONE', #19558, .T. ) ;
#24491 = AXIS2_PLACEMENT_3D ( 'NONE', #6513, #4165, #18525 ) ;
#24492 = CARTESIAN_POINT ( 'NONE',  ( -24.75800239156184546, 7.045788922043114688, 45.01673140503407211 ) ) ;
#24493 = VERTEX_POINT ( 'NONE', #15394 ) ;
#24494 = DIRECTION ( 'NONE',  ( -0.000000000000000000, -0.000000000000000000, -1.000000000000000000 ) ) ;
#24495 = DIRECTION ( 'NONE',  ( 0.000000000000000000, 1.000000000000000000, 0.000000000000000000 ) ) ;
#24496 = CARTESIAN_POINT ( 'NONE',  ( 57.49999999999998579, -50.00000000000000000, 62.49999999999999289 ) ) ;
#24497 = CARTESIAN_POINT ( 'NONE',  ( 2.034297646570668583, 39.45293230050472033, 34.50000000000000000 ) ) ;
#24498 = CARTESIAN_POINT ( 'NONE',  ( -17.94248964168179938, 34.33858135081683827, 34.80090346875804386 ) ) ;
#24499 = CARTESIAN_POINT ( 'NONE',  ( 9.186411229153639724, -14.33460949872161549, 19.96783386855779341 ) ) ;
#24500 = CARTESIAN_POINT ( 'NONE',  ( -17.84153987719600920, 14.83584055149731284, 1.500000000000000000 ) ) ;
#24501 = ORIENTED_EDGE ( 'NONE', *, *, #26177, .T. ) ;
#24502 = CARTESIAN_POINT ( 'NONE',  ( -26.81368379037235172, -6.366017791192966513, 47.44099319977362939 ) ) ;
#24503 = FACE_OUTER_BOUND ( 'NONE', #21235, .T. ) ;
#24504 = DIRECTION ( 'NONE',  ( 0.000000000000000000, 0.000000000000000000, 1.000000000000000000 ) ) ;
#24505 = ORIENTED_EDGE ( 'NONE', *, *, #4666, .F. ) ;
#24506 = CARTESIAN_POINT ( 'NONE',  ( 32.75827721992816777, -23.06400683538976892, 17.99609636942189894 ) ) ;
#24507 = DIRECTION ( 'NONE',  ( 1.000000000000000000, 2.396195514597832977E-15, 0.000000000000000000 ) ) ;
#24508 = CARTESIAN_POINT ( 'NONE',  ( -15.01515151829605976, 13.21212483861245346, 18.47110296274025742 ) ) ;
#24509 = CARTESIAN_POINT ( 'NONE',  ( 8.757878075398934925, -7.394122547431893011, 1.500000000000000000 ) ) ;
#24510 = AXIS2_PLACEMENT_3D ( 'NONE', #6316, #15986, #3681 ) ;
#24511 = CARTESIAN_POINT ( 'NONE',  ( -39.83602371821029919, -11.57901747687044924, -19.50000000000000355 ) ) ;
#24512 = DIRECTION ( 'NONE',  ( 0.000000000000000000, 0.000000000000000000, -1.000000000000000000 ) ) ;
#24513 = FACE_OUTER_BOUND ( 'NONE', #30808, .T. ) ;
#24514 = CARTESIAN_POINT ( 'NONE',  ( -64.99999999999998579, 36.86186943028246787, 57.49999999999999289 ) ) ;
#24515 = ORIENTED_EDGE ( 'NONE', *, *, #25007, .F. ) ;
#24516 = DIRECTION ( 'NONE',  ( 0.000000000000000000, 0.000000000000000000, 1.000000000000000000 ) ) ;
#24517 = ORIENTED_EDGE ( 'NONE', *, *, #1623, .T. ) ;
#24518 = CYLINDRICAL_SURFACE ( 'NONE', #736, 0.7500000000000011102 ) ;
#24519 = CARTESIAN_POINT ( 'NONE',  ( 24.03057240117691862, 26.57182937991349903, 1.500000000000000000 ) ) ;
#24520 = VERTEX_POINT ( 'NONE', #5731 ) ;
#24521 = CIRCLE ( 'NONE', #1131, 6.000000000000001776 ) ;
#24522 = VERTEX_POINT ( 'NONE', #29294 ) ;
#24523 = CARTESIAN_POINT ( 'NONE',  ( -10.07574916981069357, -17.27697906656895910, 5.779535427900759359 ) ) ;
#24524 = CIRCLE ( 'NONE', #11092, 3.000000000000002665 ) ;
#24525 = ORIENTED_EDGE ( 'NONE', *, *, #29838, .T. ) ;
#24526 = ADVANCED_FACE ( 'NONE', ( #10721 ), #5587, .F. ) ;
#24527 = ORIENTED_EDGE ( 'NONE', *, *, #2510, .F. ) ;
#24528 = PLANE ( 'NONE',  #23819 ) ;
#24529 = CARTESIAN_POINT ( 'NONE',  ( -6.533353553387044599, 38.84762322035204818, 34.49999999999999289 ) ) ;
#24530 = FACE_OUTER_BOUND ( 'NONE', #13178, .T. ) ;
#24531 = CARTESIAN_POINT ( 'NONE',  ( -37.61339438558123049, 11.23552226342446581, 11.09322008216695821 ) ) ;
#24532 = DIRECTION ( 'NONE',  ( -0.000000000000000000, -0.000000000000000000, 1.000000000000000000 ) ) ;
#24533 = EDGE_LOOP ( 'NONE', ( #30423, #14200, #16804, #20883 ) ) ;
#24534 = CARTESIAN_POINT ( 'NONE',  ( 25.64627119138473432, 23.40052582045089480, -16.50000000000000000 ) ) ;
#24535 = DIRECTION ( 'NONE',  ( 1.000000000000000000, 0.000000000000000000, 4.565061778886335400E-17 ) ) ;
#24536 = CARTESIAN_POINT ( 'NONE',  ( 1.964582201835905151, 2.267248723062786908, 24.50000000000000000 ) ) ;
#24537 = DIRECTION ( 'NONE',  ( 1.000000000000000000, 0.000000000000000000, 0.000000000000000000 ) ) ;
#24538 = ORIENTED_EDGE ( 'NONE', *, *, #23056, .T. ) ;
#24539 = CARTESIAN_POINT ( 'NONE',  ( -9.378051617232568304, -14.20529941771991211, 19.11611934778430921 ) ) ;
#24540 = FACE_OUTER_BOUND ( 'NONE', #28969, .T. ) ;
#24541 = CARTESIAN_POINT ( 'NONE',  ( -6.426383236738485216, 15.81971323177988253, 6.233981582756856987 ) ) ;
#24542 = VECTOR ( 'NONE', #13399, 1000.000000000000000 ) ;
#24543 = CARTESIAN_POINT ( 'NONE',  ( 10.68026781623521693, -13.32599531033824825, 6.447548852708279377 ) ) ;
#24544 = AXIS2_PLACEMENT_3D ( 'NONE', #21439, #4603, #7247 ) ;
#24545 = CARTESIAN_POINT ( 'NONE',  ( -40.89187623478217404, -5.790488632116337797, -19.50000000000000355 ) ) ;
#24546 = CARTESIAN_POINT ( 'NONE',  ( 2.599508007902112006, 14.29059753516471964, -1.500000000000000000 ) ) ;
#24547 = ORIENTED_EDGE ( 'NONE', *, *, #25581, .F. ) ;
#24548 = ORIENTED_EDGE ( 'NONE', *, *, #24261, .F. ) ;
#24549 = CARTESIAN_POINT ( 'NONE',  ( -5.976020107417636673, 19.08630880174946043, 18.34798005863226678 ) ) ;
#24550 = CARTESIAN_POINT ( 'NONE',  ( 2.548218919432729823, -42.41581599557042637, 34.61094837024117510 ) ) ;
#24551 = CARTESIAN_POINT ( 'NONE',  ( 6.631244434206235105, 6.812559277181991391, 21.50000000000000000 ) ) ;
#24552 = ORIENTED_EDGE ( 'NONE', *, *, #27507, .F. ) ;
#24553 = SHAPE_DEFINITION_REPRESENTATION ( #18886, #16871 ) ;
#24554 = CARTESIAN_POINT ( 'NONE',  ( 18.33777834721833599, -8.027392848387998825, 18.34777357837152323 ) ) ;
#24555 =( REPRESENTATION_RELATIONSHIP ('NONE','NONE', #19885, #10307 ) REPRESENTATION_RELATIONSHIP_WITH_TRANSFORMATION ( #22218 )SHAPE_REPRESENTATION_RELATIONSHIP( ) );
#24556 = CARTESIAN_POINT ( 'NONE',  ( -37.99999999999999289, 70.00000000000000000, -40.50000000000000000 ) ) ;
#24557 = ORIENTED_EDGE ( 'NONE', *, *, #19679, .T. ) ;
#24558 = CARTESIAN_POINT ( 'NONE',  ( -7.706848733600993206, -5.524309650260738280, 13.00000000000000178 ) ) ;
#24559 = B_SPLINE_SURFACE_WITH_KNOTS ( 'NONE', 3, 1, ( 
 ( #16739, #17049 ),
 ( #25954, #18945 ),
 ( #9880, #4732 ),
 ( #14562, #23749 ),
 ( #2560, #14234 ),
 ( #205, #26253 ),
 ( #28603, #28758 ),
 ( #21098, #11929 ),
 ( #2401, #61 ),
 ( #28455, #26577 ),
 ( #19398, #7079 ),
 ( #7395, #16906 ),
 ( #12218, #359 ),
 ( #7226, #21719 ),
 ( #4582, #26422 ),
 ( #23593, #28916 ),
 ( #28304, #5202 ),
 ( #19230, #12073 ),
 ( #14705, #24058 ),
 ( #2237, #16586 ),
 ( #21419, #30618 ),
 ( #24211, #2863 ),
 ( #6929, #9574 ),
 ( #4893, #16441 ),
 ( #9265, #21569 ),
 ( #11756, #18784 ),
 ( #14084, #21252 ),
 ( #14412, #30780 ),
 ( #9429, #19856 ),
 ( #13001, #670 ),
 ( #17838, #29530 ) ),
 .UNSPECIFIED., .F., .F., .F.,
 ( 4, 3, 3, 3, 3, 3, 3, 3, 3, 3, 4 ),
 ( 2, 2 ),
 ( 0.000000000000000000, 0.05425176834609614362, 0.1085332949128348518, 0.1623767749169379715, 0.2157504826133058717, 0.2688657508888169789, 0.3218907763505471364, 0.3749548578363334772, 0.4282048033836237666, 0.4818374082110496448, 0.4999999999131651274 ),
 ( 0.000000000000000000, 1.000000000000000000 ),
 .UNSPECIFIED. ) ;
#24560 = DIRECTION ( 'NONE',  ( 0.000000000000000000, 1.000000000000000000, 0.000000000000000000 ) ) ;
#24561 = CARTESIAN_POINT ( 'NONE',  ( 0.000000000000000000, 0.000000000000000000, 21.50000000000000000 ) ) ;
#24562 = CARTESIAN_POINT ( 'NONE',  ( -36.11265399167034218, -10.12638981614433931, 37.50000000003317524 ) ) ;
#24563 = ORIENTED_EDGE ( 'NONE', *, *, #18731, .F. ) ;
#24564 = FACE_OUTER_BOUND ( 'NONE', #4348, .T. ) ;
#24565 = VECTOR ( 'NONE', #13101, 1000.000000000000000 ) ;
#24566 = EDGE_CURVE ( 'NONE', #14545, #13653, #29922, .T. ) ;
#24567 = AXIS2_PLACEMENT_3D ( 'NONE', #24157, #7340, #2806 ) ;
#24568 = CARTESIAN_POINT ( 'NONE',  ( -4.163336342344337027E-14, 1.387778780781445676E-14, 92.49999999999998579 ) ) ;
#24569 = DIRECTION ( 'NONE',  ( 0.000000000000000000, 0.000000000000000000, -1.000000000000000000 ) ) ;
#24570 = ORIENTED_EDGE ( 'NONE', *, *, #16290, .F. ) ;
#24571 = FACE_OUTER_BOUND ( 'NONE', #8108, .T. ) ;
#24572 = CARTESIAN_POINT ( 'NONE',  ( 31.10273980501928293, 15.38400267427140378, 36.05808397467829707 ) ) ;
#24573 = CARTESIAN_POINT ( 'NONE',  ( -49.64645017045302922, 69.99712838247133107, 19.84290309017789866 ) ) ;
#24574 = CARTESIAN_POINT ( 'NONE',  ( -40.35746994301763380, -4.708323662206837845, -16.50000000000000355 ) ) ;
#24575 = LINE ( 'NONE', #14755, #13838 ) ;
#24576 = CARTESIAN_POINT ( 'NONE',  ( 35.29656769949644257, -18.08766611768221466, 17.44407013695211006 ) ) ;
#24577 = CARTESIAN_POINT ( 'NONE',  ( -77.99999999999998579, 42.50000000000000711, 27.50000000000000000 ) ) ;
#24578 = ORIENTED_EDGE ( 'NONE', *, *, #21013, .F. ) ;
#24579 = DIRECTION ( 'NONE',  ( 1.224646799147353207E-16, 1.000000000000000000, -0.000000000000000000 ) ) ;
#24580 = AXIS2_PLACEMENT_3D ( 'NONE', #21031, #4665, #13726 ) ;
#24581 = CARTESIAN_POINT ( 'NONE',  ( 4.690519134554615555, 19.44242338873975484, 5.853797745100186134 ) ) ;
#24582 = ORIENTED_EDGE ( 'NONE', *, *, #3065, .T. ) ;
#24583 = ORIENTED_EDGE ( 'NONE', *, *, #24644, .T. ) ;
#24584 = AXIS2_PLACEMENT_3D ( 'NONE', #19067, #10284, #14810 ) ;
#24585 = CARTESIAN_POINT ( 'NONE',  ( -4.668110441710642711, -19.44758969394387194, 24.50000000000000000 ) ) ;
#24586 = CARTESIAN_POINT ( 'NONE',  ( -19.64177907938615064, 36.71644397333972876, 24.50000000000000000 ) ) ;
#24587 = VECTOR ( 'NONE', #26283, 1000.000000000000000 ) ;
#24588 =( NAMED_UNIT ( * ) SI_UNIT ( $, .STERADIAN. ) SOLID_ANGLE_UNIT ( ) );
#24589 = VERTEX_POINT ( 'NONE', #10103 ) ;
#24590 = CARTESIAN_POINT ( 'NONE',  ( -20.20090942434742587, -32.69829930755841474, 27.50000000000000355 ) ) ;
#24591 = CARTESIAN_POINT ( 'NONE',  ( 14.94527285076313916, 13.31737086058187458, 18.34969686940296185 ) ) ;
#24592 = ADVANCED_FACE ( 'NONE', ( #10572 ), #26644, .T. ) ;
#24593 = ORIENTED_EDGE ( 'NONE', *, *, #19295, .T. ) ;
#24594 = EDGE_CURVE ( 'NONE', #24164, #7313, #1064, .T. ) ;
#24595 = CARTESIAN_POINT ( 'NONE',  ( -19.74495986540963344, 3.294819794740638574, 7.272049892295485485 ) ) ;
#24596 = CARTESIAN_POINT ( 'NONE',  ( 19.74942470869275724, 3.267558643021993614, 20.34789198813115263 ) ) ;
#24597 = EDGE_CURVE ( 'NONE', #19456, #19866, #11685, .T. ) ;
#24598 = FACE_BOUND ( 'NONE', #27563, .T. ) ;
#24599 = EDGE_LOOP ( 'NONE', ( #10300, #30044 ) ) ;
#24600 = LINE ( 'NONE', #29603, #12874 ) ;
#24601 = EDGE_CURVE ( 'NONE', #13769, #4888, #20939, .T. ) ;
#24602 = ORIENTED_EDGE ( 'NONE', *, *, #14950, .T. ) ;
#24603 = ADVANCED_FACE ( 'NONE', ( #24598, #3556, #13078, #22568, #26811, #1221 ), #14780, .T. ) ;
#24604 = CARTESIAN_POINT ( 'NONE',  ( -16.96556290498877573, 1.647560670993253540, 18.34798005863078885 ) ) ;
#24605 = ORIENTED_EDGE ( 'NONE', *, *, #16017, .T. ) ;
#24606 = AXIS2_PLACEMENT_3D ( 'NONE', #1698, #13866, #10921 ) ;
#24607 = CARTESIAN_POINT ( 'NONE',  ( -6.228680293130164358, 19.00574304797303782, 18.37545668562167478 ) ) ;
#24608 = EDGE_CURVE ( 'NONE', #14972, #28030, #5508, .T. ) ;
#24609 = DIRECTION ( 'NONE',  ( 0.000000000000000000, -1.000000000000000000, 0.000000000000000000 ) ) ;
#24610 = CARTESIAN_POINT ( 'NONE',  ( 45.00000000000045475, -4.871505565812501079E-13, 82.49999999999998579 ) ) ;
#24611 = CARTESIAN_POINT ( 'NONE',  ( -18.04365185506137337, -8.627086862512673093, 7.652108011868850035 ) ) ;
#24612 = EDGE_CURVE ( 'NONE', #14253, #2413, #27936, .T. ) ;
#24613 = CARTESIAN_POINT ( 'NONE',  ( -10.23401665697057084, -17.20427178438287541, 18.39992786714538298 ) ) ;
#24614 = ADVANCED_FACE ( 'NONE', ( #24298 ), #12465, .T. ) ;
#24615 = CARTESIAN_POINT ( 'NONE',  ( -38.65487109636899277, 5.678429112161928138, 32.12412996058973391 ) ) ;
#24616 = CARTESIAN_POINT ( 'NONE',  ( -25.10445388623454477, 25.60065097860747585, 1.500000000000000000 ) ) ;
#24617 = PLANE ( 'NONE',  #12867 ) ;
#24618 = ORIENTED_EDGE ( 'NONE', *, *, #18064, .F. ) ;
#24619 = CARTESIAN_POINT ( 'NONE',  ( 9.864935476506833112, -13.90063640520463650, 5.652196082367002106 ) ) ;
#24620 = DIRECTION ( 'NONE',  ( 0.000000000000000000, 0.000000000000000000, -1.000000000000000000 ) ) ;
#24621 = LINE ( 'NONE', #29936, #16073 ) ;
#24622 = ORIENTED_EDGE ( 'NONE', *, *, #3854, .T. ) ;
#24623 = ORIENTED_EDGE ( 'NONE', *, *, #21525, .T. ) ;
#24624 = FACE_OUTER_BOUND ( 'NONE', #23556, .T. ) ;
#24625 = CARTESIAN_POINT ( 'NONE',  ( 10.27641578865090466, -17.15802603149301220, 6.913388067999417963 ) ) ;
#24626 = CARTESIAN_POINT ( 'NONE',  ( -5.973960059363099262, 19.10558826632599860, 7.652108011868850035 ) ) ;
#24627 = ORIENTED_EDGE ( 'NONE', *, *, #29018, .F. ) ;
#24628 = LINE ( 'NONE', #22748, #27595 ) ;
#24629 = DIRECTION ( 'NONE',  ( 1.000000000000000000, 0.000000000000000000, 0.000000000000000000 ) ) ;
#24630 = AXIS2_PLACEMENT_3D ( 'NONE', #16047, #1409, #9037 ) ;
#24631 = EDGE_CURVE ( 'NONE', #19956, #17125, #10998, .T. ) ;
#24632 = CARTESIAN_POINT ( 'NONE',  ( -4.163336342344337027E-14, -1.387778780781445676E-14, 1.500000000000000000 ) ) ;
#24633 = ORIENTED_EDGE ( 'NONE', *, *, #26762, .T. ) ;
#24634 = EDGE_CURVE ( 'NONE', #27497, #10212, #22717, .T. ) ;
#24635 = DIRECTION ( 'NONE',  ( 0.000000000000000000, 0.000000000000000000, -1.000000000000000000 ) ) ;
#24636 = CARTESIAN_POINT ( 'NONE',  ( -10.18506332983503704, 29.04537757311073776, 1.500000000000000000 ) ) ;
#24637 = EDGE_CURVE ( 'NONE', #16462, #7391, #30370, .T. ) ;
#24638 = CARTESIAN_POINT ( 'NONE',  ( 16.87938398529693984, 2.193321724558644714, 6.755862304746362845 ) ) ;
#24639 = B_SPLINE_CURVE_WITH_KNOTS ( 'NONE', 3,
 ( #7423, #10064, #17547, #27065, #10213, #29093, #19723, #29246, #2588, #12105, #28785, #26450, #5080, #14591, #11149, #8191 ),
 .UNSPECIFIED., .F., .F.,
 ( 4, 2, 2, 2, 2, 2, 2, 4 ),
 ( 0.5000000000000000000, 0.6250000000000013323, 0.6875000000000022204, 0.7187500000000025535, 0.7500000000000028866, 0.8125000000000017764, 0.8750000000000008882, 1.000000000000000000 ),
 .UNSPECIFIED. ) ;
#24640 = ORIENTED_EDGE ( 'NONE', *, *, #28308, .F. ) ;
#24641 = CARTESIAN_POINT ( 'NONE',  ( 15.11794152162359062, 13.12142272612526206, 5.701226463332907279 ) ) ;
#24642 = ORIENTED_EDGE ( 'NONE', *, *, #9430, .F. ) ;
#24643 = CARTESIAN_POINT ( 'NONE',  ( 25.48568755041062417, 12.36160011285428872, 24.50000000000000000 ) ) ;
#24644 = EDGE_CURVE ( 'NONE', #8165, #13794, #5016, .T. ) ;
#24645 = CARTESIAN_POINT ( 'NONE',  ( -4.163336342344337027E-14, 1.387778780781445676E-14, 21.50000000000000000 ) ) ;
#24646 = ORIENTED_EDGE ( 'NONE', *, *, #24027, .F. ) ;
#24647 = ADVANCED_FACE ( 'NONE', ( #8852 ), #18375, .F. ) ;
#24648 = FACE_OUTER_BOUND ( 'NONE', #29015, .T. ) ;
#24649 = DIRECTION ( 'NONE',  ( -0.000000000000000000, -0.000000000000000000, -1.000000000000000000 ) ) ;
#24650 = FACE_OUTER_BOUND ( 'NONE', #2861, .T. ) ;
#24651 = CARTESIAN_POINT ( 'NONE',  ( 8.080641794577413606, 38.55540066144438782, 34.49999999999999289 ) ) ;
#24652 = AXIS2_PLACEMENT_3D ( 'NONE', #26093, #14227, #23289 ) ;
#24653 = DIRECTION ( 'NONE',  ( 0.000000000000000000, 0.000000000000000000, -1.000000000000000000 ) ) ;
#24654 = CARTESIAN_POINT ( 'NONE',  ( 10.28124378133233741, -17.17592898829030901, 19.56050940960062690 ) ) ;
#24655 = CARTESIAN_POINT ( 'NONE',  ( 29.81956388892670873, 15.48018185647901745, 41.40175883629448350 ) ) ;
#24656 = ORIENTED_EDGE ( 'NONE', *, *, #7533, .F. ) ;
#24657 = CARTESIAN_POINT ( 'NONE',  ( -26.58938213246210580, -6.321715805855834702, 47.66948656093877190 ) ) ;
#24658 = CARTESIAN_POINT ( 'NONE',  ( -2.552544031601109875, 42.50000000001772094, -1.500000000000000000 ) ) ;
#24659 = CARTESIAN_POINT ( 'NONE',  ( 41.02680411063263932, 65.11861831110995524, 62.46341751033051537 ) ) ;
#24660 = VERTEX_POINT ( 'NONE', #23340 ) ;
#24661 = CARTESIAN_POINT ( 'NONE',  ( 28.29745255120971947, -29.24632815619922610, 11.25607929549365238 ) ) ;
#24662 = CARTESIAN_POINT ( 'NONE',  ( 24.03057240117691862, 26.57182937991349903, -1.500000000000000000 ) ) ;
#24663 = EDGE_CURVE ( 'NONE', #14718, #11152, #17472, .T. ) ;
#24664 = CARTESIAN_POINT ( 'NONE',  ( 12.44591117076090647, 11.64178973132370487, 7.652108011868854476 ) ) ;
#24665 = PRESENTATION_STYLE_ASSIGNMENT (( #3616 ) ) ;
#24666 = EDGE_CURVE ( 'NONE', #19689, #30824, #27468, .T. ) ;
#24667 = DIRECTION ( 'NONE',  ( 1.000000000000000000, 0.000000000000000000, 0.000000000000000000 ) ) ;
#24668 = DIRECTION ( 'NONE',  ( -0.000000000000000000, -0.000000000000000000, 1.000000000000000000 ) ) ;
#24669 = CARTESIAN_POINT ( 'NONE',  ( 10.54846567588233697, 41.02342312940356095, 28.96798071624879611 ) ) ;
#24670 = VERTEX_POINT ( 'NONE', #18520 ) ;
#24671 = CARTESIAN_POINT ( 'NONE',  ( 26.58938213246210580, 6.321715805855839143, 43.42684587381940275 ) ) ;
#24672 = ORIENTED_EDGE ( 'NONE', *, *, #28987, .F. ) ;
#24673 = CARTESIAN_POINT ( 'NONE',  ( 49.99999999999998579, 70.00000000000000000, 52.49999999999999289 ) ) ;
#24674 = DIRECTION ( 'NONE',  ( -0.7416830501633135952, 0.6707505147970024284, 0.000000000000000000 ) ) ;
#24675 = EDGE_LOOP ( 'NONE', ( #2450, #10183, #5050, #23659 ) ) ;
#24676 = CIRCLE ( 'NONE', #4745, 0.7500000000000006661 ) ;
#24677 = ORIENTED_EDGE ( 'NONE', *, *, #4787, .T. ) ;
#24678 = CYLINDRICAL_SURFACE ( 'NONE', #18428, 28.20443790117963800 ) ;
#24679 = ORIENTED_EDGE ( 'NONE', *, *, #12219, .T. ) ;
#24680 = CARTESIAN_POINT ( 'NONE',  ( 1.073881485057738949, 0.9711784013061123266, 1.500000000000000000 ) ) ;
#24681 = CARTESIAN_POINT ( 'NONE',  ( -4.037311857024811879, 39.31355646053943076, 34.49999999999998579 ) ) ;
#24682 = CARTESIAN_POINT ( 'NONE',  ( -9.056208293496290196, 2.810445847081952664, 1.500000000000001332 ) ) ;
#24683 = CARTESIAN_POINT ( 'NONE',  ( -37.80350513919287891, 10.44985708433032556, 11.63959174695455445 ) ) ;
#24684 = CYLINDRICAL_SURFACE ( 'NONE', #12779, 0.7499999999999988898 ) ;
#24685 = AXIS2_PLACEMENT_3D ( 'NONE', #25480, #4101, #24462 ) ;
#24686 = DIRECTION ( 'NONE',  ( 0.000000000000000000, 0.000000000000000000, -1.000000000000000000 ) ) ;
#24687 = CARTESIAN_POINT ( 'NONE',  ( 2.599508007902112006, -14.29059753516471964, -1.500000000000000000 ) ) ;
#24688 = CARTESIAN_POINT ( 'NONE',  ( 0.9359619706472933620, -17.02419289499718502, 5.661398277488801867 ) ) ;
#24689 = DIRECTION ( 'NONE',  ( -0.000000000000000000, -0.000000000000000000, 1.000000000000000000 ) ) ;
#24690 = ORIENTED_EDGE ( 'NONE', *, *, #14387, .T. ) ;
#24691 = B_SPLINE_CURVE_WITH_KNOTS ( 'NONE', 3,
 ( #7856, #12220, #17050, #361, #19399, #7550 ),
 .UNSPECIFIED., .F., .F.,
 ( 4, 2, 4 ),
 ( 0.003121276445852158229, 0.003498170197137231551, 0.003875063948422304873 ),
 .UNSPECIFIED. ) ;
#24692 = CARTESIAN_POINT ( 'NONE',  ( -11.06207408980607099, -16.68369011021418302, 20.12545155307891065 ) ) ;
#24693 = CARTESIAN_POINT ( 'NONE',  ( -14.81015662609900119, -8.488192507792282626, 7.280727868105637768 ) ) ;
#24694 = CARTESIAN_POINT ( 'NONE',  ( -6.485253725360689891, 18.93805017237212951, 7.500147780736496017 ) ) ;
#24695 = AXIS2_PLACEMENT_3D ( 'NONE', #26292, #19123, #28490 ) ;
#24696 = CARTESIAN_POINT ( 'NONE',  ( 10.38186781339405584, -13.54365823448426553, 7.441806358946449151 ) ) ;
#24697 = CARTESIAN_POINT ( 'NONE',  ( 23.96732207937828463, 33.98584080152456011, -1.500000000000000000 ) ) ;
#24698 = AXIS2_PLACEMENT_3D ( 'NONE', #18091, #29949, #20270 ) ;
#24699 = DIRECTION ( 'NONE',  ( 0.000000000000000000, 0.000000000000000000, 1.000000000000000000 ) ) ;
#24700 = EDGE_LOOP ( 'NONE', ( #23160, #26141, #15242 ) ) ;
#24701 = ORIENTED_EDGE ( 'NONE', *, *, #19859, .T. ) ;
#24702 = PLANE ( 'NONE',  #5560 ) ;
#24703 = ADVANCED_FACE ( 'NONE', ( #18210 ), #28021, .F. ) ;
#24704 = CARTESIAN_POINT ( 'NONE',  ( -40.89187623478217404, 5.790488632116478129, -19.50000000000000355 ) ) ;
#24705 = CARTESIAN_POINT ( 'NONE',  ( 6.084764702337812636, -42.09022401479442976, 28.87506468199332232 ) ) ;
#24706 = CARTESIAN_POINT ( 'NONE',  ( -0.1790877313959190476, -17.02136788083225838, 6.973843882838226094 ) ) ;
#24707 = ORIENTED_EDGE ( 'NONE', *, *, #18336, .T. ) ;
#24708 = DIRECTION ( 'NONE',  ( -0.000000000000000000, -0.000000000000000000, 1.000000000000000000 ) ) ;
#24709 = AXIS2_PLACEMENT_3D ( 'NONE', #6021, #26941, #1193 ) ;
#24710 = CARTESIAN_POINT ( 'NONE',  ( -50.00000000000000000, 70.00000000000000000, -92.50000000000000000 ) ) ;
#24711 = ORIENTED_EDGE ( 'NONE', *, *, #28807, .T. ) ;
#24712 = CARTESIAN_POINT ( 'NONE',  ( 0.000000000000000000, 7.500000000000000000, -1.500000000000000888 ) ) ;
#24713 = DIRECTION ( 'NONE',  ( 5.125319360840571077E-16, -1.000000000000000000, 0.000000000000000000 ) ) ;
#24714 = CARTESIAN_POINT ( 'NONE',  ( -38.68935852364796801, 5.395939196257416803, 35.04663804086064971 ) ) ;
#24715 = EDGE_LOOP ( 'NONE', ( #4605, #796, #25712, #8598, #20360, #17989, #4128, #22226, #17616, #15031, #14955, #6516, #17316, #7190, #27882, #13620, #11879, #6705, #10669, #15741, #15288, #30582, #23967, #18688, #27115, #13236, #23703, #29905, #21672, #18718, #23913, #26714, #17746, #29629, #6393, #11746, #29745, #15737, #22125, #25645, #18485, #6074, #8343, #10018, #13029, #23522, #19306, #1587, #23387, #14152, #27933, #21519, #17898, #25646, #11793, #3927, #13306, #853, #11857, #22673, #21804, #19309, #2147, #21568, #12063, #22396, #30136, #10206, #1011, #3592, #507, #25817, #20300, #10381, #23877, #15897 ) ) ;
#24716 = DIRECTION ( 'NONE',  ( -0.000000000000000000, 0.000000000000000000, 1.000000000000000000 ) ) ;
#24717 = VECTOR ( 'NONE', #10632, 1000.000000000000114 ) ;
#24718 = AXIS2_PLACEMENT_3D ( 'NONE', #17207, #1142, #20164 ) ;
#24719 = DIRECTION ( 'NONE',  ( 1.000000000000000000, 0.000000000000000000, 0.000000000000000000 ) ) ;
#24720 = AXIS2_PLACEMENT_3D ( 'NONE', #23745, #3862, #28302 ) ;
#24721 = CARTESIAN_POINT ( 'NONE',  ( -25.64627119138473432, -23.40052582045089480, -16.50000000000000000 ) ) ;
#24722 = DIRECTION ( 'NONE',  ( -0.000000000000000000, -0.000000000000000000, -1.000000000000000000 ) ) ;
#24723 = ORIENTED_EDGE ( 'NONE', *, *, #42, .F. ) ;
#24724 =( REPRESENTATION_RELATIONSHIP ('NONE','NONE', #19885, #10307 ) REPRESENTATION_RELATIONSHIP_WITH_TRANSFORMATION ( #15186 )SHAPE_REPRESENTATION_RELATIONSHIP( ) );
#24725 = CARTESIAN_POINT ( 'NONE',  ( 38.00000000000000711, 70.00000000000000000, -22.50000000000003553 ) ) ;
#24726 = CARTESIAN_POINT ( 'NONE',  ( 12.99340803228413144, 10.99622480872967500, 19.60617949693493500 ) ) ;
#24727 = CARTESIAN_POINT ( 'NONE',  ( 15.81223572262637589, -6.365019322297389870, 7.652108011868850923 ) ) ;
#24728 = CARTESIAN_POINT ( 'NONE',  ( 2.270234684139676773, -8.795879380940572645, 21.50000000000000000 ) ) ;
#24729 = CIRCLE ( 'NONE', #8800, 9.084132297865673777 ) ;
#24730 = CARTESIAN_POINT ( 'NONE',  ( 9.436481611552752113, 0.9307681286968877421, 1.500000000000001332 ) ) ;
#24731 = FACE_OUTER_BOUND ( 'NONE', #18547, .T. ) ;
#24732 = CARTESIAN_POINT ( 'NONE',  ( -25.47847050916411504, 26.57182937991348481, -1.500000000000001332 ) ) ;
#24733=STYLED_ITEM('',(#30893),#2654);
#24734 = CARTESIAN_POINT ( 'NONE',  ( 0.000000000000000000, 12.18947652193946851, 29.43090101791767665 ) ) ;
#24735 = EDGE_LOOP ( 'NONE', ( #11698, #2968, #25555, #9641 ) ) ;
#24736 = CYLINDRICAL_SURFACE ( 'NONE', #16261, 1.000000000000004441 ) ;
#24737 = CARTESIAN_POINT ( 'NONE',  ( -25.23756106473024730, -11.43858098102957577, -11.49999999999999645 ) ) ;
#24738 = AXIS2_PLACEMENT_3D ( 'NONE', #26390, #5015, #11724 ) ;
#24739 = ORIENTED_EDGE ( 'NONE', *, *, #2706, .T. ) ;
#24740 = ORIENTED_EDGE ( 'NONE', *, *, #8260, .F. ) ;
#24741 = VECTOR ( 'NONE', #20618, 1000.000000000000000 ) ;
#24742 = LINE ( 'NONE', #20380, #29888 ) ;
#24743 = CARTESIAN_POINT ( 'NONE',  ( -1.796820731648991254, 42.46605015914154535, 19.75032532477241176 ) ) ;
#24744 = DIRECTION ( 'NONE',  ( 0.000000000000000000, 1.000000000000000000, 0.000000000000000000 ) ) ;
#24745 = VECTOR ( 'NONE', #16721, 1000.000000000000000 ) ;
#24746 = DIRECTION ( 'NONE',  ( 1.000000000000000000, 0.000000000000000000, 0.000000000000000000 ) ) ;
#24747 = DIRECTION ( 'NONE',  ( -0.000000000000000000, -0.000000000000000000, 1.000000000000000000 ) ) ;
#24748 = EDGE_LOOP ( 'NONE', ( #12839, #10123, #3546, #16281 ) ) ;
#24749 = ORIENTED_EDGE ( 'NONE', *, *, #20483, .T. ) ;
#24750 = CARTESIAN_POINT ( 'NONE',  ( -6.028330626922774549, 10.93629592680536788, 1.500000000000001332 ) ) ;
#24751 = FACE_OUTER_BOUND ( 'NONE', #14422, .T. ) ;
#24752 = AXIS2_PLACEMENT_3D ( 'NONE', #645, #5330, #5795 ) ;
#24753 = DIRECTION ( 'NONE',  ( -0.000000000000000000, -0.000000000000000000, 1.000000000000000000 ) ) ;
#24754 = ORIENTED_EDGE ( 'NONE', *, *, #17361, .T. ) ;
#24755 = DIRECTION ( 'NONE',  ( 1.000000000000000000, 0.000000000000000000, 0.000000000000000000 ) ) ;
#24756 = EDGE_LOOP ( 'NONE', ( #27581, #1257 ) ) ;
#24757 = CARTESIAN_POINT ( 'NONE',  ( 39.87350638640939593, 4.706224724266460768, -11.49999999999999645 ) ) ;
#24758 = AXIS2_PLACEMENT_3D ( 'NONE', #28105, #26059, #6726 ) ;
#24759 = VERTEX_POINT ( 'NONE', #8555 ) ;
#24760 = AXIS2_PLACEMENT_3D ( 'NONE', #6589, #29850, #30442 ) ;
#24761 = SURFACE_STYLE_FILL_AREA ( #1070 ) ;
#24762 = CARTESIAN_POINT ( 'NONE',  ( 42.49999999999998579, 50.00000000000000000, 62.49999999999999289 ) ) ;
#24763 = CARTESIAN_POINT ( 'NONE',  ( 19.57285800138751597, 4.196195780087079719, 6.560937769032974209 ) ) ;
#24764 = DIRECTION ( 'NONE',  ( 0.06975647374412530244, -0.000000000000000000, -0.9975640502598241977 ) ) ;
#24765 = VECTOR ( 'NONE', #26195, 1000.000000000000000 ) ;
#24766 = CARTESIAN_POINT ( 'NONE',  ( -9.702532784345956784, -17.50903092980014719, 19.69140814234746273 ) ) ;
#24767 = ADVANCED_FACE ( 'NONE', ( #23171 ), #28445, .T. ) ;
#24768 = CARTESIAN_POINT ( 'NONE',  ( -30.63683511483046118, 26.33160370704736408, 30.43224823015176383 ) ) ;
#24769 = CARTESIAN_POINT ( 'NONE',  ( -12.33859880789482233, -8.132258305203423632, -16.50000000000000000 ) ) ;
#24770 = FACE_BOUND ( 'NONE', #29983, .T. ) ;
#24771 = ORIENTED_EDGE ( 'NONE', *, *, #30132, .F. ) ;
#24772 = VECTOR ( 'NONE', #18345, 1000.000000000000000 ) ;
#24773 = PRODUCT_DEFINITION ( 'UNKNOWN', '', #13892, #15745 ) ;
#24774 = CARTESIAN_POINT ( 'NONE',  ( 9.002475149809910704, -14.44561766934883984, 6.641371103590088865 ) ) ;
#24775 = CIRCLE ( 'NONE', #5860, 9.084132297865673777 ) ;
#24776 = CARTESIAN_POINT ( 'NONE',  ( -28.46515462367053928, 29.05384490974418199, 10.83298537692093788 ) ) ;
#24777 = FACE_OUTER_BOUND ( 'NONE', #17688, .T. ) ;
#24778 = AXIS2_PLACEMENT_3D ( 'NONE', #11324, #21269, #20821 ) ;
#24779 = EDGE_CURVE ( 'NONE', #27593, #17088, #12080, .T. ) ;
#24780 = ORIENTED_EDGE ( 'NONE', *, *, #25575, .F. ) ;
#24781 = VERTEX_POINT ( 'NONE', #8665 ) ;
#24782 = CARTESIAN_POINT ( 'NONE',  ( 0.000000000000000000, 0.000000000000000000, 21.50000000000000000 ) ) ;
#24783 = CARTESIAN_POINT ( 'NONE',  ( 9.349584168494304848, 12.69858007495367680, 24.50000000000000000 ) ) ;
#24784 = AXIS2_PLACEMENT_3D ( 'NONE', #21685, #19821, #29344 ) ;
#24785 = EDGE_CURVE ( 'NONE', #1968, #19482, #12511, .T. ) ;
#24786 = CARTESIAN_POINT ( 'NONE',  ( -5.222323004038177174, 16.21609733491351690, 7.595116371587256054 ) ) ;
#24787 = VERTEX_POINT ( 'NONE', #15825 ) ;
#24788 = CARTESIAN_POINT ( 'NONE',  ( -37.99999999999999289, 209.2686044187655909, -34.49999999999999289 ) ) ;
#24789 = VECTOR ( 'NONE', #6509, 1000.000000000000000 ) ;
#24790 = CYLINDRICAL_SURFACE ( 'NONE', #29607, 29.99999999999928946 ) ;
#24791 = AXIS2_PLACEMENT_3D ( 'NONE', #18986, #4771, #21770 ) ;
#24792 = CARTESIAN_POINT ( 'NONE',  ( 6.974883619896790954, 5.687793815610376669, 1.500000000000001332 ) ) ;
#24793 = EDGE_LOOP ( 'NONE', ( #29660, #29376, #23850, #2048 ) ) ;
#24794 = DIRECTION ( 'NONE',  ( -0.000000000000000000, -0.000000000000000000, 1.000000000000000000 ) ) ;
#24795 = EDGE_CURVE ( 'NONE', #19078, #28942, #22461, .T. ) ;
#24796 = CARTESIAN_POINT ( 'NONE',  ( 1.073881485057738949, 0.9711784013061123266, -1.500000000000000000 ) ) ;
#24797 = CARTESIAN_POINT ( 'NONE',  ( 16.83479397774492980, 2.565335765644449761, 7.429667576816606278 ) ) ;
#24798 = ORIENTED_EDGE ( 'NONE', *, *, #30525, .T. ) ;
#24799 = ADVANCED_FACE ( 'NONE', ( #24464 ), #7628, .F. ) ;
#24800 = CARTESIAN_POINT ( 'NONE',  ( 0.000000000000000000, 75.00000000000001421, 50.49999999999998579 ) ) ;
#24801 = ORIENTED_EDGE ( 'NONE', *, *, #27256, .F. ) ;
#24802 = AXIS2_PLACEMENT_3D ( 'NONE', #1178, #30024, #1642 ) ;
#24803 = CARTESIAN_POINT ( 'NONE',  ( 25.48568755041062062, -12.36160011285429583, 24.50000000000000000 ) ) ;
#24804 = AXIS2_PLACEMENT_3D ( 'NONE', #29108, #4941, #18989 ) ;
#24805 = CYLINDRICAL_SURFACE ( 'NONE', #21846, 0.7500000000000006661 ) ;
#24806 = AXIS2_PLACEMENT_3D ( 'NONE', #7200, #23565, #28570 ) ;
#24807 = EDGE_LOOP ( 'NONE', ( #20542, #12240, #2424, #17617 ) ) ;
#24808 = CARTESIAN_POINT ( 'NONE',  ( 4.454645749177148062, 19.51581340210660187, 6.131018562779544823 ) ) ;
#24809 = PLANE ( 'NONE',  #21529 ) ;
#24810 = CARTESIAN_POINT ( 'NONE',  ( -39.87350638640939593, 4.706224724266459880, -6.500000000000000888 ) ) ;
#24811 = DIRECTION ( 'NONE',  ( 0.000000000000000000, 0.000000000000000000, 1.000000000000000000 ) ) ;
#24812 = VECTOR ( 'NONE', #19650, 1000.000000000000000 ) ;
#24813 = AXIS2_PLACEMENT_3D ( 'NONE', #16140, #22848, #25348 ) ;
#24814 = DIRECTION ( 'NONE',  ( 0.000000000000000000, 0.000000000000000000, -1.000000000000000000 ) ) ;
#24815 = CARTESIAN_POINT ( 'NONE',  ( -7.392982946727045146, 5.278755796068742789, 21.50000000000000000 ) ) ;
#24816 = CARTESIAN_POINT ( 'NONE',  ( 11.00066062335189621, -16.70338693167702004, 18.34726407865098707 ) ) ;
#24817 = EDGE_CURVE ( 'NONE', #18115, #23298, #25470, .T. ) ;
#24818 = ORIENTED_EDGE ( 'NONE', *, *, #30532, .F. ) ;
#24819 = EDGE_CURVE ( 'NONE', #3543, #8417, #12011, .T. ) ;
#24820 = LINE ( 'NONE', #3458, #22762 ) ;
#24821 = CARTESIAN_POINT ( 'NONE',  ( -13.87349289520723339, 9.945669722324359086, 19.97651184436794125 ) ) ;
#24822 = CARTESIAN_POINT ( 'NONE',  ( 44.60412398304908521, 68.57966167107747424, 61.38406682071050824 ) ) ;
#24823 = EDGE_CURVE ( 'NONE', #16110, #2810, #28849, .T. ) ;
#24824 = DIRECTION ( 'NONE',  ( -0.000000000000000000, 0.000000000000000000, 1.000000000000000000 ) ) ;
#24825 = VERTEX_POINT ( 'NONE', #29311 ) ;
#24826 = CARTESIAN_POINT ( 'NONE',  ( 28.45806911063409927, -29.06066469564322929, 10.87344409778036969 ) ) ;
#24827 = CARTESIAN_POINT ( 'NONE',  ( -65.00000000000000000, -70.00000000000000000, 57.49999999999999289 ) ) ;
#24828 = EDGE_CURVE ( 'NONE', #3530, #28571, #9036, .T. ) ;
#24829 = B_SPLINE_SURFACE_WITH_KNOTS ( 'NONE', 3, 1, ( 
 ( #17290, #16834 ),
 ( #19622, #29309 ),
 ( #26977, #5603 ),
 ( #26349, #14641 ),
 ( #24613, #9973 ),
 ( #3246, #23986 ),
 ( #9656, #21495 ),
 ( #136, #12154 ),
 ( #21653, #287 ),
 ( #9812, #456 ),
 ( #19325, #28846 ),
 ( #24143, #7481 ),
 ( #14791, #19477 ),
 ( #16977, #28991 ),
 ( #7625, #2960 ),
 ( #26654, #30072 ),
 ( #11049, #17754 ),
 ( #5746, #15565 ),
 ( #24766, #15888 ),
 ( #3882, #20098 ),
 ( #27274, #917 ),
 ( #29929, #6213 ),
 ( #1539, #5906 ),
 ( #15717, #15406 ),
 ( #25083, #24930 ),
 ( #25235, #8099 ),
 ( #15237, #8710 ),
 ( #3727, #17923 ),
 ( #22731, #13089 ),
 ( #3412, #27436 ),
 ( #20550, #10584 ) ),
 .UNSPECIFIED., .F., .F., .F.,
 ( 4, 3, 3, 3, 3, 3, 3, 3, 3, 3, 4 ),
 ( 2, 2 ),
 ( 0.4999999998345688312, 0.5360336730431939367, 0.5907651151589012883, 0.6456034593241830599, 0.6998270958050434309, 0.7529536536315937223, 0.8052385063053260073, 0.8575343587103997356, 0.9106564858195042023, 0.9648414833209685293, 1.000000006602610236 ),
 ( 0.000000000000000000, 1.000000000000000000 ),
 .UNSPECIFIED. ) ;
#24830 = DIRECTION ( 'NONE',  ( 0.000000000000000000, 0.000000000000000000, 1.000000000000000000 ) ) ;
#24831 = DIRECTION ( 'NONE',  ( 1.000000000000000000, 0.000000000000000000, -0.000000000000000000 ) ) ;
#24832 = AXIS2_PLACEMENT_3D ( 'NONE', #2869, #12393, #21893 ) ;
#24833 = CARTESIAN_POINT ( 'NONE',  ( 0.000000000000000000, 0.000000000000000000, 1.500000000000000000 ) ) ;
#24834 = AXIS2_PLACEMENT_3D ( 'NONE', #25048, #6328, #27702 ) ;
#24835 = EDGE_CURVE ( 'NONE', #10944, #4071, #553, .T. ) ;
#24836 = DIRECTION ( 'NONE',  ( -0.000000000000000000, -0.000000000000000000, 1.000000000000000000 ) ) ;
#24837 = CARTESIAN_POINT ( 'NONE',  ( 14.93532791487696976, 34.40258920739002235, 37.50000000003241496 ) ) ;
#24838 = EDGE_CURVE ( 'NONE', #13692, #13938, #3108, .T. ) ;
#24839 = EDGE_LOOP ( 'NONE', ( #27467, #29329, #3630, #19417, #10492, #23678 ) ) ;
#24840 = DIRECTION ( 'NONE',  ( 1.000000000000000000, 0.000000000000000000, 0.000000000000000000 ) ) ;
#24841 = CARTESIAN_POINT ( 'NONE',  ( 127.5000000000000000, 0.000000000000000000, 0.000000000000000000 ) ) ;
#24842 = CARTESIAN_POINT ( 'NONE',  ( -4.776122516674677878E-15, -42.50000000000000000, 1.500000000000000000 ) ) ;
#24843 = EDGE_LOOP ( 'NONE', ( #6727, #19715 ) ) ;
#24844 = EDGE_CURVE ( 'NONE', #27621, #24302, #16984, .T. ) ;
#24845 = ORIENTED_EDGE ( 'NONE', *, *, #28978, .F. ) ;
#24846 = DIRECTION ( 'NONE',  ( 1.000000000000000000, 0.000000000000000000, 0.000000000000000000 ) ) ;
#24847 = CARTESIAN_POINT ( 'NONE',  ( -8.752572334588105463, 2.431858781452820306, 13.22130136205108819 ) ) ;
#24848 = ORIENTED_EDGE ( 'NONE', *, *, #17374, .F. ) ;
#24849 = LINE ( 'NONE', #20160, #14854 ) ;
#24850 = EDGE_LOOP ( 'NONE', ( #15658, #20917 ) ) ;
#24851 = CARTESIAN_POINT ( 'NONE',  ( 3.914987921652262948, 49.85603305452615075, -69.51408439781332049 ) ) ;
#24852 = CARTESIAN_POINT ( 'NONE',  ( 25.48568755041062062, -12.36160011285429583, 1.500000000000000000 ) ) ;
#24853 = DIRECTION ( 'NONE',  ( -0.000000000000000000, -0.000000000000000000, 1.000000000000000000 ) ) ;
#24854 = DIRECTION ( 'NONE',  ( 1.000000000000000000, 0.000000000000000000, 0.000000000000000000 ) ) ;
#24855 = AXIS2_PLACEMENT_3D ( 'NONE', #17069, #2731, #380 ) ;
#24856 = VECTOR ( 'NONE', #1124, 1000.000000000000000 ) ;
#24857 = LINE ( 'NONE', #27046, #18391 ) ;
#24858 = DIRECTION ( 'NONE',  ( 0.000000000000000000, 0.000000000000000000, 1.000000000000000000 ) ) ;
#24859 = CARTESIAN_POINT ( 'NONE',  ( 12.25849595087226085, 11.84990609407550721, 20.33971507717571114 ) ) ;
#24860 = CARTESIAN_POINT ( 'NONE',  ( 20.71335220384823117, -27.86167394782616213, -16.50000000000000000 ) ) ;
#24861 = EDGE_CURVE ( 'NONE', #17088, #8561, #10435, .T. ) ;
#24862 = ORIENTED_EDGE ( 'NONE', *, *, #8848, .T. ) ;
#24863 = EDGE_CURVE ( 'NONE', #9060, #29096, #28993, .T. ) ;
#24864 = CIRCLE ( 'NONE', #10911, 0.7500000000000006661 ) ;
#24865 = CARTESIAN_POINT ( 'NONE',  ( -8.925879454855031980, -14.50801274514188322, 20.25336174263950184 ) ) ;
#24866 = CARTESIAN_POINT ( 'NONE',  ( -17.73902742151046752, -9.275718677609276597, 7.366751648393900176 ) ) ;
#24867 = EDGE_CURVE ( 'NONE', #26243, #22916, #26499, .T. ) ;
#24868 = CARTESIAN_POINT ( 'NONE',  ( -5.058868514924372839, 16.26385723641531555, 7.526951045817046548 ) ) ;
#24869 = CARTESIAN_POINT ( 'NONE',  ( 10.31307689846358677, -13.59231953480260024, 5.810767894563978686 ) ) ;
#24870 = CARTESIAN_POINT ( 'NONE',  ( -39.83602371821029919, -11.57901747687044924, -19.50000000000000355 ) ) ;
#24871 = AXIS2_PLACEMENT_3D ( 'NONE', #2068, #16567, #11589 ) ;
#24872 = CARTESIAN_POINT ( 'NONE',  ( 3.196529495465388226, 8.413215745755008967, -3.621320343559650379 ) ) ;
#24873 = ORIENTED_EDGE ( 'NONE', *, *, #16994, .F. ) ;
#24874 = ORIENTED_EDGE ( 'NONE', *, *, #21033, .T. ) ;
#24875 = CARTESIAN_POINT ( 'NONE',  ( -31.57687401261848592, 15.10620312102103036, 35.75338942089705796 ) ) ;
#24876 = CARTESIAN_POINT ( 'NONE',  ( -19.64114023396299302, -37.13592150529018454, -1.500000000000000000 ) ) ;
#24877 = CARTESIAN_POINT ( 'NONE',  ( -12.96684546537104765, 11.03909700805841609, 5.862424720655265098 ) ) ;
#24878 = CARTESIAN_POINT ( 'NONE',  ( 0.7836604620899301210, -17.02735026737548552, 5.652196082368483587 ) ) ;
#24879 = EDGE_LOOP ( 'NONE', ( #5532, #22765, #27189, #16787 ) ) ;
#24880 = CARTESIAN_POINT ( 'NONE',  ( 4.045242219987652987, 16.55840560649981441, 5.652196082368482699 ) ) ;
#24881 = DIRECTION ( 'NONE',  ( 1.000000000000000000, 0.000000000000000000, 0.000000000000000000 ) ) ;
#24882 = EDGE_LOOP ( 'NONE', ( #16214, #23700, #13737, #2707, #7976, #6090 ) ) ;
#24883 = CARTESIAN_POINT ( 'NONE',  ( 9.169883732660084164, -9.268939115642975679, 1.500000000000001332 ) ) ;
#24884 = AXIS2_PLACEMENT_3D ( 'NONE', #4223, #15776, #18729 ) ;
#24885 = CARTESIAN_POINT ( 'NONE',  ( 8.419710366748642372, 7.777014463793876509, -1.500000000000000000 ) ) ;
#24886 = CARTESIAN_POINT ( 'NONE',  ( -37.26385291380725562, -4.397137131605170168, 37.49999999999801759 ) ) ;
#24887 = EDGE_LOOP ( 'NONE', ( #5718, #24303, #24954, #26452, #24557 ) ) ;
#24888 = CARTESIAN_POINT ( 'NONE',  ( -4.163336342344337027E-14, 1.387778780781445676E-14, -1.500000000000000000 ) ) ;
#24889 = ADVANCED_FACE ( 'NONE', ( #19624 ), #5286, .F. ) ;
#24890 = EDGE_CURVE ( 'NONE', #16799, #3576, #26826, .T. ) ;
#24891 = AXIS2_PLACEMENT_3D ( 'NONE', #14364, #23874, #5006 ) ;
#24892 = DIRECTION ( 'NONE',  ( 0.6548607339452783282, -0.7557495743542641531, 0.000000000000000000 ) ) ;
#24893 = PLANE ( 'NONE',  #4839 ) ;
#24894 = ORIENTED_EDGE ( 'NONE', *, *, #5961, .F. ) ;
#24895 = CARTESIAN_POINT ( 'NONE',  ( -49.99999999999998579, 209.2686044187655909, -34.49999999999998579 ) ) ;
#24896 = DIRECTION ( 'NONE',  ( 0.000000000000000000, 1.000000000000000000, 1.193512090021232842E-16 ) ) ;
#24897 = DIRECTION ( 'NONE',  ( 1.000000000000000000, 0.000000000000000000, 0.000000000000000000 ) ) ;
#24898 = CARTESIAN_POINT ( 'NONE',  ( -8.884323311075783991, -1.438332125858144295, 1.500000000000001332 ) ) ;
#24899 = CARTESIAN_POINT ( 'NONE',  ( 24.03057240117691862, 26.57182937991349903, -16.50000000000000000 ) ) ;
#24900 = DIRECTION ( 'NONE',  ( 1.000000000000000000, 0.000000000000000000, 0.000000000000000000 ) ) ;
#24901 = ORIENTED_EDGE ( 'NONE', *, *, #16788, .F. ) ;
#24902 = CARTESIAN_POINT ( 'NONE',  ( -7.028330626922778990, 10.93629592680536788, 1.500000000000001332 ) ) ;
#24903 = AXIS2_PLACEMENT_3D ( 'NONE', #30612, #11750, #21244 ) ;
#24904 = CYLINDRICAL_SURFACE ( 'NONE', #4120, 2.061368542273053883 ) ;
#24905 = ORIENTED_EDGE ( 'NONE', *, *, #9045, .F. ) ;
#24906 = EDGE_LOOP ( 'NONE', ( #10579, #6970, #8892, #4760 ) ) ;
#24907 = DIRECTION ( 'NONE',  ( -1.000000000000000000, 0.000000000000000000, 0.000000000000000000 ) ) ;
#24908 = CARTESIAN_POINT ( 'NONE',  ( 10.64374042650304020, -42.96126232887725394, -19.50000000000000355 ) ) ;
#24909 = FACE_OUTER_BOUND ( 'NONE', #1638, .T. ) ;
#24910 = VERTEX_POINT ( 'NONE', #21817 ) ;
#24911 = AXIS2_PLACEMENT_3D ( 'NONE', #23614, #11778, #4148 ) ;
#24912 = DIRECTION ( 'NONE',  ( 0.000000000000000000, 0.000000000000000000, 1.000000000000000000 ) ) ;
#24913 = CARTESIAN_POINT ( 'NONE',  ( -4.608906612435655248, -7.730328572437724866, -3.621320343559650379 ) ) ;
#24914 = VERTEX_POINT ( 'NONE', #24616 ) ;
#24915 = CARTESIAN_POINT ( 'NONE',  ( -16.92011235424303806, 1.986018190673853434, 7.595116371587256054 ) ) ;
#24916 = CARTESIAN_POINT ( 'NONE',  ( 18.12802117124498835, -8.449244086891155803, 7.526993102356316356 ) ) ;
#24917 = LINE ( 'NONE', #23170, #4846 ) ;
#24918 = DIRECTION ( 'NONE',  ( 1.000000000000000000, 0.000000000000000000, 0.000000000000000000 ) ) ;
#24919 = ORIENTED_EDGE ( 'NONE', *, *, #238, .T. ) ;
#24920 = APPLICATION_CONTEXT ( 'automotive_design' ) ;
#24921 = DIRECTION ( 'NONE',  ( 1.000000000000000000, 0.000000000000000000, 0.000000000000000000 ) ) ;
#24922 = EDGE_LOOP ( 'NONE', ( #10963, #14461 ) ) ;
#24923 = AXIS2_PLACEMENT_3D ( 'NONE', #11566, #27806, #21055 ) ;
#24924 = CARTESIAN_POINT ( 'NONE',  ( 6.364020599487795415, -6.482337650448428690, -1.500000000000002442 ) ) ;
#24925 = ORIENTED_EDGE ( 'NONE', *, *, #2199, .F. ) ;
#24926 = CARTESIAN_POINT ( 'NONE',  ( 49.99999999999998579, -50.00000000000000000, 12.49999999999999112 ) ) ;
#24927 = CARTESIAN_POINT ( 'NONE',  ( 22.11486391166659615, -35.01327975322180919, 29.53756365415747354 ) ) ;
#24928 = CARTESIAN_POINT ( 'NONE',  ( 16.71770988170262129, 3.349230485916621092, 5.661398277488801867 ) ) ;
#24929 = DIRECTION ( 'NONE',  ( 0.000000000000000000, -0.000000000000000000, -1.000000000000000000 ) ) ;
#24930 = CARTESIAN_POINT ( 'NONE',  ( -8.089106849613330041, -15.02215080929124369, 20.19593175699879595 ) ) ;
#24931 = DIRECTION ( 'NONE',  ( -1.000000000000000000, 0.000000000000000000, 0.000000000000000000 ) ) ;
#24932 = CARTESIAN_POINT ( 'NONE',  ( -9.390093949357552816, -14.19700018541241882, 6.782064869129510676 ) ) ;
#24933 = FACE_BOUND ( 'NONE', #24278, .T. ) ;
#24934 = ORIENTED_EDGE ( 'NONE', *, *, #8534, .T. ) ;
#24935 = CARTESIAN_POINT ( 'NONE',  ( 49.99999999999998579, 50.00000000000000000, 97.07879600563551037 ) ) ;
#24936 = CARTESIAN_POINT ( 'NONE',  ( 10.23384659304339017, -13.64843352988229519, 18.44527579819791185 ) ) ;
#24937 = CARTESIAN_POINT ( 'NONE',  ( -3.858906612435654804, -7.730328572437724866, 21.50000000000000000 ) ) ;
#24938 = ORIENTED_EDGE ( 'NONE', *, *, #10523, .F. ) ;
#24939 = VERTEX_POINT ( 'NONE', #458 ) ;
#24940 = CARTESIAN_POINT ( 'NONE',  ( 0.000000000000000000, 0.000000000000000000, 0.000000000000000000 ) ) ;
#24941 = CARTESIAN_POINT ( 'NONE',  ( 4.510281037539698445E-13, -4.926614671774132148E-13, 77.49999999999998579 ) ) ;
#24942 = CARTESIAN_POINT ( 'NONE',  ( -5.225937649208977298, 16.21530267322276941, 5.701226463332907279 ) ) ;
#24943 = ORIENTED_EDGE ( 'NONE', *, *, #14353, .T. ) ;
#24944 = CARTESIAN_POINT ( 'NONE',  ( -70.00000000000000000, 50.00000000000000000, 59.49999999999999289 ) ) ;
#24945 = AXIS2_PLACEMENT_3D ( 'NONE', #22878, #1673, #11038 ) ;
#24946 = DIRECTION ( 'NONE',  ( 0.000000000000000000, 0.000000000000000000, -1.000000000000000000 ) ) ;
#24947 = FACE_OUTER_BOUND ( 'NONE', #13118, .T. ) ;
#24948 = VERTEX_POINT ( 'NONE', #21969 ) ;
#24949 = DIRECTION ( 'NONE',  ( 0.000000000000000000, 1.000000000000000000, 0.000000000000000000 ) ) ;
#24950 = CARTESIAN_POINT ( 'NONE',  ( 14.34755844633281363, 13.95901041572539292, 6.041646659195333058 ) ) ;
#24951 = CARTESIAN_POINT ( 'NONE',  ( 19.86222817340373226, 2.491431357970654403, 5.940635272151477686 ) ) ;
#24952 = VERTEX_POINT ( 'NONE', #599 ) ;
#24953 = DIRECTION ( 'NONE',  ( 0.000000000000000000, -1.000000000000000000, 0.000000000000000000 ) ) ;
#24954 = ORIENTED_EDGE ( 'NONE', *, *, #4701, .T. ) ;
#24955 = DIRECTION ( 'NONE',  ( 1.000000000000000000, 0.000000000000000000, 0.000000000000000000 ) ) ;
#24956 = FACE_OUTER_BOUND ( 'NONE', #17906, .T. ) ;
#24957 = B_SPLINE_CURVE_WITH_KNOTS ( 'NONE', 3,
 ( #25078, #13086, #22575, #1229 ),
 .UNSPECIFIED., .F., .F.,
 ( 4, 4 ),
 ( 3.022186913382060468E-07, 0.007932103869840195776 ),
 .UNSPECIFIED. ) ;
#24958 = EDGE_LOOP ( 'NONE', ( #5343, #218, #29881, #23008 ) ) ;
#24959 = EDGE_LOOP ( 'NONE', ( #7286, #22417, #1277, #26029, #1462, #6201, #13718, #17681, #15352, #21566, #15512, #18161, #15919, #4329, #28487, #21927, #29052, #2668, #23813, #25721, #29131, #4147, #23798, #22217, #6387, #28022 ) ) ;
#24960 = B_SPLINE_CURVE_WITH_KNOTS ( 'NONE', 3,
 ( #22860, #3540, #13059, #22549, #25050, #17574, #1201, #6027, #6182, #18041, #1511, #3694, #13208, #27556 ),
 .UNSPECIFIED., .F., .F.,
 ( 4, 2, 2, 2, 2, 2, 4 ),
 ( 2.980251112064282051E-07, 0.0007442722521831252177, 0.001488246479255043997, 0.001860233592791008320, 0.002232220706326972642, 0.002604207819862936965, 0.002976194933398901288 ),
 .UNSPECIFIED. ) ;
#24961 = CARTESIAN_POINT ( 'NONE',  ( 3.978203543573296308, 16.57681993851655733, 7.652108011868850035 ) ) ;
#24962 = ADVANCED_FACE ( 'NONE', ( #10115 ), #12512, .F. ) ;
#24963 = CARTESIAN_POINT ( 'NONE',  ( -20.71335220384823117, 27.86167394782616213, -6.500000000000000888 ) ) ;
#24964 = CARTESIAN_POINT ( 'NONE',  ( -40.05104235265675783, 2.353288714454549790, -6.500000000000000888 ) ) ;
#24965 = AXIS2_PLACEMENT_3D ( 'NONE', #563, #2921, #17103 ) ;
#24966 = CARTESIAN_POINT ( 'NONE',  ( 0.000000000000000000, 39.50000000000000000, 27.50000000000000355 ) ) ;
#24967 = CARTESIAN_POINT ( 'NONE',  ( -4.163336342344337027E-14, 1.387778780781445676E-14, 24.50000000000000000 ) ) ;
#24968 = VERTEX_POINT ( 'NONE', #22274 ) ;
#24969 = DIRECTION ( 'NONE',  ( -0.000000000000000000, -0.000000000000000000, 1.000000000000000000 ) ) ;
#24970 = CARTESIAN_POINT ( 'NONE',  ( 15.63062718528785489, -6.770321384568316780, 7.557577766377196582 ) ) ;
#24971 = CARTESIAN_POINT ( 'NONE',  ( -10.11202017158466759, 41.14070756921185534, -1.500000000000000000 ) ) ;
#24972 = CARTESIAN_POINT ( 'NONE',  ( 45.56537712369228643, 69.19660825136207905, 60.81054171467580716 ) ) ;
#24973 = EDGE_LOOP ( 'NONE', ( #15197, #17094, #22100, #29239 ) ) ;
#24974 = ORIENTED_EDGE ( 'NONE', *, *, #1965, .F. ) ;
#24975 = CARTESIAN_POINT ( 'NONE',  ( -4.163336342344337027E-14, 1.387778780781445676E-14, 1.500000000000000000 ) ) ;
#24976 = DIRECTION ( 'NONE',  ( 0.000000000000000000, 0.000000000000000000, 1.000000000000000000 ) ) ;
#24977 = CARTESIAN_POINT ( 'NONE',  ( 12.53055695656565582, 11.54555247029871268, 5.676815824193228721 ) ) ;
#24978 = DIRECTION ( 'NONE',  ( 1.000000000000000000, 0.000000000000000000, 0.000000000000000000 ) ) ;
#24979 = CARTESIAN_POINT ( 'NONE',  ( -6.187077094091591789, 11.47693674426096955, 24.50000000000000000 ) ) ;
#24980 = CARTESIAN_POINT ( 'NONE',  ( -8.999114229549592281, 0.1262659238205133538, -3.621320343559650379 ) ) ;
#24981 = CARTESIAN_POINT ( 'NONE',  ( 16.74328841314637017, 3.194145055459935545, 7.652108011868850923 ) ) ;
#24982 = ORIENTED_EDGE ( 'NONE', *, *, #8795, .F. ) ;
#24983 = ADVANCED_FACE ( 'NONE', ( #17608 ), #290, .F. ) ;
#24984 = CIRCLE ( 'NONE', #25489, 3.000000000000002665 ) ;
#24985 = CARTESIAN_POINT ( 'NONE',  ( 1.000000000000008438, 13.00000000000001421, 43.10779406592839536 ) ) ;
#24986 = CARTESIAN_POINT ( 'NONE',  ( 6.630478080506912342, 6.778663211761485563, 21.50000000000000000 ) ) ;
#24987 = CYLINDRICAL_SURFACE ( 'NONE', #8990, 1.999999999999998224 ) ;
#24988 = VERTEX_POINT ( 'NONE', #22432 ) ;
#24989 = EDGE_CURVE ( 'NONE', #6567, #3146, #7604, .T. ) ;
#24990 = ORIENTED_EDGE ( 'NONE', *, *, #192, .F. ) ;
#24991 = EDGE_CURVE ( 'NONE', #23872, #11382, #4041, .T. ) ;
#24992 = CARTESIAN_POINT ( 'NONE',  ( -4.163336342344337027E-14, -1.387778780781445676E-14, 1.500000000000000000 ) ) ;
#24993 = CARTESIAN_POINT ( 'NONE',  ( -19.92837724392306242, 1.693712106646816151, 19.96797677718663522 ) ) ;
#24994 = VERTEX_POINT ( 'NONE', #20699 ) ;
#24995 = CARTESIAN_POINT ( 'NONE',  ( 3.637110358602580362, -19.99473753024311762, 1.500000000000000000 ) ) ;
#24996 = EDGE_CURVE ( 'NONE', #1715, #1564, #15567, .T. ) ;
#24997 = CARTESIAN_POINT ( 'NONE',  ( -35.78163722268750746, 27.43648963448195133, -11.49999999999999645 ) ) ;
#24998 = EDGE_CURVE ( 'NONE', #27915, #24299, #8531, .T. ) ;
#24999 = CIRCLE ( 'NONE', #3072, 0.7500000000000006661 ) ;
#25000 = DIRECTION ( 'NONE',  ( -0.000000000000000000, -0.000000000000000000, -1.000000000000000000 ) ) ;
#25001 = CARTESIAN_POINT ( 'NONE',  ( -36.99918769783646155, 13.45200937490941584, 15.99911628778121653 ) ) ;
#25002 = LINE ( 'NONE', #10979, #19735 ) ;
#25003 = CARTESIAN_POINT ( 'NONE',  ( -4.163336342344337027E-14, 1.387778780781445676E-14, 67.49999999999997158 ) ) ;
#25004 = CARTESIAN_POINT ( 'NONE',  ( -37.99999999999999289, 209.2686044187655909, -22.50000000000001421 ) ) ;
#25005 = CARTESIAN_POINT ( 'NONE',  ( 12.06031594364850967, 12.06435167025951749, 20.25542030744407640 ) ) ;
#25006 = CYLINDRICAL_SURFACE ( 'NONE', #24062, 0.7499999999999997780 ) ;
#25007 = EDGE_CURVE ( 'NONE', #21157, #7845, #8870, .T. ) ;
#25008 = ORIENTED_EDGE ( 'NONE', *, *, #13221, .T. ) ;
#25009 = EDGE_CURVE ( 'NONE', #30777, #4361, #30226, .T. ) ;
#25010 = CARTESIAN_POINT ( 'NONE',  ( -11.24862133554823274, -16.55851774953665867, 19.87181966307587544 ) ) ;
#25011 = CARTESIAN_POINT ( 'NONE',  ( 7.500000000000000000, 9.184850993605147944E-16, 63.50000000000000000 ) ) ;
#25012 = CARTESIAN_POINT ( 'NONE',  ( -5.964083977939222514, 15.98216206238708637, 7.559636331181775581 ) ) ;
#25013 = ADVANCED_FACE ( 'NONE', ( #20408 ), #15613, .T. ) ;
#25014 = CARTESIAN_POINT ( 'NONE',  ( 9.991354877675743040, -13.81564317159775968, 5.661398277488802755 ) ) ;
#25015 = CARTESIAN_POINT ( 'NONE',  ( 5.374868878254059013, -44.10336124695543703, -19.50000000000000355 ) ) ;
#25016 = CARTESIAN_POINT ( 'NONE',  ( -5.393256883115301825, -14.81828060999315433, 24.50000000000000000 ) ) ;
#25017 = ORIENTED_EDGE ( 'NONE', *, *, #4026, .T. ) ;
#25018 = ORIENTED_EDGE ( 'NONE', *, *, #18101, .F. ) ;
#25019 = DIRECTION ( 'NONE',  ( -0.000000000000000000, 1.000000000000000000, -0.000000000000000000 ) ) ;
#25020 = CARTESIAN_POINT ( 'NONE',  ( -25.19442432475474902, -35.44676296258422354, -19.50000000000000355 ) ) ;
#25021 = CARTESIAN_POINT ( 'NONE',  ( -14.75808792347767984, 13.52460813173914289, 6.211014596808754007 ) ) ;
#25022 = LINE ( 'NONE', #3663, #19562 ) ;
#25023 = ORIENTED_EDGE ( 'NONE', *, *, #12838, .F. ) ;
#25024 = CARTESIAN_POINT ( 'NONE',  ( 19.64114023396890829, 37.13592150528549496, -1.500000000000000000 ) ) ;
#25025 = CARTESIAN_POINT ( 'NONE',  ( -11.13550902248300467, -16.63501148641496030, 7.359006845440219102 ) ) ;
#25026 = EDGE_CURVE ( 'NONE', #3597, #16680, #16343, .T. ) ;
#25027 = ORIENTED_EDGE ( 'NONE', *, *, #20075, .T. ) ;
#25028 = EDGE_CURVE ( 'NONE', #25685, #22720, #27261, .T. ) ;
#25029 = DIRECTION ( 'NONE',  ( -0.000000000000000000, -0.000000000000000000, 1.000000000000000000 ) ) ;
#25030 = ADVANCED_FACE ( 'NONE', ( #26010 ), #13999, .F. ) ;
#25031 = CARTESIAN_POINT ( 'NONE',  ( -22.86367660746757480, -34.44063100554308932, 34.50785639329988186 ) ) ;
#25032 = ORIENTED_EDGE ( 'NONE', *, *, #7675, .T. ) ;
#25033 = CARTESIAN_POINT ( 'NONE',  ( 9.454746441592959627, -0.7220001660362816986, 13.00000000000000178 ) ) ;
#25034 = EDGE_CURVE ( 'NONE', #1255, #24968, #21148, .T. ) ;
#25035 = CARTESIAN_POINT ( 'NONE',  ( 1.964582201835851638, -2.267248723062833538, 24.50000000000000000 ) ) ;
#25036 = CARTESIAN_POINT ( 'NONE',  ( -19.82706496683077191, 2.627678016133617955, 20.34789198813115618 ) ) ;
#25037 = ORIENTED_EDGE ( 'NONE', *, *, #4625, .T. ) ;
#25038 = DIRECTION ( 'NONE',  ( 1.000000000000000000, 0.000000000000000000, 0.000000000000000000 ) ) ;
#25039 = CIRCLE ( 'NONE', #11590, 9.084132297865673777 ) ;
#25040 = CIRCLE ( 'NONE', #14637, 0.7500000000000006661 ) ;
#25041 = DIRECTION ( 'NONE',  ( 1.000000000000000000, 0.000000000000000000, 0.000000000000000000 ) ) ;
#25042 = CARTESIAN_POINT ( 'NONE',  ( 49.99999999999998579, -50.00000000000000000, 52.07879600563550326 ) ) ;
#25043 = EDGE_CURVE ( 'NONE', #21089, #6958, #30385, .T. ) ;
#25044 = CARTESIAN_POINT ( 'NONE',  ( -50.00000000000001421, 70.00000000000001421, 21.82070599434954161 ) ) ;
#25045 = CARTESIAN_POINT ( 'NONE',  ( -40.57621058660762259, -1.187786509009159941, -16.50000000000000000 ) ) ;
#25046 = FACE_OUTER_BOUND ( 'NONE', #8768, .T. ) ;
#25047 = LINE ( 'NONE', #25193, #14493 ) ;
#25048 = CARTESIAN_POINT ( 'NONE',  ( -2.703030265324078307, -12.75514121382991384, 1.500000000000001332 ) ) ;
#25049 = FACE_BOUND ( 'NONE', #3814, .T. ) ;
#25050 = CARTESIAN_POINT ( 'NONE',  ( 33.03549465208793379, -8.974030344605372633, 40.76751417242802944 ) ) ;
#25051 = CARTESIAN_POINT ( 'NONE',  ( -9.824744466605366711, -8.513189541288717521, 1.500000000000001332 ) ) ;
#25052 = ORIENTED_EDGE ( 'NONE', *, *, #30696, .T. ) ;
#25053 = ORIENTED_EDGE ( 'NONE', *, *, #3805, .F. ) ;
#25054 = DIRECTION ( 'NONE',  ( 1.000000000000000000, 0.000000000000000000, 0.000000000000000000 ) ) ;
#25055 = DIRECTION ( 'NONE',  ( 0.000000000000000000, 0.000000000000000000, 1.000000000000000000 ) ) ;
#25056 = EDGE_CURVE ( 'NONE', #4949, #6035, #19485, .T. ) ;
#25057 = CARTESIAN_POINT ( 'NONE',  ( 0.8038475772933620922, 5.196152422706624030, 9.000000000000001776 ) ) ;
#25058 = ORIENTED_EDGE ( 'NONE', *, *, #4641, .F. ) ;
#25059 = EDGE_CURVE ( 'NONE', #17587, #3597, #5600, .T. ) ;
#25060 = DIRECTION ( 'NONE',  ( -1.000000000000000000, 0.000000000000000000, 0.000000000000000000 ) ) ;
#25061 = CARTESIAN_POINT ( 'NONE',  ( 9.864937699929956949, -13.90063973435163724, 18.34798005863078885 ) ) ;
#25062 = CIRCLE ( 'NONE', #26060, 3.559164065751841743 ) ;
#25063 = VERTEX_POINT ( 'NONE', #26469 ) ;
#25064 = AXIS2_PLACEMENT_3D ( 'NONE', #1479, #20490, #1157 ) ;
#25065 = FACE_OUTER_BOUND ( 'NONE', #5379, .T. ) ;
#25066 = CARTESIAN_POINT ( 'NONE',  ( 7.500000000000000000, -5.196152422706650675, 9.000000000000001776 ) ) ;
#25067 = CARTESIAN_POINT ( 'NONE',  ( 15.28831480992544911, 12.89481865072260547, 7.454139397117724997 ) ) ;
#25068 = DIRECTION ( 'NONE',  ( -0.000000000000000000, -0.000000000000000000, -1.000000000000000000 ) ) ;
#25069 =( BOUNDED_CURVE ( )  B_SPLINE_CURVE ( 3, ( #24105, #14274, #12115, #14449 ),
 .UNSPECIFIED., .F., .T. ) 
 B_SPLINE_CURVE_WITH_KNOTS ( ( 4, 4 ),
 ( 0.000000000000000000, 3.141592653589793116 ),
 .UNSPECIFIED. ) 
 CURVE ( )  GEOMETRIC_REPRESENTATION_ITEM ( )  RATIONAL_B_SPLINE_CURVE ( ( 1.000000000000000000, 0.3333333333333333703, 0.3333333333333333703, 1.000000000000000000 ) ) 
 REPRESENTATION_ITEM ( '' )  );
#25070 = ORIENTED_EDGE ( 'NONE', *, *, #12082, .F. ) ;
#25071 = CARTESIAN_POINT ( 'NONE',  ( 0.6210184355499435149, -9.062880100047300047, -1.500000000000002887 ) ) ;
#25073 = ORIENTED_EDGE ( 'NONE', *, *, #7930, .F. ) ;
#25072 = VECTOR ( 'NONE', #11918, 1000.000000000000000 ) ;
#25074 = DIRECTION ( 'NONE',  ( 0.3598999890241650346, 0.9329908884337541064, 0.000000000000000000 ) ) ;
#25075 = CARTESIAN_POINT ( 'NONE',  ( 4.622016212553096359, -12.19167610014704906, 1.500000000000001332 ) ) ;
#25076 = EDGE_LOOP ( 'NONE', ( #30317, #4410, #1553, #2812, #23248, #21671 ) ) ;
#25077 = CARTESIAN_POINT ( 'NONE',  ( -5.976020107417636673, 19.08630880174946043, 18.34798005863226678 ) ) ;
#25078 = CARTESIAN_POINT ( 'NONE',  ( -29.61203839202723032, 15.40012917324033381, 37.38016955275591613 ) ) ;
#25079 = B_SPLINE_SURFACE_WITH_KNOTS ( 'NONE', 3, 1, ( 
 ( #23764, #21735 ),
 ( #377, #12556 ),
 ( #21900, #7240 ),
 ( #10052, #5066 ),
 ( #9896, #7094 ),
 ( #9733, #19560 ),
 ( #19411, #9443 ),
 ( #14720, #16601 ),
 ( #26114, #26593 ),
 ( #4907, #19246 ),
 ( #4743, #14575 ),
 ( #7721, #17218 ),
 ( #28928, #26743 ),
 ( #5372, #7562 ),
 ( #14246, #21434 ),
 ( #76, #14425 ),
 ( #28770, #7409 ),
 ( #16917, #26433 ),
 ( #15026, #15645 ),
 ( #22046, #8338 ),
 ( #20020, #10826 ),
 ( #15493, #24693 ),
 ( #24866, #5678 ),
 ( #1149, #27200 ),
 ( #12708, #27516 ),
 ( #8506, #20170 ),
 ( #27051, #27370 ),
 ( #29393, #18008 ),
 ( #841, #19708 ),
 ( #10662, #17852 ),
 ( #8028, #3649 ) ),
 .UNSPECIFIED., .F., .F., .F.,
 ( 4, 3, 3, 3, 3, 3, 3, 3, 3, 3, 4 ),
 ( 2, 2 ),
 ( 0.4999999998345686647, 0.5360336730431942698, 0.5907651151589017324, 0.6456034593241839481, 0.6998270958050443191, 0.7529536536315944995, 0.8052385063053264513, 0.8575343587103996246, 0.9106564858195047574, 0.9648414833209688624, 1.000000006602610014 ),
 ( 0.000000000000000000, 1.000000000000000000 ),
 .UNSPECIFIED. ) ;
#25080 = CARTESIAN_POINT ( 'NONE',  ( 66.99999999999998579, 50.00000000000000000, 62.49999999999999289 ) ) ;
#25081 = DIRECTION ( 'NONE',  ( 1.000000000000000000, 0.000000000000000000, 0.000000000000000000 ) ) ;
#25082 = AXIS2_PLACEMENT_3D ( 'NONE', #13011, #22502, #8026 ) ;
#25083 = CARTESIAN_POINT ( 'NONE',  ( -10.06548534245863280, -17.30301317789300697, 20.19593175699879595 ) ) ;
#25084 = CARTESIAN_POINT ( 'NONE',  ( -17.06581907267799636, 0.6464955982430669046, 19.21769074125272425 ) ) ;
#25085 = CIRCLE ( 'NONE', #24069, 7.500000000000000000 ) ;
#25086 = CARTESIAN_POINT ( 'NONE',  ( -8.550548372801092256, -14.74545326687210611, 7.652108011868850923 ) ) ;
#25087 = CARTESIAN_POINT ( 'NONE',  ( -3.515970705488605130, 17.06554576617236307, 1.500000000000000000 ) ) ;
#25088 = EDGE_LOOP ( 'NONE', ( #7230, #30550 ) ) ;
#25089 = AXIS2_PLACEMENT_3D ( 'NONE', #1123, #8474, #15616 ) ;
#25090 = DIRECTION ( 'NONE',  ( 1.000000000000000000, 0.000000000000000000, 0.000000000000000000 ) ) ;
#25091 = CARTESIAN_POINT ( 'NONE',  ( -6.812559277181930106, 5.881244434206302607, 21.50000000000000000 ) ) ;
#25092 = CARTESIAN_POINT ( 'NONE',  ( 31.18890335284659443, -19.89223002944918761, 27.50000000000001776 ) ) ;
#25093 = EDGE_LOOP ( 'NONE', ( #23634, #6217, #8591, #7249 ) ) ;
#25094 = EDGE_LOOP ( 'NONE', ( #22529, #12765 ) ) ;
#25095 = CARTESIAN_POINT ( 'NONE',  ( -70.00000000000000000, -50.00000000000000000, 59.49999999999999289 ) ) ;
#25096 = CARTESIAN_POINT ( 'NONE',  ( 17.26937953831880534, -14.36006998371588317, 1.500000000000000000 ) ) ;
#25097 = CARTESIAN_POINT ( 'NONE',  ( -4.850186825639134724, 16.32197540402033198, 7.359006845440219102 ) ) ;
#25098 = EDGE_LOOP ( 'NONE', ( #22699, #1981, #8998, #11776 ) ) ;
#25099 = CARTESIAN_POINT ( 'NONE',  ( -42.49999999999998579, 50.00000000000000000, 97.07879600563551037 ) ) ;
#25100 = LINE ( 'NONE', #3743, #5693 ) ;
#25101 = EDGE_CURVE ( 'NONE', #15798, #498, #5102, .T. ) ;
#25102 = CARTESIAN_POINT ( 'NONE',  ( 23.10264100946039534, 11.84391650453516043, 49.03857552305024825 ) ) ;
#25103 = ORIENTED_EDGE ( 'NONE', *, *, #28683, .F. ) ;
#25104 = B_SPLINE_CURVE_WITH_KNOTS ( 'NONE', 3,
 ( #18312, #16421, #2220, #30764, #27830, #13489, #6459, #11287 ),
 .UNSPECIFIED., .F., .F.,
 ( 4, 2, 2, 4 ),
 ( 0.005257893453559881955, 0.006567392922673221702, 0.007876892391786561448, 0.01049589133001324094 ),
 .UNSPECIFIED. ) ;
#25105 = DIRECTION ( 'NONE',  ( -0.000000000000000000, -0.000000000000000000, -1.000000000000000000 ) ) ;
#25106 = CARTESIAN_POINT ( 'NONE',  ( -3.395021109945014270, 30.50000000000000355, 1.500000000000000000 ) ) ;
#25107 = CARTESIAN_POINT ( 'NONE',  ( -1.195154792889458806, -9.406652940105983518, 1.500000000000001332 ) ) ;
#25108 = VERTEX_POINT ( 'NONE', #26629 ) ;
#25109 = LINE ( 'NONE', #24800, #26275 ) ;
#25110 = AXIS2_PLACEMENT_3D ( 'NONE', #30606, #9252, #4569 ) ;
#25111 = ORIENTED_EDGE ( 'NONE', *, *, #25197, .T. ) ;
#25112 = CARTESIAN_POINT ( 'NONE',  ( -16.46198811862381817, -1.356593340923033075, 1.500000000000000000 ) ) ;
#25113 = ORIENTED_EDGE ( 'NONE', *, *, #18891, .F. ) ;
#25114 = ORIENTED_EDGE ( 'NONE', *, *, #24785, .T. ) ;
#25115 = CARTESIAN_POINT ( 'NONE',  ( -25.47847050916410439, -26.57182937991348481, -6.499999999999999112 ) ) ;
#25116 = CARTESIAN_POINT ( 'NONE',  ( 0.000000000000000000, 0.000000000000000000, 21.50000000000000000 ) ) ;
#25117 = DIRECTION ( 'NONE',  ( -0.000000000000000000, -1.000000000000000000, -0.000000000000000000 ) ) ;
#25118 = EDGE_LOOP ( 'NONE', ( #14858, #16062, #20721, #14928 ) ) ;
#25119 = CARTESIAN_POINT ( 'NONE',  ( -15.85884089648730644, -35.55173462727348266, 27.49999999999998934 ) ) ;
#25120 = CARTESIAN_POINT ( 'NONE',  ( 9.801156115998399088, -13.94312737849039330, 18.34969686940296185 ) ) ;
#25121 = PLANE ( 'NONE',  #1424 ) ;
#25122 = VERTEX_POINT ( 'NONE', #418 ) ;
#25123 = CARTESIAN_POINT ( 'NONE',  ( -19.84651427434118176, 2.615565199888951753, 20.34789198813115263 ) ) ;
#25124 = CARTESIAN_POINT ( 'NONE',  ( 15.71976421978571459, -6.574744378264575140, 7.632642797338977658 ) ) ;
#25125 = CARTESIAN_POINT ( 'NONE',  ( -13.88241978398541221, 9.934084310449181388, 6.041646659195333058 ) ) ;
#25126 = CARTESIAN_POINT ( 'NONE',  ( 3.529212228261827011, 16.69261290539733977, 20.19593175699879595 ) ) ;
#25127 = EDGE_LOOP ( 'NONE', ( #23748, #15134, #29038, #19546 ) ) ;
#25128 = ORIENTED_EDGE ( 'NONE', *, *, #19324, .F. ) ;
#25129 = CARTESIAN_POINT ( 'NONE',  ( 32.98805937973592961, -22.67054169308934064, 18.00000000000000000 ) ) ;
#25130 = CYLINDRICAL_SURFACE ( 'NONE', #27075, 2.000000000000001776 ) ;
#25131 = CARTESIAN_POINT ( 'NONE',  ( -4.661329110590011204, 16.37253524622244427, 19.77662771831109367 ) ) ;
#25132 = DIRECTION ( 'NONE',  ( -0.8910248307962438385, 0.4539545692076743522, 0.000000000000000000 ) ) ;
#25133 = CARTESIAN_POINT ( 'NONE',  ( 8.303920738747214259, 3.683253992019856149, 21.50000000000000000 ) ) ;
#25134 = CARTESIAN_POINT ( 'NONE',  ( 9.184850993605159777E-16, -7.500000000000015099, -16.50000000000000000 ) ) ;
#25135 = DIRECTION ( 'NONE',  ( 0.000000000000000000, -0.000000000000000000, 1.000000000000000000 ) ) ;
#25136 = ORIENTED_EDGE ( 'NONE', *, *, #27910, .F. ) ;
#25137 = CARTESIAN_POINT ( 'NONE',  ( 0.000000000000000000, -2.775557561562891351E-14, 157.4999999999999716 ) ) ;
#25138 = CARTESIAN_POINT ( 'NONE',  ( -8.817355867515827228, -2.185336383880175593, 21.50000000000000000 ) ) ;
#25139 = DIRECTION ( 'NONE',  ( 0.000000000000000000, 0.000000000000000000, 1.000000000000000000 ) ) ;
#25140 = ORIENTED_EDGE ( 'NONE', *, *, #8308, .T. ) ;
#25141 = ORIENTED_EDGE ( 'NONE', *, *, #6377, .T. ) ;
#25142 = CARTESIAN_POINT ( 'NONE',  ( -4.608906612435655248, -7.730328572437724866, 21.50000000000000000 ) ) ;
#25143 = UNCERTAINTY_MEASURE_WITH_UNIT (LENGTH_MEASURE( 1.000000000000000082E-05 ), #10547, 'distance_accuracy_value', 'NONE');
#25144 = CARTESIAN_POINT ( 'NONE',  ( -19.90071050938331609, 1.994113959836040451, 20.22386025856690139 ) ) ;
#25145 = VERTEX_POINT ( 'NONE', #10233 ) ;
#25146 = CARTESIAN_POINT ( 'NONE',  ( 17.84153987719590972, -14.83584055149750114, 1.500000000000000000 ) ) ;
#25147 = AXIS2_PLACEMENT_3D ( 'NONE', #30051, #8692, #22561 ) ;
#25148 = DIRECTION ( 'NONE',  ( 1.000000000000000000, 0.000000000000000000, 0.000000000000000000 ) ) ;
#25149 = DIRECTION ( 'NONE',  ( -1.000000000000000000, 0.000000000000000000, 0.000000000000000000 ) ) ;
#25150 = CARTESIAN_POINT ( 'NONE',  ( -20.50469103882543109, -27.17502484134976015, -16.50001200000000523 ) ) ;
#25151 = DIRECTION ( 'NONE',  ( -0.000000000000000000, -0.000000000000000000, 1.000000000000000000 ) ) ;
#25152 = LINE ( 'NONE', #18148, #9118 ) ;
#25153 = CARTESIAN_POINT ( 'NONE',  ( 1.367976436446960875, -19.97081545247029410, 6.560937769032974209 ) ) ;
#25154 = DIRECTION ( 'NONE',  ( 1.000000000000000000, 0.000000000000000000, 0.000000000000000000 ) ) ;
#25155 = VERTEX_POINT ( 'NONE', #880 ) ;
#25156 = CARTESIAN_POINT ( 'NONE',  ( -9.081360402260857612, -14.40588898056577705, 18.55820869691756769 ) ) ;
#25157 = FACE_OUTER_BOUND ( 'NONE', #30234, .T. ) ;
#25158 = DIRECTION ( 'NONE',  ( 1.000000000000000000, 0.000000000000000000, 0.000000000000000000 ) ) ;
#25159 = CARTESIAN_POINT ( 'NONE',  ( -14.70205207497229871, -8.690259054815006934, 19.25672174529527325 ) ) ;
#25160 = CARTESIAN_POINT ( 'NONE',  ( 20.65888525914559892, 38.75220717792412728, -19.50000000000000355 ) ) ;
#25161 = CARTESIAN_POINT ( 'NONE',  ( -33.54113041553378594, 10.01041480049199173, 35.75454235599931252 ) ) ;
#25162 = VERTEX_POINT ( 'NONE', #9937 ) ;
#25163 = EDGE_CURVE ( 'NONE', #29647, #22222, #22955, .T. ) ;
#25164 = ORIENTED_EDGE ( 'NONE', *, *, #14903, .T. ) ;
#25165 = CARTESIAN_POINT ( 'NONE',  ( -29.61203839202723032, 15.40012917324033381, 37.38016955275591613 ) ) ;
#25166 = CONICAL_SURFACE ( 'NONE', #3256, 5.035999999999999588, 0.7853981633974388421 ) ;
#25167 = CARTESIAN_POINT ( 'NONE',  ( 2.687479362164894248, -44.39187623478217404, -19.50000000000000355 ) ) ;
#25168 = CARTESIAN_POINT ( 'NONE',  ( -5.029589720584652035, -42.14523135961886169, 34.60377126736910469 ) ) ;
#25169 = EDGE_CURVE ( 'NONE', #18098, #20761, #1555, .T. ) ;
#25170 = CYLINDRICAL_SURFACE ( 'NONE', #26082, 20.00000000000000000 ) ;
#25171 = ORIENTED_EDGE ( 'NONE', *, *, #13063, .T. ) ;
#25172 = CARTESIAN_POINT ( 'NONE',  ( 2.687479363073301819, 44.39187623479102740, -19.50000000000000355 ) ) ;
#25173 = CARTESIAN_POINT ( 'NONE',  ( -10.55542352351189095, -17.00870908956209249, 5.651989602109218858 ) ) ;
#25174 = ORIENTED_EDGE ( 'NONE', *, *, #20090, .F. ) ;
#25175 = ADVANCED_FACE ( 'NONE', ( #7754 ), #17258, .T. ) ;
#25176 = CARTESIAN_POINT ( 'NONE',  ( 0.000000000000000000, 0.000000000000000000, 34.49999999999999289 ) ) ;
#25177 = CARTESIAN_POINT ( 'NONE',  ( -9.737156396509783818, -41.16134080394702721, 34.57994222443139165 ) ) ;
#25178 = VERTEX_POINT ( 'NONE', #5563 ) ;
#25179 = DIRECTION ( 'NONE',  ( 1.000000000000000000, 0.000000000000000000, 0.000000000000000000 ) ) ;
#25180 = EDGE_CURVE ( 'NONE', #12762, #2167, #11530, .T. ) ;
#25181 = DIRECTION ( 'NONE',  ( -0.7416830501633041584, 0.6707505147970128645, 0.000000000000000000 ) ) ;
#25182 = DIRECTION ( 'NONE',  ( 0.000000000000000000, 1.000000000000000000, 0.000000000000000000 ) ) ;
#25183 = CARTESIAN_POINT ( 'NONE',  ( 7.548823014270646503, -5.738360882149970976, 21.50000000000000000 ) ) ;
#25184 = ORIENTED_EDGE ( 'NONE', *, *, #3444, .F. ) ;
#25185 = CYLINDRICAL_SURFACE ( 'NONE', #360, 6.000000000000001776 ) ;
#25186 = CIRCLE ( 'NONE', #28687, 9.482273699623480212 ) ;
#25187 = CARTESIAN_POINT ( 'NONE',  ( 8.999114229549594057, -0.1262659238204522361, 21.50000000000000000 ) ) ;
#25188 = CARTESIAN_POINT ( 'NONE',  ( 0.3567147238643519902, -19.99681861211371370, 18.34798005863226678 ) ) ;
#25189 = CARTESIAN_POINT ( 'NONE',  ( -26.36764545593177544, 31.31467416275353344, 1.500000000000000000 ) ) ;
#25190 = VECTOR ( 'NONE', #22601, 1000.000000000000000 ) ;
#25191 = CARTESIAN_POINT ( 'NONE',  ( -17.05026832884990995, 0.8441673869621679760, 6.037360021877316463 ) ) ;
#25192 = LINE ( 'NONE', #16602, #8850 ) ;
#25193 = CARTESIAN_POINT ( 'NONE',  ( 1.000000000000008438, 13.00000000000001421, 24.50000000000000000 ) ) ;
#25194 = DIRECTION ( 'NONE',  ( 1.000000000000000000, 0.000000000000000000, 0.000000000000000000 ) ) ;
#25195 = ADVANCED_FACE ( 'NONE', ( #22401 ), #13364, .F. ) ;
#25196 = EDGE_CURVE ( 'NONE', #16566, #11965, #15531, .T. ) ;
#25197 = EDGE_CURVE ( 'NONE', #16236, #9004, #13517, .T. ) ;
#25198 = DIRECTION ( 'NONE',  ( -0.000000000000000000, -0.000000000000000000, -1.000000000000000000 ) ) ;
#25199 = CARTESIAN_POINT ( 'NONE',  ( -32.19782014694307293, 14.25394737442115733, 39.78814634291943975 ) ) ;
#25200 = CARTESIAN_POINT ( 'NONE',  ( -9.072316094201720915, -14.41194981467785929, 20.14907003336612945 ) ) ;
#25201 = CIRCLE ( 'NONE', #20696, 11.46182693247429718 ) ;
#25202 = ORIENTED_EDGE ( 'NONE', *, *, #12657, .T. ) ;
#25203 = VERTEX_POINT ( 'NONE', #1043 ) ;
#25204 = CARTESIAN_POINT ( 'NONE',  ( 0.000000000000000000, 1.699320956058915452E-16, -1.500000000000001776 ) ) ;
#25205 = CARTESIAN_POINT ( 'NONE',  ( 13.22505861668094340, 42.10773672057246841, -19.50000000000000355 ) ) ;
#25206 = DIRECTION ( 'NONE',  ( 1.000000000000000000, 0.000000000000000000, 0.000000000000000000 ) ) ;
#25207 = EDGE_CURVE ( 'NONE', #8705, #27809, #15498, .T. ) ;
#25208 = EDGE_LOOP ( 'NONE', ( #25482, #9693, #18999, #2162, #4010, #17826 ) ) ;
#25209 = CARTESIAN_POINT ( 'NONE',  ( -6.458576814772031049, 15.80792270644134767, 19.02573955821369367 ) ) ;
#25210 = DIRECTION ( 'NONE',  ( 0.000000000000000000, 0.000000000000000000, 1.000000000000000000 ) ) ;
#25211 = EDGE_CURVE ( 'NONE', #29282, #4972, #14984, .T. ) ;
#25212 = CIRCLE ( 'NONE', #22228, 9.084132297865673777 ) ;
#25213 = EDGE_CURVE ( 'NONE', #24910, #22212, #25047, .T. ) ;
#25214 = ORIENTED_EDGE ( 'NONE', *, *, #12452, .T. ) ;
#25215 = VERTEX_POINT ( 'NONE', #13521 ) ;
#25216 = CARTESIAN_POINT ( 'NONE',  ( -11.35972605147144598, -16.46076013017338013, 19.21471108562412766 ) ) ;
#25217 = CIRCLE ( 'NONE', #7859, 9.000000000000000000 ) ;
#25218 = LINE ( 'NONE', #26248, #13280 ) ;
#25219 = CIRCLE ( 'NONE', #21208, 50.00000000000000000 ) ;
#25220 = CARTESIAN_POINT ( 'NONE',  ( -8.832446728800206870, -14.56826516372322367, 18.39701043959520987 ) ) ;
#25221 = CARTESIAN_POINT ( 'NONE',  ( -8.549354426873712498, 36.53117268482988322, 37.50000000000129319 ) ) ;
#25222 = ORIENTED_EDGE ( 'NONE', *, *, #26131, .F. ) ;
#25223 = DIRECTION ( 'NONE',  ( -1.000000000000000000, 0.000000000000000000, 0.000000000000000000 ) ) ;
#25224 = ORIENTED_EDGE ( 'NONE', *, *, #19283, .T. ) ;
#25225 = CARTESIAN_POINT ( 'NONE',  ( 32.28307784207223108, -8.475829241206289666, 41.62281023987511475 ) ) ;
#25226 = CARTESIAN_POINT ( 'NONE',  ( -16.84890868872602354, 2.447051129731594887, 18.72771030977187579 ) ) ;
#25227 = AXIS2_PLACEMENT_3D ( 'NONE', #24425, #22080, #21466 ) ;
#25228 = ORIENTED_EDGE ( 'NONE', *, *, #18508, .F. ) ;
#25229 = AXIS2_PLACEMENT_3D ( 'NONE', #22508, #1008, #15177 ) ;
#25230 = CARTESIAN_POINT ( 'NONE',  ( -40.00000000000002842, 80.00000000000001421, 17.49999999999982947 ) ) ;
#25231 = ADVANCED_FACE ( 'NONE', ( #1508 ), #13202, .F. ) ;
#25232 = CARTESIAN_POINT ( 'NONE',  ( 24.12434750488276691, -33.40019891058758361, 29.69951012705165283 ) ) ;
#25233 = FACE_OUTER_BOUND ( 'NONE', #1224, .T. ) ;
#25234 = DIRECTION ( 'NONE',  ( -0.000000000000000000, -0.000000000000000000, -1.000000000000000000 ) ) ;
#25235 = CARTESIAN_POINT ( 'NONE',  ( -10.14924625765044119, -17.25430667454972067, 20.25542030744407640 ) ) ;
#25236 = DIRECTION ( 'NONE',  ( 0.9898214418809327952, -0.1423148382732850048, 0.000000000000000000 ) ) ;
#25237 = CARTESIAN_POINT ( 'NONE',  ( -17.00515754968433768, 1.312003563659740690, 18.39992786714538298 ) ) ;
#25238 = CARTESIAN_POINT ( 'NONE',  ( 57.49999999999998579, -50.00000000000000000, 52.07879600563550326 ) ) ;
#25239 = VERTEX_POINT ( 'NONE', #17714 ) ;
#25240 = EDGE_CURVE ( 'NONE', #15826, #26641, #17491, .T. ) ;
#25241 = EDGE_CURVE ( 'NONE', #24237, #20108, #30189, .T. ) ;
#25242 = VECTOR ( 'NONE', #20055, 1000.000000000000000 ) ;
#25243 = CARTESIAN_POINT ( 'NONE',  ( 9.268856789657281325, -38.25380398711768493, 27.49999999999999645 ) ) ;
#25244 = ORIENTED_EDGE ( 'NONE', *, *, #9548, .T. ) ;
#25245 = EDGE_CURVE ( 'NONE', #3989, #3010, #20205, .T. ) ;
#25246 = ORIENTED_EDGE ( 'NONE', *, *, #14151, .F. ) ;
#25247 = CARTESIAN_POINT ( 'NONE',  ( 45.89490515299661411, 69.57600767808649778, 14.41534730701735256 ) ) ;
#25248 = CYLINDRICAL_SURFACE ( 'NONE', #13641, 0.7500000000000006661 ) ;
#25249 = CARTESIAN_POINT ( 'NONE',  ( -4.673829994069186533, 16.36915245889226256, 6.211014596808754007 ) ) ;
#25250 = ORIENTED_EDGE ( 'NONE', *, *, #9154, .F. ) ;
#25251 = CARTESIAN_POINT ( 'NONE',  ( 6.900000000000000355, -7.794228634059938265, -4.500000000000013323 ) ) ;
#25252 = CIRCLE ( 'NONE', #18291, 0.7500000000000007772 ) ;
#25253 =( BOUNDED_SURFACE ( )  B_SPLINE_SURFACE ( 3, 1, ( 
 ( #7175, #9513 ),
 ( #21046, #16380 ),
 ( #21505, #25895 ),
 ( #11859, #9207 ) ),
 .UNSPECIFIED., .F., .F., .T. ) 
 B_SPLINE_SURFACE_WITH_KNOTS ( ( 4, 4 ),
 ( 2, 2 ),
 ( 0.000000000000000000, 1.000000000000000000 ),
 ( 0.000000000000000000, 1.000000000000000000 ),
 .UNSPECIFIED. ) 
 GEOMETRIC_REPRESENTATION_ITEM ( )  RATIONAL_B_SPLINE_SURFACE ( (
 ( 1.000000000000000000, 1.000000000000000000),
 ( 0.3333333333333333703, 0.3333333333333333703),
 ( 0.3333333333333333703, 0.3333333333333333703),
 ( 1.000000000000000000, 1.000000000000000000) ) ) 
 REPRESENTATION_ITEM ( '' )  SURFACE ( )  );
#25254 = CARTESIAN_POINT ( 'NONE',  ( -12.79952941389652921, 11.22436372988652664, 6.143977687428009204 ) ) ;
#25255 = MECHANICAL_DESIGN_GEOMETRIC_PRESENTATION_REPRESENTATION (  '', ( #24238 ), #26673 ) ;
#25256 = LINE ( 'NONE', #29794, #18895 ) ;
#25257 = EDGE_LOOP ( 'NONE', ( #26385, #11203, #19156, #13507 ) ) ;
#25258 = DIRECTION ( 'NONE',  ( 1.000000000000000000, 0.000000000000000000, 0.000000000000000000 ) ) ;
#25259 = AXIS2_PLACEMENT_3D ( 'NONE', #13982, #1670, #9005 ) ;
#25260 = DIRECTION ( 'NONE',  ( -0.000000000000000000, 1.132880637372608986E-16, -1.000000000000000000 ) ) ;
#25261 = ORIENTED_EDGE ( 'NONE', *, *, #4387, .F. ) ;
#25262 = AXIS2_PLACEMENT_3D ( 'NONE', #10302, #5636, #14827 ) ;
#25263 = CARTESIAN_POINT ( 'NONE',  ( 12.57902516942791671, 11.48976026227458291, 5.701226463332907279 ) ) ;
#25264 = ORIENTED_EDGE ( 'NONE', *, *, #26374, .F. ) ;
#25265 = CARTESIAN_POINT ( 'NONE',  ( -13.37849590498012553, 10.56201291617987792, 20.34789198813115263 ) ) ;
#25266 = AXIS2_PLACEMENT_3D ( 'NONE', #28230, #5140, #14651 ) ;
#25267 = ORIENTED_EDGE ( 'NONE', *, *, #13934, .T. ) ;
#25268 = ORIENTED_EDGE ( 'NONE', *, *, #14679, .F. ) ;
#25269 = AXIS2_PLACEMENT_3D ( 'NONE', #28927, #17063, #10051 ) ;
#25270 = EDGE_CURVE ( 'NONE', #5874, #21024, #11017, .T. ) ;
#25271 = DIRECTION ( 'NONE',  ( 1.000000000000000000, 0.000000000000000000, 0.000000000000000000 ) ) ;
#25272 = CARTESIAN_POINT ( 'NONE',  ( 6.237549684377466264, 19.00251437819607858, 19.60917204426171523 ) ) ;
#25273 = AXIS2_PLACEMENT_3D ( 'NONE', #10980, #6739, #20626 ) ;
#25274 = ORIENTED_EDGE ( 'NONE', *, *, #10561, .F. ) ;
#25275 = CIRCLE ( 'NONE', #871, 0.6002263538043630664 ) ;
#25276 = CARTESIAN_POINT ( 'NONE',  ( -4.375757216953428294E-15, -39.50000000000000000, 34.80090346875804386 ) ) ;
#25277 = CARTESIAN_POINT ( 'NONE',  ( 9.138492726993298731, -14.36378254522091780, 18.80699882434806369 ) ) ;
#25278 = DIRECTION ( 'NONE',  ( 1.000000000000000000, 0.000000000000000000, 0.000000000000000000 ) ) ;
#25279 = VERTEX_POINT ( 'NONE', #3538 ) ;
#25280 = AXIS2_PLACEMENT_3D ( 'NONE', #24343, #5639, #3285 ) ;
#25281 = LINE ( 'NONE', #6095, #28694 ) ;
#25282 = DIRECTION ( 'NONE',  ( -0.000000000000000000, 1.132880637372608986E-16, -1.000000000000000000 ) ) ;
#25283 = VECTOR ( 'NONE', #27303, 1000.000000000000227 ) ;
#25284 = CARTESIAN_POINT ( 'NONE',  ( 39.99999999999998579, 90.00000000000001421, 52.49999999999999289 ) ) ;
#25285 = CARTESIAN_POINT ( 'NONE',  ( 5.303644920943711760, 19.30240823413181062, 20.34789198813115263 ) ) ;
#25286 = EDGE_LOOP ( 'NONE', ( #27111, #22027, #1829, #29101 ) ) ;
#25287 = VERTEX_POINT ( 'NONE', #24732 ) ;
#25288 = AXIS2_PLACEMENT_3D ( 'NONE', #17558, #8056, #19736 ) ;
#25289 = DIRECTION ( 'NONE',  ( 1.000000000000000000, 0.000000000000000000, -0.000000000000000000 ) ) ;
#25290 = FACE_OUTER_BOUND ( 'NONE', #26265, .T. ) ;
#25291 = CARTESIAN_POINT ( 'NONE',  ( -5.205279254987321025, 19.32936484843851588, 19.96783386855779341 ) ) ;
#25292 = DIRECTION ( 'NONE',  ( -0.000000000000000000, 1.132880637372608986E-16, -1.000000000000000000 ) ) ;
#25293 = VECTOR ( 'NONE', #9391, 1000.000000000000000 ) ;
#25294 = FACE_OUTER_BOUND ( 'NONE', #24922, .T. ) ;
#25295 = DIRECTION ( 'NONE',  ( 0.000000000000000000, 0.000000000000000000, 1.000000000000000000 ) ) ;
#25296 = CARTESIAN_POINT ( 'NONE',  ( 0.000000000000000000, 0.000000000000000000, -52.50000000000000000 ) ) ;
#25297 = AXIS2_PLACEMENT_3D ( 'NONE', #24411, #3053, #5544 ) ;
#25298 = ORIENTED_EDGE ( 'NONE', *, *, #21799, .F. ) ;
#25299 = VECTOR ( 'NONE', #18305, 1000.000000000000000 ) ;
#25300 = CARTESIAN_POINT ( 'NONE',  ( -33.43088607478084384, -9.613432587296607323, 35.97188228570009727 ) ) ;
#25301 = AXIS2_PLACEMENT_3D ( 'NONE', #26942, #10082, #5562 ) ;
#25302 = DIRECTION ( 'NONE',  ( -0.000000000000000000, 1.132880637372608986E-16, -1.000000000000000000 ) ) ;
#25303 = CARTESIAN_POINT ( 'NONE',  ( 19.74328841314634886, 3.194145055459934213, 20.34789198813115263 ) ) ;
#25304 = ORIENTED_EDGE ( 'NONE', *, *, #22585, .F. ) ;
#25305 = VERTEX_POINT ( 'NONE', #29897 ) ;
#25306 = DIRECTION ( 'NONE',  ( 0.000000000000000000, 0.000000000000000000, 1.000000000000000000 ) ) ;
#25307 = AXIS2_PLACEMENT_3D ( 'NONE', #30372, #4017, #11040 ) ;
#25308 = DIRECTION ( 'NONE',  ( 0.1423148382732889183, 0.9898214418809321291, 0.000000000000000000 ) ) ;
#25309 = EDGE_LOOP ( 'NONE', ( #3001, #17970, #11259, #11485, #14989, #23949, #27630, #2752, #25250, #13593, #12225, #28407, #1246, #22676, #6249, #23849, #27930, #28707 ) ) ;
#25310 = CARTESIAN_POINT ( 'NONE',  ( -0.4553004113513133833, -19.99503986737293815, 7.267242832833950672 ) ) ;
#25311 = VECTOR ( 'NONE', #21102, 1000.000000000000227 ) ;
#25312 = CARTESIAN_POINT ( 'NONE',  ( 14.99996214399394567, 47.69697197601039562, -55.49547544386297204 ) ) ;
#25313 = CARTESIAN_POINT ( 'NONE',  ( -50.00000000000000000, 70.00000000000000000, -75.50000000000002842 ) ) ;
#25314 = DIRECTION ( 'NONE',  ( 0.000000000000000000, 0.000000000000000000, -1.000000000000000000 ) ) ;
#25315 = CARTESIAN_POINT ( 'NONE',  ( 15.43499236066653779, -3.229500095980125440, 1.500000000000001332 ) ) ;
#25316 = DIRECTION ( 'NONE',  ( -1.000000000000000000, 0.000000000000000000, 0.000000000000000000 ) ) ;
#25317 = CARTESIAN_POINT ( 'NONE',  ( -16.89625272878625140, 2.150609578402132183, 5.774779864094945481 ) ) ;
#25318 = ORIENTED_EDGE ( 'NONE', *, *, #1002, .F. ) ;
#25319 = B_SPLINE_CURVE_WITH_KNOTS ( 'NONE', 3,
 ( #14336, #2492, #23389, #26356 ),
 .UNSPECIFIED., .F., .F.,
 ( 4, 4 ),
 ( 2.143643656977389965E-07, 0.003421830178490238485 ),
 .UNSPECIFIED. ) ;
#25320 = AXIS2_PLACEMENT_3D ( 'NONE', #13158, #22359, #15486 ) ;
#25321 = VECTOR ( 'NONE', #18752, 1000.000000000000000 ) ;
#25322 = CARTESIAN_POINT ( 'NONE',  ( 40.89187623478217404, 5.790488632116406187, -19.50000000000000355 ) ) ;
#25323 = CARTESIAN_POINT ( 'NONE',  ( -6.028330626922774549, 10.93629592680536788, 24.50000000000000000 ) ) ;
#25324 = LINE ( 'NONE', #18156, #3096 ) ;
#25325 = CARTESIAN_POINT ( 'NONE',  ( -15.06439250341027147, -7.989583865232170012, 18.37415474056476938 ) ) ;
#25326 = CARTESIAN_POINT ( 'NONE',  ( -10.11202017158466759, 41.14070756921185534, -1.500000000000000000 ) ) ;
#25327 = CARTESIAN_POINT ( 'NONE',  ( -32.49060333908415288, 8.555881924488323520, 37.15911814905553001 ) ) ;
#25328 = VECTOR ( 'NONE', #6764, 1000.000000000000000 ) ;
#25329 = ORIENTED_EDGE ( 'NONE', *, *, #7744, .F. ) ;
#25330 = APPLICATION_CONTEXT ( 'automotive_design' ) ;
#25331 = LINE ( 'NONE', #18162, #26859 ) ;
#25332 = CARTESIAN_POINT ( 'NONE',  ( -13.22505861668184046, -42.10773672057003125, -19.50000000000000355 ) ) ;
#25333 = CARTESIAN_POINT ( 'NONE',  ( 19.81438245631380113, -36.63624637273056095, 34.51461286089641334 ) ) ;
#25334 = DIRECTION ( 'NONE',  ( 0.000000000000000000, 0.000000000000000000, 1.000000000000000000 ) ) ;
#25335 = ORIENTED_EDGE ( 'NONE', *, *, #20958, .F. ) ;
#25336 = CARTESIAN_POINT ( 'NONE',  ( 3.089102459999460315, 16.79563822435759590, 6.917457548096561659 ) ) ;
#25337 = CARTESIAN_POINT ( 'NONE',  ( 5.374868878254059013, -44.10336124695543703, -19.50000000000000355 ) ) ;
#25338 = DIRECTION ( 'NONE',  ( -0.000000000000000000, -0.000000000000000000, 1.000000000000000000 ) ) ;
#25339 = ORIENTED_EDGE ( 'NONE', *, *, #30184, .F. ) ;
#25340 = CIRCLE ( 'NONE', #30810, 0.7500000000000024425 ) ;
#25341 = CARTESIAN_POINT ( 'NONE',  ( -57.50000000000001421, -50.00000000000000000, 52.07879600563550326 ) ) ;
#25342 = AXIS2_PLACEMENT_3D ( 'NONE', #15304, #6105, #1284 ) ;
#25343 = CARTESIAN_POINT ( 'NONE',  ( -10.60011131210715440, -35.97541730661800585, 37.50000000000953548 ) ) ;
#25344 = EDGE_CURVE ( 'NONE', #27501, #19329, #8827, .T. ) ;
#25345 = ORIENTED_EDGE ( 'NONE', *, *, #24384, .T. ) ;
#25346 = CARTESIAN_POINT ( 'NONE',  ( 11.10715495309692891, -16.63223102436628409, 7.652108011868850035 ) ) ;
#25347 = DIRECTION ( 'NONE',  ( 0.000000000000000000, -1.132880637372608986E-16, 1.000000000000000000 ) ) ;
#25348 = DIRECTION ( 'NONE',  ( 0.000000000000000000, 0.000000000000000000, -1.000000000000000000 ) ) ;
#25349 = CIRCLE ( 'NONE', #2441, 0.7441270634457337607 ) ;
#25350 = CARTESIAN_POINT ( 'NONE',  ( 0.7836603910024348973, -17.02734626465442247, 18.34798005862662507 ) ) ;
#25351 = ORIENTED_EDGE ( 'NONE', *, *, #80, .T. ) ;
#25352 = CARTESIAN_POINT ( 'NONE',  ( 0.000000000000000000, -14.99999999999997158, -55.00000000000000711 ) ) ;
#25353 = B_SPLINE_CURVE_WITH_KNOTS ( 'NONE', 3,
 ( #7375, #14065, #25931, #17029, #26233 ),
 .UNSPECIFIED., .F., .F.,
 ( 4, 1, 4 ),
 ( 0.3464918507984035556, 0.3518176900574713217, 0.3571435293165390878 ),
 .UNSPECIFIED. ) ;
#25354 = CARTESIAN_POINT ( 'NONE',  ( -37.16608720827707657, 65.00000000000000000, 15.49999999999998579 ) ) ;
#25355 = FACE_OUTER_BOUND ( 'NONE', #18987, .T. ) ;
#25356 = EDGE_CURVE ( 'NONE', #21157, #27347, #27553, .T. ) ;
#25357 = DIRECTION ( 'NONE',  ( -0.000000000000000000, -0.000000000000000000, -1.000000000000000000 ) ) ;
#25358 = VECTOR ( 'NONE', #22830, 1000.000000000000000 ) ;
#25359 = EDGE_CURVE ( 'NONE', #3526, #17261, #576, .T. ) ;
#25360 = CARTESIAN_POINT ( 'NONE',  ( 53.00000000000045475, -4.861708391419322267E-13, 62.49999999999998579 ) ) ;
#25361 = DIRECTION ( 'NONE',  ( -1.000000000000000000, 0.000000000000000000, 0.000000000000000000 ) ) ;
#25362 = DIRECTION ( 'NONE',  ( 1.000000000000000000, 0.000000000000000000, 0.000000000000000000 ) ) ;
#25363 = CARTESIAN_POINT ( 'NONE',  ( 7.974144905643788306, 5.130938270761631337, 1.500000000000001332 ) ) ;
#25364 = CARTESIAN_POINT ( 'NONE',  ( 19.78337026033623403, 2.938244205458795388, 5.676722608126685721 ) ) ;
#25365 = CARTESIAN_POINT ( 'NONE',  ( -9.395142731145691428, -14.19351217900080719, 19.21496526180053976 ) ) ;
#25366 = CIRCLE ( 'NONE', #11926, 6.000000000000005329 ) ;
#25367 = ORIENTED_EDGE ( 'NONE', *, *, #10232, .F. ) ;
#25368 = EDGE_LOOP ( 'NONE', ( #14813, #9823, #21848 ) ) ;
#25369 = B_SPLINE_CURVE_WITH_KNOTS ( 'NONE', 3,
 ( #8226, #27419, #6036, #15545, #18050, #25209, #9459, #23474, #25678, #9140, #20975, #25835, #23166, #6794, #16621, #16319 ),
 .UNSPECIFIED., .F., .F.,
 ( 4, 2, 2, 2, 2, 2, 2, 4 ),
 ( 0.5000000000000001110, 0.6250000000000007772, 0.6875000000000013323, 0.7187500000000017764, 0.7500000000000022204, 0.8125000000000015543, 0.8750000000000006661, 1.000000000000000000 ),
 .UNSPECIFIED. ) ;
#25370 = EDGE_CURVE ( 'NONE', #19662, #30243, #18030, .T. ) ;
#25371 = FACE_BOUND ( 'NONE', #21941, .T. ) ;
#25372 = CARTESIAN_POINT ( 'NONE',  ( -50.00000000000000000, 50.00000000000000000, -92.50000000000000000 ) ) ;
#25373 = CARTESIAN_POINT ( 'NONE',  ( -3.515970705488605130, -17.06554576617236307, -1.500000000000000000 ) ) ;
#25374 = ORIENTED_EDGE ( 'NONE', *, *, #15692, .T. ) ;
#25375 =( NAMED_UNIT ( * ) SI_UNIT ( $, .STERADIAN. ) SOLID_ANGLE_UNIT ( ) );
#25376 = VECTOR ( 'NONE', #2037, 1000.000000000000000 ) ;
#25377 = CARTESIAN_POINT ( 'NONE',  ( 26.80246859415415273, -7.028748154183637631, -1.499999999999999556 ) ) ;
#25378 = CARTESIAN_POINT ( 'NONE',  ( 5.687793815610356241, -6.974883619896809606, 1.500000000000001332 ) ) ;
#25379 = ORIENTED_EDGE ( 'NONE', *, *, #9404, .T. ) ;
#25380 = ORIENTED_EDGE ( 'NONE', *, *, #15695, .T. ) ;
#25381 = CARTESIAN_POINT ( 'NONE',  ( -11.03465445395214672, -16.68068344163647510, 18.54479204710284890 ) ) ;
#25382 = B_SPLINE_CURVE_WITH_KNOTS ( 'NONE', 3,
 ( #23152, #23457, #25968, #18188, #1654, #11322 ),
 .UNSPECIFIED., .F., .F.,
 ( 4, 2, 4 ),
 ( 0.001794032523744855520, 0.007046146517949118150, 0.01388807892444184240 ),
 .UNSPECIFIED. ) ;
#25383 = AXIS2_PLACEMENT_3D ( 'NONE', #29847, #10494, #20005 ) ;
#25384 = DIRECTION ( 'NONE',  ( 0.000000000000000000, 0.000000000000000000, -1.000000000000000000 ) ) ;
#25385 = CARTESIAN_POINT ( 'NONE',  ( -3.653991135135629342, -43.89827854335435120, -16.50000000000000355 ) ) ;
#25386 = CARTESIAN_POINT ( 'NONE',  ( -0.4404457618616001158, 37.56938067690362715, 37.49999999996049382 ) ) ;
#25387 = ORIENTED_EDGE ( 'NONE', *, *, #30177, .F. ) ;
#25388 = LINE ( 'NONE', #20987, #24789 ) ;
#25389 = ADVANCED_FACE ( 'NONE', ( #5712 ), #3378, .F. ) ;
#25390 = EDGE_LOOP ( 'NONE', ( #7371, #27789 ) ) ;
#25391 = ADVANCED_FACE ( 'NONE', ( #12905 ), #11325, .T. ) ;
#25392 = DIRECTION ( 'NONE',  ( 1.000000000000000000, 0.000000000000000000, 0.000000000000000000 ) ) ;
#25393 = CARTESIAN_POINT ( 'NONE',  ( -70.00000000000000000, 70.00000000000000000, -92.50000000000000000 ) ) ;
#25394 = ORIENTED_EDGE ( 'NONE', *, *, #23124, .F. ) ;
#25395 = DIRECTION ( 'NONE',  ( -0.5406408174555976665, 0.8412535328311812055, 0.000000000000000000 ) ) ;
#25396 = SURFACE_STYLE_FILL_AREA ( #28032 ) ;
#25397 = EDGE_CURVE ( 'NONE', #24446, #28753, #30343, .T. ) ;
#25398 = CARTESIAN_POINT ( 'NONE',  ( 57.49999999999998579, 50.00000000000000000, 97.07879600563551037 ) ) ;
#25399 = CARTESIAN_POINT ( 'NONE',  ( 16.68770897235365780, 3.522277800415036353, 7.603368798681074736 ) ) ;
#25400 = CARTESIAN_POINT ( 'NONE',  ( 1.588511040490847792, -16.99700008610011182, 7.269896094239231665 ) ) ;
#25401 = EDGE_CURVE ( 'NONE', #16767, #27365, #23317, .T. ) ;
#25402 = LINE ( 'NONE', #18394, #8070 ) ;
#25403 = CARTESIAN_POINT ( 'NONE',  ( -9.290115248528675096, -14.26557846602795188, 7.156916968540300239 ) ) ;
#25404 = DIRECTION ( 'NONE',  ( 0.000000000000000000, 0.000000000000000000, -1.000000000000000000 ) ) ;
#25405 = ORIENTED_EDGE ( 'NONE', *, *, #14566, .F. ) ;
#25406 = EDGE_CURVE ( 'NONE', #15501, #11969, #16148, .T. ) ;
#25407 = CIRCLE ( 'NONE', #11962, 9.084132297865673777 ) ;
#25408 = DIRECTION ( 'NONE',  ( -0.000000000000000000, 0.000000000000000000, 1.000000000000000000 ) ) ;
#25409 = CARTESIAN_POINT ( 'NONE',  ( 28.55068628633582861, -24.19494186940697844, 27.50000000000000355 ) ) ;
#25410 = EDGE_CURVE ( 'NONE', #11295, #26463, #23972, .T. ) ;
#25411 = ORIENTED_EDGE ( 'NONE', *, *, #10385, .F. ) ;
#25412 = ORIENTED_EDGE ( 'NONE', *, *, #29419, .F. ) ;
#25413 = EDGE_CURVE ( 'NONE', #498, #11642, #9528, .T. ) ;
#25414 = PLANE ( 'NONE',  #9322 ) ;
#25415 = CARTESIAN_POINT ( 'NONE',  ( -4.626122995383915359, 16.38173570853530592, 6.310736198168394928 ) ) ;
#25416 = VERTEX_POINT ( 'NONE', #13815 ) ;
#25417 = CARTESIAN_POINT ( 'NONE',  ( 11.61739189738757894, -16.28020533589261376, 20.15039051365864253 ) ) ;
#25418 = LINE ( 'NONE', #1854, #15661 ) ;
#25419 = CARTESIAN_POINT ( 'NONE',  ( 23.59223810913926656, 12.86535672232149707, 48.12792051025102325 ) ) ;
#25420 = VERTEX_POINT ( 'NONE', #25518 ) ;
#25421 = DIRECTION ( 'NONE',  ( 1.000000000000000000, 0.000000000000000000, 0.000000000000000000 ) ) ;
#25422 = CIRCLE ( 'NONE', #27430, 6.000000000000005329 ) ;
#25423 = CARTESIAN_POINT ( 'NONE',  ( -33.19297012087366028, -9.154531925606914200, 40.56825029428927110 ) ) ;
#25424 = ORIENTED_EDGE ( 'NONE', *, *, #3097, .F. ) ;
#25425 = CARTESIAN_POINT ( 'NONE',  ( 25.47847050916410439, -26.57182937991349903, 26.54355021145562787 ) ) ;
#25426 = EDGE_CURVE ( 'NONE', #15589, #1105, #7560, .T. ) ;
#25427 = EDGE_LOOP ( 'NONE', ( #15864, #9875 ) ) ;
#25428 = DIRECTION ( 'NONE',  ( 0.000000000000000000, 0.000000000000000000, 1.000000000000000000 ) ) ;
#25429 = EDGE_CURVE ( 'NONE', #24493, #3904, #30797, .T. ) ;
#25430 = ORIENTED_EDGE ( 'NONE', *, *, #189, .F. ) ;
#25431 = EDGE_CURVE ( 'NONE', #13626, #26229, #1958, .T. ) ;
#25432 = CIRCLE ( 'NONE', #3952, 1.447898107987198646 ) ;
#25433 = EDGE_LOOP ( 'NONE', ( #12690, #30505 ) ) ;
#25434 = EDGE_CURVE ( 'NONE', #16733, #30322, #30634, .T. ) ;
#25435 = CARTESIAN_POINT ( 'NONE',  ( 4.608906612435600181, 7.730328572437758616, 21.50000000000000000 ) ) ;
#25436 = FACE_OUTER_BOUND ( 'NONE', #11255, .T. ) ;
#25437 = ORIENTED_EDGE ( 'NONE', *, *, #29414, .T. ) ;
#25438 = CARTESIAN_POINT ( 'NONE',  ( -34.83396020575242602, 10.30249279383516381, 34.80090346875805096 ) ) ;
#25439 = CARTESIAN_POINT ( 'NONE',  ( 10.30772981839320579, -17.16011447240169474, 19.00652017443069752 ) ) ;
#25440 = DIRECTION ( 'NONE',  ( 0.000000000000000000, 0.000000000000000000, 1.000000000000000000 ) ) ;
#25441 = ORIENTED_EDGE ( 'NONE', *, *, #3451, .T. ) ;
#25442 = ADVANCED_FACE ( 'NONE', ( #9127 ), #18647, .T. ) ;
#25443 = CARTESIAN_POINT ( 'NONE',  ( 24.03057240117691862, 26.57182937991349903, 1.500000000000000000 ) ) ;
#25444 = CARTESIAN_POINT ( 'NONE',  ( 18.21411928606760711, -8.304179478877907528, 7.595116371587256054 ) ) ;
#25445 = AXIS2_PLACEMENT_3D ( 'NONE', #16969, #6999, #26487 ) ;
#25446 = CARTESIAN_POINT ( 'NONE',  ( -13.59632618586111441, 10.29740991163844832, 5.704143890883081269 ) ) ;
#25447 = CARTESIAN_POINT ( 'NONE',  ( 3.215610563331060767, 16.76717343535964133, 19.89182036555910571 ) ) ;
#25448 = VERTEX_POINT ( 'NONE', #28321 ) ;
#25449 = ORIENTED_EDGE ( 'NONE', *, *, #9192, .F. ) ;
#25450 = FACE_OUTER_BOUND ( 'NONE', #9284, .T. ) ;
#25451 = CARTESIAN_POINT ( 'NONE',  ( 9.860909914091287476, -13.90333503830274609, 7.652108011868850923 ) ) ;
#25452 = CARTESIAN_POINT ( 'NONE',  ( 12.99340803228152197, 10.99622480873287955, 6.910395520694541993 ) ) ;
#25453 = FILL_AREA_STYLE ('',( #27945 ) ) ;
#25454 = CARTESIAN_POINT ( 'NONE',  ( 12.17894461897553526, 11.93905285453845089, 5.653604225791663218 ) ) ;
#25455 = CARTESIAN_POINT ( 'NONE',  ( -7.946654084575756727, 38.53100927994441349, 27.50000000000000711 ) ) ;
#25456 = ITEM_DEFINED_TRANSFORMATION ( 'NONE', 'NONE', #15879,  #7396 ) ;
#25457 = CARTESIAN_POINT ( 'NONE',  ( 23.15419545472249041, -10.94206393902796925, 49.39104690845173451 ) ) ;
#25458 = EDGE_CURVE ( 'NONE', #1564, #21044, #20489, .T. ) ;
#25459 = EDGE_LOOP ( 'NONE', ( #2348, #8799 ) ) ;
#25460 = EDGE_CURVE ( 'NONE', #12213, #14363, #2099, .T. ) ;
#25461 = CARTESIAN_POINT ( 'NONE',  ( -17.03429152191317542, 1.023117790763819590, 7.441806358946449151 ) ) ;
#25462 = DIRECTION ( 'NONE',  ( 0.000000000000000000, 0.000000000000000000, 1.000000000000000000 ) ) ;
#25463 = CARTESIAN_POINT ( 'NONE',  ( -40.00000000000002842, 90.00000000000001421, 57.50000000000015632 ) ) ;
#25464 = ORIENTED_EDGE ( 'NONE', *, *, #13501, .T. ) ;
#25465 = DIRECTION ( 'NONE',  ( 0.000000000000000000, 0.000000000000000000, 1.000000000000000000 ) ) ;
#25466 = VERTEX_POINT ( 'NONE', #6947 ) ;
#25467 = CARTESIAN_POINT ( 'NONE',  ( 18.35307771382468900, -7.992233955150555680, 5.652196082364320695 ) ) ;
#25468 = VECTOR ( 'NONE', #17673, 1000.000000000000000 ) ;
#25469 = UNCERTAINTY_MEASURE_WITH_UNIT (LENGTH_MEASURE( 1.000000000000000082E-05 ), #30684, 'distance_accuracy_value', 'NONE');
#25470 = CIRCLE ( 'NONE', #1063, 0.7500000000000002220 ) ;
#25471 = DIRECTION ( 'NONE',  ( -0.000000000000000000, -0.000000000000000000, -1.000000000000000000 ) ) ;
#25472 = ORIENTED_EDGE ( 'NONE', *, *, #11100, .F. ) ;
#25473 = CARTESIAN_POINT ( 'NONE',  ( -0.4522595252855811654, -19.99510590919688013, 6.033082186765056143 ) ) ;
#25474 = CARTESIAN_POINT ( 'NONE',  ( 9.161835861599374908, 49.16032949430592680, -66.91699464352380744 ) ) ;
#25475 = CARTESIAN_POINT ( 'NONE',  ( -19.64177907938615064, -36.71644397333972876, 24.50000000000000000 ) ) ;
#25476 = VECTOR ( 'NONE', #8185, 1000.000000000000000 ) ;
#25477 = DIRECTION ( 'NONE',  ( -0.9898214418809327952, 0.1423148382732851158, 0.000000000000000000 ) ) ;
#25478 = CARTESIAN_POINT ( 'NONE',  ( -10.51100883930070040, -17.01524884273342764, 18.34798005863226678 ) ) ;
#25479 = LINE ( 'NONE', #18300, #28767 ) ;
#25480 = CARTESIAN_POINT ( 'NONE',  ( -4.163336342344337027E-14, -1.387778780781445676E-14, -1.500000000000000000 ) ) ;
#25481 = FACE_OUTER_BOUND ( 'NONE', #27239, .T. ) ;
#25482 = ORIENTED_EDGE ( 'NONE', *, *, #25101, .F. ) ;
#25483 = FACE_OUTER_BOUND ( 'NONE', #28393, .T. ) ;
#25484 = DIRECTION ( 'NONE',  ( 1.000000000000000000, 0.000000000000000000, 0.000000000000000000 ) ) ;
#25485 = VERTEX_POINT ( 'NONE', #16456 ) ;
#25486 = CYLINDRICAL_SURFACE ( 'NONE', #15557, 0.7499999999999997780 ) ;
#25487 = DIRECTION ( 'NONE',  ( 0.000000000000000000, 1.000000000000000000, 0.000000000000000000 ) ) ;
#25488 = CARTESIAN_POINT ( 'NONE',  ( -2.552544030762004645, -42.50000000000000000, -1.500000000000000000 ) ) ;
#25489 = AXIS2_PLACEMENT_3D ( 'NONE', #3953, #13474, #23412 ) ;
#25490 = VERTEX_POINT ( 'NONE', #25970 ) ;
#25491 = DIRECTION ( 'NONE',  ( 0.000000000000000000, 0.000000000000000000, 1.000000000000000000 ) ) ;
#25492 = FACE_OUTER_BOUND ( 'NONE', #15008, .T. ) ;
#25493 = CARTESIAN_POINT ( 'NONE',  ( 37.99594503683577074, -9.942093294496530120, 34.97541777410600616 ) ) ;
#25494 = FACE_BOUND ( 'NONE', #2202, .T. ) ;
#25495 = ORIENTED_EDGE ( 'NONE', *, *, #21025, .T. ) ;
#25496 = CARTESIAN_POINT ( 'NONE',  ( -13.93282946021075830, 9.868441342986791653, 6.147510495896838734 ) ) ;
#25497 = VERTEX_POINT ( 'NONE', #14098 ) ;
#25498 = ADVANCED_FACE ( 'NONE', ( #23607 ), #2250, .T. ) ;
#25499 = CARTESIAN_POINT ( 'NONE',  ( -25.19442432475839055, 35.44676296258369064, -19.50000000000000355 ) ) ;
#25500 = CARTESIAN_POINT ( 'NONE',  ( 20.71335220384823117, 27.86167394782616213, -6.500000000000000888 ) ) ;
#25501 = EDGE_CURVE ( 'NONE', #11387, #26848, #10015, .T. ) ;
#25502 = ORIENTED_EDGE ( 'NONE', *, *, #5764, .T. ) ;
#25503 = AXIS2_PLACEMENT_3D ( 'NONE', #16492, #18993, #26009 ) ;
#25504 = CARTESIAN_POINT ( 'NONE',  ( -15.50214450999369831, -39.10813156751746789, 34.54020706897479442 ) ) ;
#25505 = ORIENTED_EDGE ( 'NONE', *, *, #25401, .F. ) ;
#25506 = CARTESIAN_POINT ( 'NONE',  ( -27.03074382657074537, -6.449748410230988327, 42.96778633356042576 ) ) ;
#25507 = EDGE_CURVE ( 'NONE', #24988, #23272, #18455, .T. ) ;
#25508 = AXIS2_PLACEMENT_3D ( 'NONE', #19129, #11646, #9468 ) ;
#25509 = CARTESIAN_POINT ( 'NONE',  ( 8.549050687778162683, 4.102102735472488604, 1.500000000000001332 ) ) ;
#25510 = CARTESIAN_POINT ( 'NONE',  ( 1.836970198721033928E-15, -15.00000000000003375, -87.50000000000000000 ) ) ;
#25511 = ORIENTED_EDGE ( 'NONE', *, *, #9181, .T. ) ;
#25512 = FACE_OUTER_BOUND ( 'NONE', #14417, .T. ) ;
#25513 = DIRECTION ( 'NONE',  ( -0.000000000000000000, 1.132880637372608986E-16, -1.000000000000000000 ) ) ;
#25514 = DIRECTION ( 'NONE',  ( 0.000000000000000000, 1.000000000000000000, 0.000000000000000000 ) ) ;
#25515 = FACE_OUTER_BOUND ( 'NONE', #22245, .T. ) ;
#25516 = CARTESIAN_POINT ( 'NONE',  ( -15.16307827826492449, -7.786259562520723598, 18.34798005863078885 ) ) ;
#25517 = DIRECTION ( 'NONE',  ( -0.000000000000000000, 0.000000000000000000, 1.000000000000000000 ) ) ;
#25518 = CARTESIAN_POINT ( 'NONE',  ( 7.538175180318423152, 5.069257791428403159, 21.50000000000000000 ) ) ;
#25519 = CARTESIAN_POINT ( 'NONE',  ( 6.899999999999999467, 5.196152422706624030, 9.000000000000001776 ) ) ;
#25520 = VECTOR ( 'NONE', #12197, 1000.000000000000000 ) ;
#25521 = CARTESIAN_POINT ( 'NONE',  ( -15.46558767506643761, -7.123678207069782609, 20.05479082170252525 ) ) ;
#25522 = DIRECTION ( 'NONE',  ( -0.000000000000000000, -0.000000000000000000, 1.000000000000000000 ) ) ;
#25523 = VERTEX_POINT ( 'NONE', #22489 ) ;
#25524 = VERTEX_POINT ( 'NONE', #3635 ) ;
#25525 = CARTESIAN_POINT ( 'NONE',  ( 33.78553873773097393, 24.40792641592722134, -16.50000000000000000 ) ) ;
#25526 = DIRECTION ( 'NONE',  ( 0.000000000000000000, 0.000000000000000000, 1.000000000000000000 ) ) ;
#25527 = FACE_OUTER_BOUND ( 'NONE', #22936, .T. ) ;
#25528 = ORIENTED_EDGE ( 'NONE', *, *, #10538, .T. ) ;
#25529 = CARTESIAN_POINT ( 'NONE',  ( 49.99999999999999289, 50.00000000000000000, 70.00000000000000000 ) ) ;
#25530 = CARTESIAN_POINT ( 'NONE',  ( -32.82330813384598400, -22.94799032726886523, -1.500000000000000000 ) ) ;
#25531 = CARTESIAN_POINT ( 'NONE',  ( 9.343263424981191889, -14.23786665600031576, 18.54473042795395443 ) ) ;
#25532 = VERTEX_POINT ( 'NONE', #8938 ) ;
#25533 = LINE ( 'NONE', #4159, #12821 ) ;
#25534 = DIRECTION ( 'NONE',  ( -0.000000000000000000, 1.000000000000000000, -0.000000000000000000 ) ) ;
#25535 = VERTEX_POINT ( 'NONE', #27351 ) ;
#25536 = CARTESIAN_POINT ( 'NONE',  ( -9.958038337755704461, 17.34466697471556884, 24.50000000000000000 ) ) ;
#25537 = AXIS2_PLACEMENT_3D ( 'NONE', #27211, #27063, #391 ) ;
#25538 = CIRCLE ( 'NONE', #14579, 10.00000000000003730 ) ;
#25539 = EDGE_LOOP ( 'NONE', ( #10868, #15758 ) ) ;
#25540 = B_SPLINE_CURVE_WITH_KNOTS ( 'NONE', 3,
 ( #490, #17643, #27160, #26690, #5786, #7818, #17329, #24344, #29346, #2991, #7988, #17490, #12510, #27012, #5640, #15135, #14830, #956, #22312, #10467, #5319, #12665, #24651, #3286, #19516, #24497, #22004, #14983 ),
 .UNSPECIFIED., .F., .F.,
 ( 4, 2, 2, 2, 2, 2, 2, 2, 2, 2, 2, 2, 2, 4 ),
 ( 0.06961508940978108906, 0.07265001228952157331, 0.07416747372939182237, 0.07568493516926205755, 0.08175478092874302605, 0.08782462668822399454, 0.09085954956796447879, 0.09389447244770496304, 0.09996431820718593153, 0.1029992410869264019, 0.1060341639666669000, 0.1121040097261478685, 0.1151389326058883389, 0.1181738554856288231 ),
 .UNSPECIFIED. ) ;
#25541 = DIRECTION ( 'NONE',  ( 0.000000000000000000, 0.000000000000000000, 1.000000000000000000 ) ) ;
#25542 = CARTESIAN_POINT ( 'NONE',  ( 4.390207617113956573, -7.856594496258208160, -3.621320343559650379 ) ) ;
#25543 = ORIENTED_EDGE ( 'NONE', *, *, #10503, .F. ) ;
#25544 = LINE ( 'NONE', #2281, #30280 ) ;
#25545 = SURFACE_STYLE_USAGE ( .BOTH. , #13549 ) ;
#25546 = CARTESIAN_POINT ( 'NONE',  ( 10.58893626534552190, -42.55607912659770165, -16.49999999999999645 ) ) ;
#25547 = CARTESIAN_POINT ( 'NONE',  ( -0.1973194101962248148, -20.01708124257649146, 7.500898271101006820 ) ) ;
#25548 = CARTESIAN_POINT ( 'NONE',  ( 24.75800239156184190, -7.045788922043113800, 49.25937209215325652 ) ) ;
#25549 = CARTESIAN_POINT ( 'NONE',  ( 9.033033306777456417, -0.9621688436939737077, -1.500000000000001998 ) ) ;
#25550 = CARTESIAN_POINT ( 'NONE',  ( -9.395348974764877070, -14.19336984580851713, 6.714907520933424578 ) ) ;
#25551 = CARTESIAN_POINT ( 'NONE',  ( 3.993622308618882677, 8.159193615868414184, -1.500000000000000888 ) ) ;
#25552 = ORIENTED_EDGE ( 'NONE', *, *, #3444, .T. ) ;
#25553 = CARTESIAN_POINT ( 'NONE',  ( 35.76481447503398670, -5.202797454133663457, 27.50000000000001066 ) ) ;
#25554 = ORIENTED_EDGE ( 'NONE', *, *, #25987, .T. ) ;
#25555 = ORIENTED_EDGE ( 'NONE', *, *, #23630, .T. ) ;
#25556 = AXIS2_PLACEMENT_3D ( 'NONE', #27896, #6519, #9890 ) ;
#25557 = EDGE_CURVE ( 'NONE', #8512, #20433, #23103, .T. ) ;
#25558 = DIRECTION ( 'NONE',  ( 1.000000000000000000, 0.000000000000000000, 0.000000000000000000 ) ) ;
#25559 = EDGE_CURVE ( 'NONE', #6583, #5896, #7024, .T. ) ;
#25560 = CIRCLE ( 'NONE', #28537, 0.7500000000000006661 ) ;
#25561 = CARTESIAN_POINT ( 'NONE',  ( -5.941992259041530389, 19.11559255287553682, 5.651989602109218858 ) ) ;
#25562 = ORIENTED_EDGE ( 'NONE', *, *, #9968, .F. ) ;
#25563 = B_SPLINE_CURVE_WITH_KNOTS ( 'NONE', 3,
 ( #23105, #22958, #8628, #20762, #23255, #25310, #3956, #30292, #6442, #13476, #22644, #17995, #25473, #18457, #13758, #27502, #1612, #28110 ),
 .UNSPECIFIED., .F., .F.,
 ( 4, 2, 2, 2, 2, 2, 2, 2, 4 ),
 ( 0.003174295595554301776, 0.003570702171545528901, 0.003967108747536756026, 0.004363515323527983152, 0.004759921899519211144, 0.005156328475510438270, 0.005552735051501665395, 0.005949141627492892520, 0.006345548203484119645 ),
 .UNSPECIFIED. ) ;
#25564 = EDGE_CURVE ( 'NONE', #8444, #2547, #19509, .T. ) ;
#25565 = CARTESIAN_POINT ( 'NONE',  ( -13.29453093336401537, 10.66243031773958805, 7.652108011868852699 ) ) ;
#25566 = EDGE_CURVE ( 'NONE', #606, #7300, #29961, .T. ) ;
#25567 = DIRECTION ( 'NONE',  ( 0.000000000000000000, 0.000000000000000000, 1.000000000000000000 ) ) ;
#25568 = ORIENTED_EDGE ( 'NONE', *, *, #8197, .F. ) ;
#25569 = ADVANCED_FACE ( 'NONE', ( #20759 ), #10807, .T. ) ;
#25570 = CARTESIAN_POINT ( 'NONE',  ( -7.106594496258223259, -4.390207617113929039, 21.50000000000000000 ) ) ;
#25571 = DIRECTION ( 'NONE',  ( 0.000000000000000000, 1.000000000000000000, 1.132880637372608986E-16 ) ) ;
#25572 = EDGE_LOOP ( 'NONE', ( #20610, #12280, #8718, #25268 ) ) ;
#25573 = DIRECTION ( 'NONE',  ( -0.000000000000000000, -0.000000000000000000, -1.000000000000000000 ) ) ;
#25574 = ORIENTED_EDGE ( 'NONE', *, *, #25370, .T. ) ;
#25575 = EDGE_CURVE ( 'NONE', #22258, #14561, #27500, .T. ) ;
#25576 = CARTESIAN_POINT ( 'NONE',  ( 33.42925964089141644, -11.06161099612213228, -16.55003854064094426 ) ) ;
#25577 = AXIS2_PLACEMENT_3D ( 'NONE', #16747, #26263, #12084 ) ;
#25578 = ORIENTED_EDGE ( 'NONE', *, *, #4936, .F. ) ;
#25579 = EDGE_CURVE ( 'NONE', #5755, #17047, #8489, .T. ) ;
#25580 = VERTEX_POINT ( 'NONE', #10972 ) ;
#25581 = EDGE_CURVE ( 'NONE', #20124, #6265, #3059, .T. ) ;
#25582 = AXIS2_PLACEMENT_3D ( 'NONE', #29626, #8112, #756 ) ;
#25583 = CIRCLE ( 'NONE', #26063, 2.898871837527149609 ) ;
#25584 = DIRECTION ( 'NONE',  ( 0.000000000000000000, 1.132880637372608986E-16, -1.000000000000000000 ) ) ;
#25585 = DIRECTION ( 'NONE',  ( 0.000000000000000000, -0.000000000000000000, -1.000000000000000000 ) ) ;
#25586 = CARTESIAN_POINT ( 'NONE',  ( -35.76481447503397959, 5.202797454133647470, 34.80090346875805096 ) ) ;
#25587 = DIRECTION ( 'NONE',  ( 1.000000000000000000, 0.000000000000000000, 0.000000000000000000 ) ) ;
#25588 = CARTESIAN_POINT ( 'NONE',  ( 24.73258466867332572, 33.64422401625767378, -6.500000000000000888 ) ) ;
#25589 = ORIENTED_EDGE ( 'NONE', *, *, #20028, .F. ) ;
#25590 = DIRECTION ( 'NONE',  ( -0.000000000000000000, -0.000000000000000000, 1.000000000000000000 ) ) ;
#25591 = CARTESIAN_POINT ( 'NONE',  ( 18.08817148584474310, -8.575141465928741269, 7.429667576816606278 ) ) ;
#25592 = CARTESIAN_POINT ( 'NONE',  ( -15.50193441389834881, 12.66492269502747092, 5.678370764302467677 ) ) ;
#25593 = CARTESIAN_POINT ( 'NONE',  ( 3.518760595952255876, 16.69517982287620939, 18.50655187082627862 ) ) ;
#25594 = ORIENTED_EDGE ( 'NONE', *, *, #26762, .F. ) ;
#25595 = ORIENTED_EDGE ( 'NONE', *, *, #12446, .T. ) ;
#25596 = CARTESIAN_POINT ( 'NONE',  ( 0.000000000000000000, 0.000000000000000000, -87.50000000000000000 ) ) ;
#25597 = ADVANCED_FACE ( 'NONE', ( #18138 ), #27649, .T. ) ;
#25598 = CARTESIAN_POINT ( 'NONE',  ( -4.163336342344337027E-14, 1.387778780781445676E-14, 77.49999999999998579 ) ) ;
#25599 = EDGE_CURVE ( 'NONE', #4862, #12729, #24984, .T. ) ;
#25600 = CIRCLE ( 'NONE', #17145, 15.00000000000003375 ) ;
#25601 = CARTESIAN_POINT ( 'NONE',  ( 15.28716501070585565, 12.89617714416416128, 18.54479204710283469 ) ) ;
#25602 = CARTESIAN_POINT ( 'NONE',  ( -4.775770841707818626, 16.34206821731733328, 19.96783386855779341 ) ) ;
#25603 = ADVANCED_FACE ( 'NONE', ( #26214 ), #2519, .F. ) ;
#25604 = CARTESIAN_POINT ( 'NONE',  ( 11.69640250239185342, 12.44177653179680476, 6.329955581934035180 ) ) ;
#25605 = ADVANCED_FACE ( 'NONE', ( #9080 ), #28255, .F. ) ;
#25606 = CARTESIAN_POINT ( 'NONE',  ( -26.85023221529805681, 26.31525925951064337, 27.50000000000000355 ) ) ;
#25607 = VECTOR ( 'NONE', #21907, 1000.000000000000000 ) ;
#25608 = DIRECTION ( 'NONE',  ( -1.000000000000000000, 0.000000000000000000, 0.000000000000000000 ) ) ;
#25609 = ORIENTED_EDGE ( 'NONE', *, *, #14117, .F. ) ;
#25610 = AXIS2_PLACEMENT_3D ( 'NONE', #19363, #635, #28884 ) ;
#25611 = EDGE_CURVE ( 'NONE', #22212, #15364, #2572, .T. ) ;
#25612 = CARTESIAN_POINT ( 'NONE',  ( -17.02601880987614535, 1.106972870283160493, 5.810767894563978686 ) ) ;
#25613 = DIRECTION ( 'NONE',  ( -0.000000000000000000, -0.000000000000000000, -1.000000000000000000 ) ) ;
#25614 = LINE ( 'NONE', #27953, #30402 ) ;
#25615 = EDGE_CURVE ( 'NONE', #16773, #29972, #6063, .T. ) ;
#25616 = ORIENTED_EDGE ( 'NONE', *, *, #2110, .T. ) ;
#25617 = CARTESIAN_POINT ( 'NONE',  ( -70.00000000000000000, 50.00000000000000000, 12.49999999999999112 ) ) ;
#25618 = ORIENTED_EDGE ( 'NONE', *, *, #1794, .F. ) ;
#25619 = EDGE_CURVE ( 'NONE', #25635, #13348, #11718, .T. ) ;
#25620 = DIRECTION ( 'NONE',  ( 0.000000000000000000, -1.132880637372608986E-16, 1.000000000000000000 ) ) ;
#25621 = CARTESIAN_POINT ( 'NONE',  ( -1.046997975306281248, 44.06280042554938348, -16.50000000000000355 ) ) ;
#25622 = ORIENTED_EDGE ( 'NONE', *, *, #11710, .F. ) ;
#25623 = CARTESIAN_POINT ( 'NONE',  ( -23.11204207310937875, -35.56592875159903855, -11.49994540249954156 ) ) ;
#25624 = CARTESIAN_POINT ( 'NONE',  ( 9.906380082428048794, 49.01032848149721133, -43.72596795826983396 ) ) ;
#25625 = FACE_OUTER_BOUND ( 'NONE', #26960, .T. ) ;
#25626 = CARTESIAN_POINT ( 'NONE',  ( -23.91679456219654298, -22.99653376284463491, -16.50001200000000168 ) ) ;
#25627 = VECTOR ( 'NONE', #20074, 1000.000000000000000 ) ;
#25628 = DIRECTION ( 'NONE',  ( 0.000000000000000000, -1.000000000000000000, 0.000000000000000000 ) ) ;
#25629 = CARTESIAN_POINT ( 'NONE',  ( -16.93131609043279795, 1.909234121842571019, 5.676815824193228721 ) ) ;
#25630 = EDGE_LOOP ( 'NONE', ( #23040, #30538, #19801, #2559 ) ) ;
#25631 = EDGE_CURVE ( 'NONE', #8392, #4264, #19449, .T. ) ;
#25632 = EDGE_CURVE ( 'NONE', #12729, #14399, #23876, .T. ) ;
#25633 = CARTESIAN_POINT ( 'NONE',  ( -40.00000000000002842, 90.00000000000001421, 47.50000000000014921 ) ) ;
#25634 = CARTESIAN_POINT ( 'NONE',  ( -26.36764545593177544, -31.31467416275353344, -1.500000000000000000 ) ) ;
#25635 = VERTEX_POINT ( 'NONE', #16397 ) ;
#25636 = FACE_OUTER_BOUND ( 'NONE', #26750, .T. ) ;
#25637 = DIRECTION ( 'NONE',  ( 0.000000000000000000, 0.000000000000000000, 1.000000000000000000 ) ) ;
#25638 = CARTESIAN_POINT ( 'NONE',  ( -23.96732207938974213, -33.98584080153308662, -1.500000000000000000 ) ) ;
#25639 = LINE ( 'NONE', #13930, #23532 ) ;
#25640 = ORIENTED_EDGE ( 'NONE', *, *, #23214, .T. ) ;
#25641 = CARTESIAN_POINT ( 'NONE',  ( -4.163336342344337027E-14, 1.387778780781445676E-14, 24.50000000000000000 ) ) ;
#25642 = FACE_OUTER_BOUND ( 'NONE', #28889, .T. ) ;
#25643 = CARTESIAN_POINT ( 'NONE',  ( 10.21997447646774937, -36.08534693423421658, 37.50000000003055334 ) ) ;
#25644 = CYLINDRICAL_SURFACE ( 'NONE', #7609, 22.49999999999996447 ) ;
#25645 = ORIENTED_EDGE ( 'NONE', *, *, #4473, .T. ) ;
#25646 = ORIENTED_EDGE ( 'NONE', *, *, #24991, .F. ) ;
#25647 = CARTESIAN_POINT ( 'NONE',  ( -39.00000000000000000, -5.563236990218529243, -1.500000000000000000 ) ) ;
#25648 = DIRECTION ( 'NONE',  ( 0.000000000000000000, 1.000000000000000000, 0.000000000000000000 ) ) ;
#25649 = AXIS2_PLACEMENT_3D ( 'NONE', #22181, #19539, #28907 ) ;
#25650 = ORIENTED_EDGE ( 'NONE', *, *, #19093, .T. ) ;
#25651 = DIRECTION ( 'NONE',  ( 0.000000000000000000, 0.000000000000000000, -1.000000000000000000 ) ) ;
#25652 = ORIENTED_EDGE ( 'NONE', *, *, #29014, .F. ) ;
#25653 = CARTESIAN_POINT ( 'NONE',  ( -25.18096005886327760, -6.640581704039635547, 44.71664046397099668 ) ) ;
#25654 = CARTESIAN_POINT ( 'NONE',  ( -8.163758309741957930, -14.97879848885351706, 5.749491821935610147 ) ) ;
#25655 = LINE ( 'NONE', #520, #5380 ) ;
#25656 = CARTESIAN_POINT ( 'NONE',  ( -3.221450758838616757, 1.621276839356792454, 1.500000000000000000 ) ) ;
#25657 = VERTEX_POINT ( 'NONE', #9385 ) ;
#25658 = CARTESIAN_POINT ( 'NONE',  ( -24.35970437652574105, 13.37404834226503247, 47.21042702067971675 ) ) ;
#25659 = LINE ( 'NONE', #4279, #21316 ) ;
#25660 = DIRECTION ( 'NONE',  ( 1.000000000000000000, 0.000000000000000000, 0.000000000000000000 ) ) ;
#25661 = ADVANCED_FACE ( 'NONE', ( #20916 ), #25913, .F. ) ;
#25662 = CARTESIAN_POINT ( 'NONE',  ( -44.20831430623121605, 69.15340090750629543, 13.40607705188479670 ) ) ;
#25663 = DIRECTION ( 'NONE',  ( 0.000000000000000000, 0.000000000000000000, -1.000000000000000000 ) ) ;
#25664 = CARTESIAN_POINT ( 'NONE',  ( 25.48568755041062417, 12.36160011285428872, 24.50000000000000000 ) ) ;
#25665 = CARTESIAN_POINT ( 'NONE',  ( -12.79825419741609771, 11.22575876276140505, 19.85270094495842130 ) ) ;
#25666 = AXIS2_PLACEMENT_3D ( 'NONE', #5193, #14856, #29671 ) ;
#25667 = CARTESIAN_POINT ( 'NONE',  ( -47.00000000000000000, 90.00000000000001421, 52.49999999999999289 ) ) ;
#25668 = DIRECTION ( 'NONE',  ( 0.000000000000000000, -0.000000000000000000, -1.000000000000000000 ) ) ;
#25669 = CARTESIAN_POINT ( 'NONE',  ( -18.15888143814678557, -8.424936462863952258, 20.32842677360128292 ) ) ;
#25670 = DIRECTION ( 'NONE',  ( -1.000000000000000000, -0.000000000000000000, -0.000000000000000000 ) ) ;
#25671 = ORIENTED_EDGE ( 'NONE', *, *, #16974, .T. ) ;
#25672 = VERTEX_POINT ( 'NONE', #18903 ) ;
#25673 = CARTESIAN_POINT ( 'NONE',  ( -0.7220001660362882490, -9.454746441592959627, 1.500000000000001332 ) ) ;
#25674 = CARTESIAN_POINT ( 'NONE',  ( 19.64114023396309960, -37.13592150529014191, -1.500000000000000000 ) ) ;
#25675 = DIRECTION ( 'NONE',  ( -0.000000000000000000, -0.000000000000000000, -1.000000000000000000 ) ) ;
#25676 = ORIENTED_EDGE ( 'NONE', *, *, #12657, .F. ) ;
#25677 = CARTESIAN_POINT ( 'NONE',  ( 0.000000000000000000, 0.000000000000000000, 0.000000000000000000 ) ) ;
#25678 = CARTESIAN_POINT ( 'NONE',  ( -6.507549961782360448, 15.78987431823413523, 19.28454053338349183 ) ) ;
#25679 = CARTESIAN_POINT ( 'NONE',  ( 5.908622583341371026, 19.12614776545568418, 5.862424720655265098 ) ) ;
#25680 = EDGE_LOOP ( 'NONE', ( #11911, #4660, #22503, #10062, #5124 ) ) ;
#25681 = CARTESIAN_POINT ( 'NONE',  ( -16.95096719779282424, 1.761153487549136587, 5.657991946698900598 ) ) ;
#25682 = DIRECTION ( 'NONE',  ( 1.000000000000000000, 0.000000000000000000, 0.000000000000000000 ) ) ;
#25683 = CARTESIAN_POINT ( 'NONE',  ( -8.275208547106167600, -43.16521806348789880, -16.50000000000000000 ) ) ;
#25684 = DIRECTION ( 'NONE',  ( -1.000000000000000000, 0.000000000000000000, 0.000000000000000000 ) ) ;
#25685 = VERTEX_POINT ( 'NONE', #7037 ) ;
#25686 = DIRECTION ( 'NONE',  ( -0.9329908884337534403, 0.3598999890241668664, 0.000000000000000000 ) ) ;
#25687 = AXIS2_PLACEMENT_3D ( 'NONE', #24662, #5494, #24507 ) ;
#25688 = CARTESIAN_POINT ( 'NONE',  ( -14.80112376882104819, -8.505769479164674962, 7.269896094239229889 ) ) ;
#25689 = DIRECTION ( 'NONE',  ( 1.000000000000000000, 0.000000000000000000, 0.000000000000000000 ) ) ;
#25690 = EDGE_LOOP ( 'NONE', ( #4723, #8252, #6543, #398 ) ) ;
#25691 = LINE ( 'NONE', #18218, #2380 ) ;
#25692 = FACE_OUTER_BOUND ( 'NONE', #11616, .T. ) ;
#25693 = CARTESIAN_POINT ( 'NONE',  ( -49.99999999999955236, -4.926614671774132148E-13, 65.49999999999998579 ) ) ;
#25694 = CARTESIAN_POINT ( 'NONE',  ( -0.1834311997418870965, -17.02123387943971977, 6.974106381145714018 ) ) ;
#25695 = EDGE_CURVE ( 'NONE', #29313, #1784, #15558, .T. ) ;
#25696 = VECTOR ( 'NONE', #5367, 1000.000000000000000 ) ;
#25697 = DIRECTION ( 'NONE',  ( 0.000000000000000000, 0.000000000000000000, 1.000000000000000000 ) ) ;
#25698 = CARTESIAN_POINT ( 'NONE',  ( 14.83584055149749759, 17.84153987719500734, 1.500000000000000000 ) ) ;
#25699 = CARTESIAN_POINT ( 'NONE',  ( -17.06612199394662710, 0.6423840055640230862, 19.47783254395485031 ) ) ;
#25700 = DIRECTION ( 'NONE',  ( 1.000000000000000000, 0.000000000000000000, 0.000000000000000000 ) ) ;
#25701 = VERTEX_POINT ( 'NONE', #26683 ) ;
#25702 = FACE_OUTER_BOUND ( 'NONE', #28735, .T. ) ;
#25703 = CARTESIAN_POINT ( 'NONE',  ( 36.00000000000001421, 2.601438916704194249, 34.80090346875809360 ) ) ;
#25704 = ORIENTED_EDGE ( 'NONE', *, *, #23860, .F. ) ;
#25705 = VERTEX_POINT ( 'NONE', #14824 ) ;
#25706 = VECTOR ( 'NONE', #17427, 1000.000000000000000 ) ;
#25707 = CARTESIAN_POINT ( 'NONE',  ( -47.57918908651176793, 69.85400074660304881, 59.03148159615753343 ) ) ;
#25708 = EDGE_LOOP ( 'NONE', ( #123, #17244, #4230, #24066 ) ) ;
#25709 = CIRCLE ( 'NONE', #18715, 0.7500000000000002220 ) ;
#25710 = FACE_OUTER_BOUND ( 'NONE', #10707, .T. ) ;
#25711 = DIRECTION ( 'NONE',  ( -1.000000000000000000, 0.000000000000000000, 0.000000000000000000 ) ) ;
#25712 = ORIENTED_EDGE ( 'NONE', *, *, #29471, .T. ) ;
#25713 = CARTESIAN_POINT ( 'NONE',  ( -15.73693831436014179, 12.34332084443492938, 18.54958172136248606 ) ) ;
#25714 = AXIS2_PLACEMENT_3D ( 'NONE', #11199, #30383, #18992 ) ;
#25715 = DIRECTION ( 'NONE',  ( -0.000000000000000000, -0.000000000000000000, 1.000000000000000000 ) ) ;
#25716 = ORIENTED_EDGE ( 'NONE', *, *, #12602, .F. ) ;
#25717 = CARTESIAN_POINT ( 'NONE',  ( 11.21147646446735102, 30.29926891764210595, 1.500000000000000000 ) ) ;
#25718 = MECHANICAL_DESIGN_GEOMETRIC_PRESENTATION_REPRESENTATION (  '', ( #26725 ), #12794 ) ;
#25719 = ORIENTED_EDGE ( 'NONE', *, *, #2700, .F. ) ;
#25720 = LINE ( 'NONE', #3698, #30857 ) ;
#25721 = ORIENTED_EDGE ( 'NONE', *, *, #21194, .F. ) ;
#25722 = ORIENTED_EDGE ( 'NONE', *, *, #12282, .F. ) ;
#25723 = EDGE_CURVE ( 'NONE', #12979, #23733, #485, .T. ) ;
#25724 = AXIS2_PLACEMENT_3D ( 'NONE', #26387, #24494, #14979 ) ;
#25725 = AXIS2_PLACEMENT_3D ( 'NONE', #27859, #18497, #2095 ) ;
#25726 = DIRECTION ( 'NONE',  ( -0.000000000000000000, 1.000000000000000000, -0.000000000000000000 ) ) ;
#25727 = CARTESIAN_POINT ( 'NONE',  ( 0.2758680007052473626, -17.03033689273113183, 18.47056384035244037 ) ) ;
#25728 = ADVANCED_FACE ( 'NONE', ( #10891 ), #26854, .F. ) ;
#25729 = CARTESIAN_POINT ( 'NONE',  ( -34.83396020575241891, -10.30249279383514960, 27.50000000000001066 ) ) ;
#25730 = CARTESIAN_POINT ( 'NONE',  ( 1.743352590885965281, -16.98718212385403348, 19.02573955821369367 ) ) ;
#25731 = CARTESIAN_POINT ( 'NONE',  ( 19.79578860058543910, 2.975267875541937723, 18.36582235739946611 ) ) ;
#25732 = ORIENTED_EDGE ( 'NONE', *, *, #4434, .F. ) ;
#25733 = ADVANCED_FACE ( 'NONE', ( #24170 ), #5008, .F. ) ;
#25734 = CARTESIAN_POINT ( 'NONE',  ( 11.11463893384431323, -16.64861865631835514, 7.652108011868850035 ) ) ;
#25735 = DIRECTION ( 'NONE',  ( 1.000000000000000000, 0.000000000000000000, 0.000000000000000000 ) ) ;
#25736 = DIRECTION ( 'NONE',  ( 1.000000000000000000, 0.000000000000000000, 0.000000000000000000 ) ) ;
#25737 = CARTESIAN_POINT ( 'NONE',  ( 3.898220458062930049, 16.59828442330440978, 18.35718225375110180 ) ) ;
#25738 = VERTEX_POINT ( 'NONE', #24339 ) ;
#25739 = ORIENTED_EDGE ( 'NONE', *, *, #14502, .T. ) ;
#25740 = DIRECTION ( 'NONE',  ( 0.000000000000000000, 0.000000000000000000, 1.000000000000000000 ) ) ;
#25741 = CARTESIAN_POINT ( 'NONE',  ( 33.13218612630368654, -7.028748154183637631, -1.942616967526160643 ) ) ;
#25742 = DIRECTION ( 'NONE',  ( -0.000000000000000000, 0.000000000000000000, -1.000000000000000000 ) ) ;
#25744 = EDGE_CURVE ( 'NONE', #13119, #4772, #23481, .T. ) ;
#25743 = CIRCLE ( 'NONE', #16282, 1.447898107987198646 ) ;
#25745 = CARTESIAN_POINT ( 'NONE',  ( 36.00000000000063238, 1.782879839924971010, 34.75735931288080849 ) ) ;
#25747 = EDGE_CURVE ( 'NONE', #18622, #11660, #17011, .T. ) ;
#25746 = AXIS2_PLACEMENT_3D ( 'NONE', #20813, #15990, #13513 ) ;
#25748 = ITEM_DEFINED_TRANSFORMATION ( 'NONE', 'NONE', #19857,  #7396 ) ;
#25749 = CARTESIAN_POINT ( 'NONE',  ( 23.59634279088906439, -12.86962927293162906, 48.12226976371609766 ) ) ;
#25750 = ORIENTED_EDGE ( 'NONE', *, *, #455, .F. ) ;
#25751 = AXIS2_PLACEMENT_3D ( 'NONE', #25925, #17023, #7048 ) ;
#25752 = AXIS2_PLACEMENT_3D ( 'NONE', #30271, #27941, #6568 ) ;
#25753 = CARTESIAN_POINT ( 'NONE',  ( -16.99143801116385433, 1.432169416036910725, 7.627891251804737927 ) ) ;
#25754 = CARTESIAN_POINT ( 'NONE',  ( 14.20332585465777520, 14.08077620357339299, 19.61564845152805603 ) ) ;
#25755 = CARTESIAN_POINT ( 'NONE',  ( 30.53339558441486190, 7.800891647352844238, 43.48653168448679196 ) ) ;
#25756 = ORIENTED_EDGE ( 'NONE', *, *, #15723, .F. ) ;
#25757 = DIRECTION ( 'NONE',  ( 0.000000000000000000, 0.000000000000000000, -1.000000000000000000 ) ) ;
#25758 = ORIENTED_EDGE ( 'NONE', *, *, #29583, .F. ) ;
#25759 = CARTESIAN_POINT ( 'NONE',  ( 18.44211820063743446, -7.784504718833763270, 5.678370764302467677 ) ) ;
#25760 = CARTESIAN_POINT ( 'NONE',  ( -7.281713232848989747, 43.36492703356076817, -16.49999999999999645 ) ) ;
#25761 = AXIS2_PLACEMENT_3D ( 'NONE', #28392, #16526, #26192 ) ;
#25762 = ORIENTED_EDGE ( 'NONE', *, *, #1572, .F. ) ;
#25763 = CARTESIAN_POINT ( 'NONE',  ( 21.15904228388716746, -31.96044797056314124, 27.50000000000000355 ) ) ;
#25764 = EDGE_CURVE ( 'NONE', #27309, #14218, #5085, .T. ) ;
#25765 = CLOSED_SHELL ( 'NONE', ( #765, #25785, #14883, #20758, #25231, #449, #24526, #5988, #18199, #5737, #28659, #26554, #1720, #1999, #3504, #25603, #5631, #30173, #28835, #28478, #13436, #2934, #3668, #20214, #3887, #25962, #6348, #24249, #16625, #1950, #8487, #7830, #25442, #14275, #1214, #5352, #29076, #1762, #5633, #2628, #26675, #25195, #22152, #1451, #9929, #8069, #12075, #26328, #23312, #28452, #16031, #12623, #22516, #29796, #6545, #13392, #25958, #5026, #15835, #20096, #4397, #22812, #22514, #6677, #7318, #15102, #14541, #16022, #27922, #6011, #9697, #2718, #16856, #28667, #5991, #28098, #5724, #1159, #22062, #19308, #12454, #795, #28630, #11686, #14002, #9999, #10563, #25843, #6368, #3279, #14196, #26157, #24799, #30065, #28516, #28644, #30682, #23099, #1228, #22335, #13744, #16191, #13778, #1925, #5001, #6724, #20833, #1944, #11441, #27482, #8503, #20601 ) ) ;
#25766 = DIRECTION ( 'NONE',  ( 1.000000000000000000, 0.000000000000000000, 0.000000000000000000 ) ) ;
#25767 = EDGE_CURVE ( 'NONE', #1665, #17197, #1104, .T. ) ;
#25768 = DIRECTION ( 'NONE',  ( 1.000000000000000000, 0.000000000000000000, 0.000000000000000000 ) ) ;
#25769 = AXIS2_PLACEMENT_3D ( 'NONE', #2161, #9339, #8893 ) ;
#25770 = CARTESIAN_POINT ( 'NONE',  ( -6.413028646417897605, 15.82458379172921603, 19.79423548914561692 ) ) ;
#25771 = CIRCLE ( 'NONE', #4347, 7.500000000000013323 ) ;
#25772 = DIRECTION ( 'NONE',  ( -0.000000000000000000, 0.000000000000000000, 1.000000000000000000 ) ) ;
#25773 = EDGE_CURVE ( 'NONE', #27607, #3383, #6082, .T. ) ;
#25774 = DIRECTION ( 'NONE',  ( 1.000000000000000000, 0.000000000000000000, 0.000000000000000000 ) ) ;
#25775 = ORIENTED_EDGE ( 'NONE', *, *, #25807, .T. ) ;
#25776 = ADVANCED_FACE ( 'NONE', ( #2824 ), #12346, .F. ) ;
#25777 = VECTOR ( 'NONE', #755, 1000.000000000000227 ) ;
#25778 = DIRECTION ( 'NONE',  ( 0.000000000000000000, 1.000000000000000000, 0.000000000000000000 ) ) ;
#25779 = CARTESIAN_POINT ( 'NONE',  ( -12.24063095261064227, 4.490763173670005770, 1.500000000000001332 ) ) ;
#25780 = EDGE_LOOP ( 'NONE', ( #22416, #12875, #7092, #20839 ) ) ;
#25781 = EDGE_CURVE ( 'NONE', #17742, #1033, #17033, .T. ) ;
#25782 = CARTESIAN_POINT ( 'NONE',  ( -3.515970705488605130, 17.06554576617236307, -1.500000000000000000 ) ) ;
#25783 = CARTESIAN_POINT ( 'NONE',  ( 49.99999999999997868, 209.2686044187655909, -34.50000000000000000 ) ) ;
#25784 = CIRCLE ( 'NONE', #2376, 0.7499999999999997780 ) ;
#25785 = ADVANCED_FACE ( 'NONE', ( #7662 ), #28880, .F. ) ;
#25786 = SURFACE_STYLE_FILL_AREA ( #28126 ) ;
#25787 = AXIS2_PLACEMENT_3D ( 'NONE', #6449, #25772, #30447 ) ;
#25788 = CARTESIAN_POINT ( 'NONE',  ( 33.42925964089141644, 11.06161099612213405, -16.55003854064094426 ) ) ;
#25789 = AXIS2_PLACEMENT_3D ( 'NONE', #14247, #1957, #9277 ) ;
#25790 = VERTEX_POINT ( 'NONE', #628 ) ;
#25791 = DIRECTION ( 'NONE',  ( -1.000000000000000000, -0.000000000000000000, -0.000000000000000000 ) ) ;
#25792 = EDGE_CURVE ( 'NONE', #28054, #19044, #3595, .T. ) ;
#25793 = CARTESIAN_POINT ( 'NONE',  ( 49.99999999999998579, 50.00000000000000000, 12.49999999999999112 ) ) ;
#25794 = CARTESIAN_POINT ( 'NONE',  ( 26.15871596101562702, -26.98401179872733735, 37.49999999983522514 ) ) ;
#25795 = FACE_BOUND ( 'NONE', #694, .T. ) ;
#25796 = ORIENTED_EDGE ( 'NONE', *, *, #17216, .F. ) ;
#25797 = DIRECTION ( 'NONE',  ( -0.000000000000000000, 0.000000000000000000, -1.000000000000000000 ) ) ;
#25798 = AXIS2_PLACEMENT_3D ( 'NONE', #13691, #23023, #16329 ) ;
#25799 = CARTESIAN_POINT ( 'NONE',  ( -9.454746441592954298, 0.7220001660363423168, 1.500000000000001332 ) ) ;
#25800 = LINE ( 'NONE', #28138, #30852 ) ;
#25801 = AXIS2_PLACEMENT_3D ( 'NONE', #20765, #2052, #20477 ) ;
#25802 = ORIENTED_EDGE ( 'NONE', *, *, #42, .T. ) ;
#25803 = DIRECTION ( 'NONE',  ( 1.000000000000000000, 0.000000000000000000, 0.000000000000000000 ) ) ;
#25804 = ORIENTED_EDGE ( 'NONE', *, *, #4774, .F. ) ;
#25805 = CARTESIAN_POINT ( 'NONE',  ( -30.50204315964898427, -15.53056155674291183, 40.77182279853386859 ) ) ;
#25806 = EDGE_CURVE ( 'NONE', #23863, #15313, #21007, .T. ) ;
#25807 = EDGE_CURVE ( 'NONE', #28109, #28104, #17458, .T. ) ;
#25808 = CARTESIAN_POINT ( 'NONE',  ( -7.931808866138727154, -15.11281102451792080, 7.366751648393900176 ) ) ;
#25809 = CIRCLE ( 'NONE', #12365, 9.084132297865673777 ) ;
#25810 = CARTESIAN_POINT ( 'NONE',  ( 29.81954908927654202, -15.48017614753372584, 41.40177460054268721 ) ) ;
#25811 = CARTESIAN_POINT ( 'NONE',  ( 1.709141304117141047, -16.98942507101831012, 18.92976555901915603 ) ) ;
#25812 = EDGE_LOOP ( 'NONE', ( #20181, #10779 ) ) ;
#25813 = CARTESIAN_POINT ( 'NONE',  ( 18.57491549710359635, -7.414944001931016437, 7.454606537396340826 ) ) ;
#25814 = CARTESIAN_POINT ( 'NONE',  ( 12.93167884983506610, 11.07185515090903749, 18.83976166372256245 ) ) ;
#25815 = LINE ( 'NONE', #13957, #5279 ) ;
#25816 = LINE ( 'NONE', #5744, #12647 ) ;
#25817 = ORIENTED_EDGE ( 'NONE', *, *, #26386, .T. ) ;
#25818 = CARTESIAN_POINT ( 'NONE',  ( -49.44509678728922353, 69.99255420029007269, 19.19783229408952252 ) ) ;
#25819 = VECTOR ( 'NONE', #988, 1000.000000000000000 ) ;
#25820 = CARTESIAN_POINT ( 'NONE',  ( -15.37673962019493956, -7.325595981656340960, 18.47056384035244747 ) ) ;
#25821 = FACE_OUTER_BOUND ( 'NONE', #2788, .T. ) ;
#25822 = DIRECTION ( 'NONE',  ( -0.000000000000000000, 1.132880637372608986E-16, -1.000000000000000000 ) ) ;
#25823 = CARTESIAN_POINT ( 'NONE',  ( -4.163336342344337027E-14, 1.387778780781445676E-14, 24.50000000000000000 ) ) ;
#25824 = FACE_OUTER_BOUND ( 'NONE', #9059, .T. ) ;
#25825 = CARTESIAN_POINT ( 'NONE',  ( 9.755266892098159559, -13.97392213622798707, 5.651492010659114662 ) ) ;
#25826 = CARTESIAN_POINT ( 'NONE',  ( 69.99999999999998579, -70.00000000000000000, 12.49999999999999112 ) ) ;
#25827 = VERTEX_POINT ( 'NONE', #22883 ) ;
#25828 = VERTEX_POINT ( 'NONE', #18062 ) ;
#25829 = LINE ( 'NONE', #11334, #27418 ) ;
#25830 = CARTESIAN_POINT ( 'NONE',  ( -8.097046320181942036, -15.01856385382801129, 5.759928666072747561 ) ) ;
#25831 = FACE_OUTER_BOUND ( 'NONE', #3570, .T. ) ;
#25832 = ORIENTED_EDGE ( 'NONE', *, *, #11452, .F. ) ;
#25833 = DIRECTION ( 'NONE',  ( 0.000000000000000000, 0.000000000000000000, -1.000000000000000000 ) ) ;
#25834 = VECTOR ( 'NONE', #25513, 1000.000000000000000 ) ;
#25835 = CARTESIAN_POINT ( 'NONE',  ( -6.384540597184203747, 15.83495921351375735, 19.85459532544248162 ) ) ;
#25836 = AXIS2_PLACEMENT_3D ( 'NONE', #14290, #28505, #14000 ) ;
#25837 = CIRCLE ( 'NONE', #12390, 20.00000000000000000 ) ;
#25838 = CARTESIAN_POINT ( 'NONE',  ( 5.413395986729065079, 19.27227163692344902, 7.652108011868850035 ) ) ;
#25839 = EDGE_CURVE ( 'NONE', #1882, #30491, #12265, .T. ) ;
#25840 = VERTEX_POINT ( 'NONE', #27889 ) ;
#25841 = CARTESIAN_POINT ( 'NONE',  ( -16.95590486909633654, 1.723587065725475265, 5.653912893140659257 ) ) ;
#25842 = FACE_OUTER_BOUND ( 'NONE', #26369, .T. ) ;
#25843 = ADVANCED_FACE ( 'NONE', ( #11191 ), #15873, .F. ) ;
#25844 = VECTOR ( 'NONE', #13529, 1000.000000000000000 ) ;
#25845 = DIRECTION ( 'NONE',  ( 0.000000000000000000, 1.000000000000000000, 0.000000000000000000 ) ) ;
#25846 = CARTESIAN_POINT ( 'NONE',  ( -37.63189979596968016, 11.23836474745404423, 34.94552664686906951 ) ) ;
#25847 = ORIENTED_EDGE ( 'NONE', *, *, #21943, .F. ) ;
#25848 = CARTESIAN_POINT ( 'NONE',  ( 0.000000000000000000, 0.000000000000000000, -1.500000000000000000 ) ) ;
#25849 = CARTESIAN_POINT ( 'NONE',  ( -14.79998981352115983, -8.507912210563924660, 6.037360021877317351 ) ) ;
#25850 = CARTESIAN_POINT ( 'NONE',  ( -7.974144905643821168, -5.130938270761581599, 21.50000000000000000 ) ) ;
#25851 = ORIENTED_EDGE ( 'NONE', *, *, #20636, .T. ) ;
#25852 = CARTESIAN_POINT ( 'NONE',  ( 6.812559277181973627, -5.881244434206257310, 21.50000000000000000 ) ) ;
#25853 = CARTESIAN_POINT ( 'NONE',  ( 0.000000000000000000, 0.000000000000000000, -87.50000000000000000 ) ) ;
#25854 = DIRECTION ( 'NONE',  ( -1.000000000000000000, 0.000000000000000000, 0.000000000000000000 ) ) ;
#25855 = FACE_OUTER_BOUND ( 'NONE', #28841, .T. ) ;
#25856 = CIRCLE ( 'NONE', #15910, 0.7500000000000011102 ) ;
#25857 = FACE_OUTER_BOUND ( 'NONE', #21675, .T. ) ;
#25858 = CARTESIAN_POINT ( 'NONE',  ( 7.856594496258195726, 4.390207617113981442, 21.50000000000000000 ) ) ;
#25859 = CARTESIAN_POINT ( 'NONE',  ( -19.89984252009588062, 2.172142757504853972, 20.29915277494337644 ) ) ;
#25860 = CARTESIAN_POINT ( 'NONE',  ( 5.278755796068665518, 7.392982946727100213, 21.50000000000000000 ) ) ;
#25861 = ORIENTED_EDGE ( 'NONE', *, *, #8693, .T. ) ;
#25862 = CARTESIAN_POINT ( 'NONE',  ( 10.13630142350640462, -13.71646693216190371, 20.29915277494337644 ) ) ;
#25863 = VECTOR ( 'NONE', #28551, 1000.000000000000000 ) ;
#25864 = CARTESIAN_POINT ( 'NONE',  ( 4.677126025380971441, 39.24912351428226742, 27.50000000000000355 ) ) ;
#25865 = ORIENTED_EDGE ( 'NONE', *, *, #14712, .T. ) ;
#25866 = VERTEX_POINT ( 'NONE', #29921 ) ;
#25867 = CARTESIAN_POINT ( 'NONE',  ( -47.98494098007435582, 69.89927657657921145, 58.52868780040671481 ) ) ;
#25868 = ORIENTED_EDGE ( 'NONE', *, *, #10687, .F. ) ;
#25869 = TOROIDAL_SURFACE ( 'NONE', #12429, 47.00000000000000000, 3.000000000000000000 ) ;
#25870 = CYLINDRICAL_SURFACE ( 'NONE', #12171, 2.000000000000001776 ) ;
#25871 =( NAMED_UNIT ( * ) SI_UNIT ( $, .STERADIAN. ) SOLID_ANGLE_UNIT ( ) );
#25872 = EDGE_LOOP ( 'NONE', ( #14590, #1922 ) ) ;
#25873 = DIRECTION ( 'NONE',  ( 0.000000000000000000, 1.000000000000000000, 1.193512090021232842E-16 ) ) ;
#25874 = EDGE_CURVE ( 'NONE', #24056, #22039, #18540, .T. ) ;
#25875 = VECTOR ( 'NONE', #19263, 1000.000000000000000 ) ;
#25876 = CARTESIAN_POINT ( 'NONE',  ( -0.9370274472974918778, -8.840471615930066918, 21.50000000000000000 ) ) ;
#25877 = ORIENTED_EDGE ( 'NONE', *, *, #26976, .F. ) ;
#25878 = CARTESIAN_POINT ( 'NONE',  ( -12.50000000000000000, 0.000000000000000000, -87.50000000000000000 ) ) ;
#25879 = CYLINDRICAL_SURFACE ( 'NONE', #3475, 37.60050224823048381 ) ;
#25880 = ORIENTED_EDGE ( 'NONE', *, *, #12606, .F. ) ;
#25881 = AXIS2_PLACEMENT_3D ( 'NONE', #6392, #6230, #25711 ) ;
#25882 = ORIENTED_EDGE ( 'NONE', *, *, #19668, .F. ) ;
#25883 = FACE_BOUND ( 'NONE', #14801, .T. ) ;
#25884 = CARTESIAN_POINT ( 'NONE',  ( -17.59500444164590149, -9.508866521682284301, 6.919864475265789849 ) ) ;
#25885 = CIRCLE ( 'NONE', #29391, 0.7500000000000006661 ) ;
#25886 = CARTESIAN_POINT ( 'NONE',  ( -14.76516729830842500, -8.573104839187553949, 19.85459532544248162 ) ) ;
#25887 = CARTESIAN_POINT ( 'NONE',  ( 0.7836604620899298990, -17.02735026737547841, 18.34798005863078885 ) ) ;
#25888 = CARTESIAN_POINT ( 'NONE',  ( 16.86202325244926570, 2.345734461008496474, 18.80699882434806369 ) ) ;
#25889 = ORIENTED_EDGE ( 'NONE', *, *, #953, .T. ) ;
#25890 = CARTESIAN_POINT ( 'NONE',  ( -19.78695419347077333, 3.033347482080938740, 18.49267272388512140 ) ) ;
#25891 = CARTESIAN_POINT ( 'NONE',  ( 8.029152834601454458, -38.52032120320185271, 34.49999999999999289 ) ) ;
#25892 = DIRECTION ( 'NONE',  ( 1.000000000000000000, 0.000000000000000000, 0.000000000000000000 ) ) ;
#25893 = ORIENTED_EDGE ( 'NONE', *, *, #16744, .F. ) ;
#25894 = ORIENTED_EDGE ( 'NONE', *, *, #15887, .T. ) ;
#25895 = CARTESIAN_POINT ( 'NONE',  ( -77.99999999999998579, -42.49999999999998579, 1.500000000000001110 ) ) ;
#25896 = PLANE ( 'NONE',  #2662 ) ;
#25897 = CARTESIAN_POINT ( 'NONE',  ( -4.940218127011004157, 16.29708528951388402, 18.55820869691756769 ) ) ;
#25898 = CARTESIAN_POINT ( 'NONE',  ( -23.07950435457351190, 11.50806656539842798, 44.96784366550151191 ) ) ;
#25899 = CIRCLE ( 'NONE', #2011, 0.7500000000000003331 ) ;
#25900 = CARTESIAN_POINT ( 'NONE',  ( -70.00000000000000000, 65.00000000000000000, 57.49999999999999289 ) ) ;
#25901 = FACE_OUTER_BOUND ( 'NONE', #23924, .T. ) ;
#25902 = ORIENTED_EDGE ( 'NONE', *, *, #22130, .T. ) ;
#25903 = AXIS2_PLACEMENT_3D ( 'NONE', #6495, #14107, #13824 ) ;
#25904 = CARTESIAN_POINT ( 'NONE',  ( -17.06249589246194276, 0.6902251470929409161, 6.341840715582230281 ) ) ;
#25905 = CYLINDRICAL_SURFACE ( 'NONE', #30633, 0.6002263538043648428 ) ;
#25906 = CARTESIAN_POINT ( 'NONE',  ( 19.83281414115336005, 2.582324728781443923, 20.14992337338002670 ) ) ;
#25907 = EDGE_LOOP ( 'NONE', ( #14645, #1678, #23168, #26379 ) ) ;
#25908 = CARTESIAN_POINT ( 'NONE',  ( 0.000000000000000000, 1.699320956058915452E-16, -1.500000000000001776 ) ) ;
#25909 = EDGE_CURVE ( 'NONE', #17261, #7591, #7583, .T. ) ;
#25910 = ORIENTED_EDGE ( 'NONE', *, *, #3100, .T. ) ;
#25911 = CARTESIAN_POINT ( 'NONE',  ( -50.00000000000000000, 50.00000000000000000, 12.49999999999999112 ) ) ;
#25912 = ADVANCED_FACE ( 'NONE', ( #4020 ), #6204, .F. ) ;
#25913 = CYLINDRICAL_SURFACE ( 'NONE', #9050, 0.7499999999999988898 ) ;
#25914 = ORIENTED_EDGE ( 'NONE', *, *, #8874, .T. ) ;
#25915 = CARTESIAN_POINT ( 'NONE',  ( 21.62415194650660766, 31.60332031111338225, 27.50000000000000000 ) ) ;
#25916 = CARTESIAN_POINT ( 'NONE',  ( 77.99999999999998579, 42.50000000000000711, 24.50000000000000000 ) ) ;
#25917 = CARTESIAN_POINT ( 'NONE',  ( -7.548823014270604759, 5.738360882150026931, 1.500000000000001332 ) ) ;
#25918 = CARTESIAN_POINT ( 'NONE',  ( -18.45576848551221971, -7.706141034055812966, 6.518927109361836614 ) ) ;
#25919 = CIRCLE ( 'NONE', #12490, 4.999999999999997335 ) ;
#25920 = CARTESIAN_POINT ( 'NONE',  ( -3.469446951953614189E-15, -30.50000000000000711, 24.50000000000000000 ) ) ;
#25921 = CARTESIAN_POINT ( 'NONE',  ( -4.608906612435655248, -7.730328572437724866, 21.50000000000000000 ) ) ;
#25922 = CARTESIAN_POINT ( 'NONE',  ( -28.34828976096172681, 29.18752572968383419, 1.500000000000000000 ) ) ;
#25923 = LINE ( 'NONE', #26071, #26823 ) ;
#25924 = ORIENTED_EDGE ( 'NONE', *, *, #7106, .F. ) ;
#25925 = CARTESIAN_POINT ( 'NONE',  ( -24.03057240117690441, -26.57182937991348481, -1.500000000000001332 ) ) ;
#25926 = CARTESIAN_POINT ( 'NONE',  ( 0.000000000000000000, 1.699320956058915452E-16, -1.500000000000001776 ) ) ;
#25927 = DIRECTION ( 'NONE',  ( -8.673617379884027583E-16, 1.000000000000000000, 0.000000000000000000 ) ) ;
#25928 = ORIENTED_EDGE ( 'NONE', *, *, #29644, .T. ) ;
#25929 = CARTESIAN_POINT ( 'NONE',  ( -1.000000000000008438, 13.00000000000001421, 24.50000000000000000 ) ) ;
#25930 = CARTESIAN_POINT ( 'NONE',  ( -17.64660589602035046, -9.450098986197517092, 19.79423548914561692 ) ) ;
#25931 = CARTESIAN_POINT ( 'NONE',  ( -33.03678701508917470, 25.60268426854908697, -16.50000000000000000 ) ) ;
#25932 = EDGE_CURVE ( 'NONE', #30628, #165, #6292, .T. ) ;
#25933 = CARTESIAN_POINT ( 'NONE',  ( 22.58267429318970443, -26.57182937991349903, -1.500000000000001332 ) ) ;
#25934 = ORIENTED_EDGE ( 'NONE', *, *, #27142, .F. ) ;
#25935 = DIRECTION ( 'NONE',  ( -1.000000000000000000, 0.000000000000000000, 0.000000000000000000 ) ) ;
#25936 = LINE ( 'NONE', #28290, #19618 ) ;
#25937 = EDGE_CURVE ( 'NONE', #23361, #5698, #20544, .T. ) ;
#25938 = CARTESIAN_POINT ( 'NONE',  ( 10.78888246121507599, -35.91932794629070003, 37.50000000001028866 ) ) ;
#25939 = ADVANCED_FACE ( 'NONE', ( #8858 ), #20689, .F. ) ;
#25940 = LINE ( 'NONE', #14074, #17066 ) ;
#25941 = ORIENTED_EDGE ( 'NONE', *, *, #8874, .F. ) ;
#25942 = AXIS2_PLACEMENT_3D ( 'NONE', #27817, #15790, #3793 ) ;
#25943 = B_SPLINE_CURVE_WITH_KNOTS ( 'NONE', 3,
 ( #21307, #15876, #27892, #11649 ),
 .UNSPECIFIED., .F., .F.,
 ( 4, 4 ),
 ( 0.000000000000000000, 0.005028157979644255586 ),
 .UNSPECIFIED. ) ;
#25944 = AXIS2_PLACEMENT_3D ( 'NONE', #9166, #19140, #1843 ) ;
#25945 = CARTESIAN_POINT ( 'NONE',  ( -13.54809176561740358, 10.35918576918405343, 7.652108011868851811 ) ) ;
#25946 = DIRECTION ( 'NONE',  ( 0.000000000000000000, 0.000000000000000000, 1.000000000000000000 ) ) ;
#25947 = CYLINDRICAL_SURFACE ( 'NONE', #6960, 9.482273699623480212 ) ;
#25948 = VERTEX_POINT ( 'NONE', #13693 ) ;
#25949 = EDGE_CURVE ( 'NONE', #19691, #1661, #594, .T. ) ;
#25950 = ORIENTED_EDGE ( 'NONE', *, *, #6576, .F. ) ;
#25951 = DIRECTION ( 'NONE',  ( 0.000000000000000000, 0.000000000000000000, 1.000000000000000000 ) ) ;
#25952 = EDGE_CURVE ( 'NONE', #3349, #27621, #20849, .T. ) ;
#25953 = VERTEX_POINT ( 'NONE', #9155 ) ;
#25954 = CARTESIAN_POINT ( 'NONE',  ( 0.2355109517537158914, -20.01673911375432269, 20.34789198813115263 ) ) ;
#25955 = EDGE_CURVE ( 'NONE', #28009, #15594, #3083, .T. ) ;
#25956 = CARTESIAN_POINT ( 'NONE',  ( -9.650234827617415689, -17.53789701089549879, 6.782048567692550378 ) ) ;
#25957 = LINE ( 'NONE', #28143, #28299 ) ;
#25958 = ADVANCED_FACE ( 'NONE', ( #23632 ), #9302, .F. ) ;
#25959 = CARTESIAN_POINT ( 'NONE',  ( 1.219801289189190729, -17.01504883035040905, 20.25542030744407640 ) ) ;
#25960 = ORIENTED_EDGE ( 'NONE', *, *, #1395, .T. ) ;
#25961 = DIRECTION ( 'NONE',  ( 0.000000000000000000, 1.000000000000000000, 0.000000000000000000 ) ) ;
#25962 = ADVANCED_FACE ( 'NONE', ( #26139 ), #28496, .T. ) ;
#25963 = CARTESIAN_POINT ( 'NONE',  ( -70.00000000000000000, -50.00000000000000000, 12.49999999999999112 ) ) ;
#25964 = CARTESIAN_POINT ( 'NONE',  ( 1.367923798957378034, -19.95316478012377104, 19.48477075383299351 ) ) ;
#25965 = CARTESIAN_POINT ( 'NONE',  ( 23.17581250239727808, -34.50630206824671831, -1.499999999999999778 ) ) ;
#25966 = ORIENTED_EDGE ( 'NONE', *, *, #10765, .F. ) ;
#25967 = VECTOR ( 'NONE', #29677, 1000.000000000000000 ) ;
#25968 = CARTESIAN_POINT ( 'NONE',  ( 29.15452456067750475, -29.11038375076027762, -6.500000000000000000 ) ) ;
#25969 = CARTESIAN_POINT ( 'NONE',  ( -13.37849590498012553, 10.56201291617987792, 20.34789198813115263 ) ) ;
#25970 = CARTESIAN_POINT ( 'NONE',  ( -8.757878075398936701, -7.394122547431892123, 1.500000000000000000 ) ) ;
#25971 = CARTESIAN_POINT ( 'NONE',  ( 3.094187858400090363, 16.79444423853913904, 19.08844262864049668 ) ) ;
#25972 = DIRECTION ( 'NONE',  ( -0.000000000000000000, -0.000000000000000000, 1.000000000000000000 ) ) ;
#25973 = PLANE ( 'NONE',  #21860 ) ;
#25974 = CARTESIAN_POINT ( 'NONE',  ( 32.60608336680204644, -8.625548295239457985, 37.02973996997542372 ) ) ;
#25975 = EDGE_LOOP ( 'NONE', ( #21202, #28249 ) ) ;
#25976 = ORIENTED_EDGE ( 'NONE', *, *, #22911, .F. ) ;
#25977 = CARTESIAN_POINT ( 'NONE',  ( 37.49999999999997158, 1.387778780781445676E-14, 37.50000000000000000 ) ) ;
#25978 = CARTESIAN_POINT ( 'NONE',  ( -10.64374042650306862, 42.96126232887723972, -19.50000000000000355 ) ) ;
#25979 = EDGE_CURVE ( 'NONE', #3526, #16618, #2276, .T. ) ;
#25980 = DIRECTION ( 'NONE',  ( 0.5406408174555976665, -0.8412535328311810945, 0.000000000000000000 ) ) ;
#25981 = EDGE_CURVE ( 'NONE', #7027, #29776, #252, .T. ) ;
#25983 = CARTESIAN_POINT ( 'NONE',  ( 11.93908819109399921, -16.04550321516295242, 19.21940439362674979 ) ) ;
#25982 = AXIS2_PLACEMENT_3D ( 'NONE', #25858, #23354, #23496 ) ;
#25984 = ORIENTED_EDGE ( 'NONE', *, *, #6675, .F. ) ;
#25985 = DIRECTION ( 'NONE',  ( 0.000000000000000000, 0.000000000000000000, 1.000000000000000000 ) ) ;
#25986 = CARTESIAN_POINT ( 'NONE',  ( 15.81223571690235019, -6.365019318618784006, 20.34789198813115263 ) ) ;
#25987 = EDGE_CURVE ( 'NONE', #4497, #7702, #4585, .T. ) ;
#25988 = CARTESIAN_POINT ( 'NONE',  ( 4.373786442354537840, 16.46525014965066092, 7.595116371587256054 ) ) ;
#25989 = ORIENTED_EDGE ( 'NONE', *, *, #10545, .F. ) ;
#25990 = CARTESIAN_POINT ( 'NONE',  ( 6.225165711324287088, 19.02535939286849498, 19.66989035740801839 ) ) ;
#25991 = EDGE_CURVE ( 'NONE', #28059, #30853, #7126, .T. ) ;
#25992 = CARTESIAN_POINT ( 'NONE',  ( 14.46722394715956561, 13.83532015011945937, 7.441806358946449151 ) ) ;
#25993 = AXIS2_PLACEMENT_3D ( 'NONE', #11505, #7589, #14126 ) ;
#25994 = DIRECTION ( 'NONE',  ( 0.000000000000000000, 0.000000000000000000, -1.000000000000000000 ) ) ;
#25995 = CARTESIAN_POINT ( 'NONE',  ( -27.00603848422143471, 26.04669493682374437, 37.49999999997637445 ) ) ;
#25996 = ORIENTED_EDGE ( 'NONE', *, *, #7480, .T. ) ;
#25997 = FACE_OUTER_BOUND ( 'NONE', #27961, .T. ) ;
#25998 = EDGE_CURVE ( 'NONE', #1974, #4023, #8079, .T. ) ;
#25999 = CARTESIAN_POINT ( 'NONE',  ( 32.28307784207223108, 8.475829241206289666, 37.38016955275583086 ) ) ;
#26000 = DIRECTION ( 'NONE',  ( -0.000000000000000000, -0.000000000000000000, 1.000000000000000000 ) ) ;
#26001 = ORIENTED_EDGE ( 'NONE', *, *, #22555, .T. ) ;
#26002 = CARTESIAN_POINT ( 'NONE',  ( -15.49606647121365910, -7.052879176030718789, 7.272049892295485485 ) ) ;
#26003 = CARTESIAN_POINT ( 'NONE',  ( 16.85582347140584858, 2.398957759809809076, 18.72771030977187579 ) ) ;
#26004 = CARTESIAN_POINT ( 'NONE',  ( 27.03074382657074182, -6.449748410230990991, 42.96778633356034049 ) ) ;
#26005 = AXIS2_PLACEMENT_3D ( 'NONE', #7206, #5754, #14538 ) ;
#26006 = CARTESIAN_POINT ( 'NONE',  ( 23.17549888352340659, -36.17843697208695630, -16.49999999999999645 ) ) ;
#26007 = CARTESIAN_POINT ( 'NONE',  ( -0.5107318660475965721, -20.01137538934480986, 7.176035686813569292 ) ) ;
#26008 = CARTESIAN_POINT ( 'NONE',  ( 25.18466322232234234, -6.657711795334220639, 48.95036236631847260 ) ) ;
#26009 = DIRECTION ( 'NONE',  ( -1.000000000000000000, 0.000000000000000000, -0.000000000000000000 ) ) ;
#26010 = FACE_OUTER_BOUND ( 'NONE', #21247, .T. ) ;
#26011 = DIRECTION ( 'NONE',  ( -0.000000000000000000, -0.000000000000000000, 1.000000000000000000 ) ) ;
#26012 = ORIENTED_EDGE ( 'NONE', *, *, #17781, .T. ) ;
#26013 = EDGE_CURVE ( 'NONE', #19602, #10953, #30450, .T. ) ;
#26014 = EDGE_CURVE ( 'NONE', #16473, #27870, #8592, .T. ) ;
#26015 = CARTESIAN_POINT ( 'NONE',  ( -6.507434545313858898, 15.78991698230835361, 6.783738457429056012 ) ) ;
#26016 = CARTESIAN_POINT ( 'NONE',  ( 0.000000000000000000, 0.000000000000000000, 21.50000000000000000 ) ) ;
#26017 = EDGE_LOOP ( 'NONE', ( #1295, #9648 ) ) ;
#26018 = ORIENTED_EDGE ( 'NONE', *, *, #9763, .T. ) ;
#26019 = CARTESIAN_POINT ( 'NONE',  ( -47.36551906495753883, 69.82702131092923992, 59.27138182264830135 ) ) ;
#26020 = VERTEX_POINT ( 'NONE', #2598 ) ;
#26021 = CYLINDRICAL_SURFACE ( 'NONE', #16669, 11.46182693247429718 ) ;
#26022 = VERTEX_POINT ( 'NONE', #26460 ) ;
#26023 = AXIS2_PLACEMENT_3D ( 'NONE', #30043, #8684, #16609 ) ;
#26024 = FACE_OUTER_BOUND ( 'NONE', #2293, .T. ) ;
#26025 = CARTESIAN_POINT ( 'NONE',  ( 19.59127448685153894, 4.109591991357616436, 18.92976555901915603 ) ) ;
#26026 = CARTESIAN_POINT ( 'NONE',  ( -25.53015708495999903, 6.470147010658195974, 48.66282223834838305 ) ) ;
#26027 = VERTEX_POINT ( 'NONE', #21136 ) ;
#26028 = DIRECTION ( 'NONE',  ( 1.000000000000000000, 0.000000000000000000, 0.000000000000000000 ) ) ;
#26029 = ORIENTED_EDGE ( 'NONE', *, *, #3160, .F. ) ;
#26030 = B_SPLINE_CURVE_WITH_KNOTS ( 'NONE', 3,
 ( #2837, #11901, #176, #19058 ),
 .UNSPECIFIED., .F., .F.,
 ( 4, 4 ),
 ( 0.000000000000000000, 0.005028157979644231300 ),
 .UNSPECIFIED. ) ;
#26031 = ORIENTED_EDGE ( 'NONE', *, *, #10695, .T. ) ;
#26032 = CARTESIAN_POINT ( 'NONE',  ( -42.49999999999998579, -50.00000000000000000, 12.49999999999999112 ) ) ;
#26033 = CARTESIAN_POINT ( 'NONE',  ( -8.860628911697515875, 8.184276679720483116, 1.500000000000000000 ) ) ;
#26034 = CARTESIAN_POINT ( 'NONE',  ( 1.068432182113367990, -19.98925970413798936, 7.366751648393900176 ) ) ;
#26035 = CARTESIAN_POINT ( 'NONE',  ( -6.397449029611151694, -41.94755430240511629, 28.88750951715501714 ) ) ;
#26036 = VECTOR ( 'NONE', #14788, 1000.000000000000000 ) ;
#26037 = CARTESIAN_POINT ( 'NONE',  ( 20.47140768548292655, -27.01178922547192585, -16.50001200000000168 ) ) ;
#26038 = CARTESIAN_POINT ( 'NONE',  ( -43.34097750826428097, 11.89502811014148342, 1.500000000000000444 ) ) ;
#26039 = VERTEX_POINT ( 'NONE', #24106 ) ;
#26040 = DIRECTION ( 'NONE',  ( 0.000000000000000000, -1.132880637372608986E-16, 1.000000000000000000 ) ) ;
#26041 = LINE ( 'NONE', #16217, #15238 ) ;
#26042 = CARTESIAN_POINT ( 'NONE',  ( -13.59008529392184883, 10.30512752726515124, 7.603368798681074736 ) ) ;
#26043 = CARTESIAN_POINT ( 'NONE',  ( -26.83043119477639493, -8.695877139419037505, 1.500000000000000000 ) ) ;
#26044 = VERTEX_POINT ( 'NONE', #16638 ) ;
#26045 = ORIENTED_EDGE ( 'NONE', *, *, #9196, .T. ) ;
#26046 = EDGE_CURVE ( 'NONE', #30031, #21650, #2447, .T. ) ;
#26047 = CARTESIAN_POINT ( 'NONE',  ( 0.000000000000000000, 0.000000000000000000, -87.50000000000000000 ) ) ;
#26048 = CARTESIAN_POINT ( 'NONE',  ( 21.22112865003566640, -24.30434497425369855, -16.50001199999999812 ) ) ;
#26049 = CARTESIAN_POINT ( 'NONE',  ( -40.05104235265675783, 2.353288714454549790, -11.49999999999999645 ) ) ;
#26050 = PLANE ( 'NONE',  #3387 ) ;
#26051 = CARTESIAN_POINT ( 'NONE',  ( -28.34828976096172681, -29.18752572968383419, 1.500000000000000000 ) ) ;
#26052 = DIRECTION ( 'NONE',  ( 1.000000000000000000, 0.000000000000000000, -0.000000000000000000 ) ) ;
#26053 = CARTESIAN_POINT ( 'NONE',  ( -5.485816626893764258, 19.23332246807784784, 7.526993102356320797 ) ) ;
#26054 = VERTEX_POINT ( 'NONE', #9764 ) ;
#26055 = CARTESIAN_POINT ( 'NONE',  ( -19.93127403599639891, 1.860458748833899278, 5.872146474157316831 ) ) ;
#26056 = CARTESIAN_POINT ( 'NONE',  ( -0.4564504349075017564, 9.471281197126600659, 1.500000000000001332 ) ) ;
#26057 = DIRECTION ( 'NONE',  ( 0.000000000000000000, 0.000000000000000000, 1.000000000000000000 ) ) ;
#26058 = ORIENTED_EDGE ( 'NONE', *, *, #12406, .F. ) ;
#26059 = DIRECTION ( 'NONE',  ( 0.000000000000000000, 0.000000000000000000, -1.000000000000000000 ) ) ;
#26060 = AXIS2_PLACEMENT_3D ( 'NONE', #2721, #30220, #8865 ) ;
#26061 = EDGE_LOOP ( 'NONE', ( #13263, #5648, #6093, #5151 ) ) ;
#26062 = CARTESIAN_POINT ( 'NONE',  ( -5.687793815610304726, 6.974883619896852238, 21.50000000000000000 ) ) ;
#26063 = AXIS2_PLACEMENT_3D ( 'NONE', #8924, #9517, #11866 ) ;
#26064 = CARTESIAN_POINT ( 'NONE',  ( -19.96030473831224583, 38.37413104131353947, -16.50000000000000000 ) ) ;
#26065 = VERTEX_POINT ( 'NONE', #19277 ) ;
#26066 = CARTESIAN_POINT ( 'NONE',  ( 29.09438610025163641, 23.39414391798310078, 27.50000000000000355 ) ) ;
#26067 = CARTESIAN_POINT ( 'NONE',  ( 6.674134664086328605, 49.56092362459834533, -41.53091777090556747 ) ) ;
#26068 = CYLINDRICAL_SURFACE ( 'NONE', #13515, 0.7500000000000006661 ) ;
#26069 = CARTESIAN_POINT ( 'NONE',  ( -18.30192086700450815, -8.065271870204650639, 7.454139397117723220 ) ) ;
#26070 = CARTESIAN_POINT ( 'NONE',  ( -6.482337650448453559, -6.364020599487773211, -1.500000000000002442 ) ) ;
#26071 = CARTESIAN_POINT ( 'NONE',  ( -3.668292057955944596, 8.743977807160110416, 13.00000000000000178 ) ) ;
#26072 = ORIENTED_EDGE ( 'NONE', *, *, #14549, .F. ) ;
#26073 = CARTESIAN_POINT ( 'NONE',  ( 15.55638214364780758, -6.928938690364088160, 7.453286057244487672 ) ) ;
#26074 = AXIS2_PLACEMENT_3D ( 'NONE', #19097, #2723, #12231 ) ;
#26075 = CARTESIAN_POINT ( 'NONE',  ( -32.74775157610760346, -27.21557300919352329, -19.50000000000000355 ) ) ;
#26076 = CYLINDRICAL_SURFACE ( 'NONE', #17803, 9.000000000000000000 ) ;
#26077 = ORIENTED_EDGE ( 'NONE', *, *, #22939, .F. ) ;
#26078 = CARTESIAN_POINT ( 'NONE',  ( 8.840471615930072247, -1.687027447297460236, 1.500000000000001332 ) ) ;
#26079 = AXIS2_PLACEMENT_3D ( 'NONE', #11061, #9032, #25558 ) ;
#26080 = CARTESIAN_POINT ( 'NONE',  ( -14.81015662609899408, -8.488192507792284403, 19.97651184436794125 ) ) ;
#26081 = DIRECTION ( 'NONE',  ( 1.000000000000000000, 0.000000000000000000, 0.000000000000000000 ) ) ;
#26082 = AXIS2_PLACEMENT_3D ( 'NONE', #30162, #6466, #29704 ) ;
#26083 = CARTESIAN_POINT ( 'NONE',  ( -50.00000000000000000, 70.00000000000000000, 22.49999999999999289 ) ) ;
#26084 = DIRECTION ( 'NONE',  ( -0.000000000000000000, -0.000000000000000000, 1.000000000000000000 ) ) ;
#26085 = ORIENTED_EDGE ( 'NONE', *, *, #6552, .T. ) ;
#26086 = CARTESIAN_POINT ( 'NONE',  ( -0.6299556268942225756, -19.99014111075368305, 19.08232364404839743 ) ) ;
#26087 = CARTESIAN_POINT ( 'NONE',  ( -46.99999999999955236, -4.867219302015485475E-13, 82.49999999999998579 ) ) ;
#26088 = CARTESIAN_POINT ( 'NONE',  ( 29.37505062631091945, 27.96840008810541178, 34.56100623550605633 ) ) ;
#26089 = CARTESIAN_POINT ( 'NONE',  ( -6.813581335325352484, 18.80366338534912529, 6.149077423860700442 ) ) ;
#26090 = ORIENTED_EDGE ( 'NONE', *, *, #13014, .F. ) ;
#26091 = LINE ( 'NONE', #4122, #14608 ) ;
#26092 = ORIENTED_EDGE ( 'NONE', *, *, #15271, .F. ) ;
#26093 = CARTESIAN_POINT ( 'NONE',  ( 5.687793815610356241, -6.974883619896809606, 1.500000000000001332 ) ) ;
#26094 = CARTESIAN_POINT ( 'NONE',  ( -28.34828976096172681, -29.18752572968383063, -1.500000000000000000 ) ) ;
#26095 = ORIENTED_EDGE ( 'NONE', *, *, #7568, .F. ) ;
#26096 = ORIENTED_EDGE ( 'NONE', *, *, #12893, .F. ) ;
#26097 = CARTESIAN_POINT ( 'NONE',  ( -6.062559277181930106, 5.881244434206302607, -3.621320343559650379 ) ) ;
#26098 = PRODUCT_DEFINITION_SHAPE ( 'NONE', 'NONE',  #21923 ) ;
#26099 = ORIENTED_EDGE ( 'NONE', *, *, #13806, .F. ) ;
#26100 = EDGE_LOOP ( 'NONE', ( #17359, #1696, #29825, #20189 ) ) ;
#26101 = CARTESIAN_POINT ( 'NONE',  ( 6.187077094091595342, 11.47693674426096599, 24.50000000000000000 ) ) ;
#26102 = AXIS2_PLACEMENT_3D ( 'NONE', #20935, #2069, #16124 ) ;
#26103 = CARTESIAN_POINT ( 'NONE',  ( -5.687793815610304726, 6.974883619896852238, 21.50000000000000000 ) ) ;
#26104 = CARTESIAN_POINT ( 'NONE',  ( 4.823417667949169818, 16.32807078418213464, 19.96344307082652492 ) ) ;
#26105 = CARTESIAN_POINT ( 'NONE',  ( 1.365674945463512646, -19.97097327164668812, 19.36813350477385143 ) ) ;
#26106 = ORIENTED_EDGE ( 'NONE', *, *, #2534, .T. ) ;
#26107 = CARTESIAN_POINT ( 'NONE',  ( 18.64567588040446111, -7.235161915364464846, 6.037995405461180631 ) ) ;
#26108 = CARTESIAN_POINT ( 'NONE',  ( 23.00100564343818021, 35.20929534198214128, -8.166629675737638649 ) ) ;
#26109 = CARTESIAN_POINT ( 'NONE',  ( 1.159631224985661513, -19.96657546246603943, 19.96797677718664232 ) ) ;
#26110 = CARTESIAN_POINT ( 'NONE',  ( 7.500000000000000000, 5.196152422706634688, -9.000000000000001776 ) ) ;
#26111 = VERTEX_POINT ( 'NONE', #21458 ) ;
#26112 = PRODUCT_RELATED_PRODUCT_CATEGORY ( 'part', '', ( #7963 ) ) ;
#26113 = FACE_OUTER_BOUND ( 'NONE', #29675, .T. ) ;
#26114 = CARTESIAN_POINT ( 'NONE',  ( -17.73231296732452478, -9.288543855440103414, 5.951255046771932733 ) ) ;
#26115 = CARTESIAN_POINT ( 'NONE',  ( -37.99999999999999289, 209.2686044187655909, -75.50000000000000000 ) ) ;
#26116 = CARTESIAN_POINT ( 'NONE',  ( 24.03057240117691862, 26.57182937991349903, -6.500000000000000888 ) ) ;
#26117 = EDGE_CURVE ( 'NONE', #6039, #30777, #2755, .T. ) ;
#26118 = CARTESIAN_POINT ( 'NONE',  ( 6.601643239663004076E-16, 42.50000000000000000, 28.83974596215562514 ) ) ;
#26119 = LINE ( 'NONE', #23934, #12588 ) ;
#26120 = EDGE_LOOP ( 'NONE', ( #20881, #3886, #809, #9029 ) ) ;
#26121 = EDGE_LOOP ( 'NONE', ( #6350, #24938, #21450, #25543 ) ) ;
#26122 = CARTESIAN_POINT ( 'NONE',  ( -12.50000000000000000, 0.000000000000000000, -52.50000000000000000 ) ) ;
#26123 = CARTESIAN_POINT ( 'NONE',  ( -39.00000000000000000, 5.563236990218665134, -1.500000000000000000 ) ) ;
#26124 = CARTESIAN_POINT ( 'NONE',  ( -13.37849590052435289, 10.56201291103764106, 7.652108011868850035 ) ) ;
#26125 = DIRECTION ( 'NONE',  ( 0.000000000000000000, 0.000000000000000000, -1.000000000000000000 ) ) ;
#26126 = ORIENTED_EDGE ( 'NONE', *, *, #25981, .T. ) ;
#26127 = CARTESIAN_POINT ( 'NONE',  ( 18.12620810650619418, -8.494884113463653463, 20.19668224736330941 ) ) ;
#26128 = EDGE_CURVE ( 'NONE', #29372, #20109, #407, .T. ) ;
#26129 = CARTESIAN_POINT ( 'NONE',  ( 5.008980049945720658, 16.26773947435521706, 6.530762810602277924 ) ) ;
#26130 = B_SPLINE_CURVE_WITH_KNOTS ( 'NONE', 3,
 ( #24880, #20348, #8659, #3518, #10841, #3665, #8350, #15817, #10527, #5691, #25336, #13179, #8798, #15187, #22520, #6152 ),
 .UNSPECIFIED., .F., .F.,
 ( 4, 2, 2, 2, 2, 2, 2, 4 ),
 ( 0.4999999999999997780, 0.6249999999999996669, 0.6874999999999995559, 0.7187499999999995559, 0.7499999999999996669, 0.8124999999999996669, 0.8749999999999997780, 1.000000000000000000 ),
 .UNSPECIFIED. ) ;
#26131 = EDGE_CURVE ( 'NONE', #30824, #16597, #26496, .T. ) ;
#26132 = ORIENTED_EDGE ( 'NONE', *, *, #2137, .T. ) ;
#26133 = CARTESIAN_POINT ( 'NONE',  ( 6.270562923531076471, 19.01045013183040311, 19.45164628100866722 ) ) ;
#26134 = DIRECTION ( 'NONE',  ( 0.000000000000000000, -0.000000000000000000, 1.000000000000000000 ) ) ;
#26135 = LINE ( 'NONE', #1979, #26288 ) ;
#26136 = CARTESIAN_POINT ( 'NONE',  ( -27.78122617307444031, 29.83607645924699270, 30.06620328777349016 ) ) ;
#26137 = ORIENTED_EDGE ( 'NONE', *, *, #2926, .T. ) ;
#26138 = CARTESIAN_POINT ( 'NONE',  ( 23.21352257770656635, -10.78826658734920052, -16.55003854064094426 ) ) ;
#26139 = FACE_OUTER_BOUND ( 'NONE', #19752, .T. ) ;
#26140 = CARTESIAN_POINT ( 'NONE',  ( -8.413215745754975217, 3.196529495465474380, 1.500000000000001332 ) ) ;
#26141 = ORIENTED_EDGE ( 'NONE', *, *, #1983, .F. ) ;
#26142 = CARTESIAN_POINT ( 'NONE',  ( -6.962021646281573162, -6.437683520590147701, 13.00000000000000178 ) ) ;
#26143 = VECTOR ( 'NONE', #12254, 1000.000000000000000 ) ;
#26144 = FACE_OUTER_BOUND ( 'NONE', #20730, .T. ) ;
#26145 = EDGE_CURVE ( 'NONE', #5487, #13230, #29717, .T. ) ;
#26146 = DIRECTION ( 'NONE',  ( -0.000000000000000000, -0.000000000000000000, -1.000000000000000000 ) ) ;
#26147 = EDGE_CURVE ( 'NONE', #10252, #9325, #29984, .T. ) ;
#26148 = LINE ( 'NONE', #26625, #4811 ) ;
#26149 = EDGE_CURVE ( 'NONE', #26677, #15822, #1185, .T. ) ;
#26150 =( REPRESENTATION_RELATIONSHIP ('NONE','NONE', #19885, #7129 ) REPRESENTATION_RELATIONSHIP_WITH_TRANSFORMATION ( #8190 )SHAPE_REPRESENTATION_RELATIONSHIP( ) );
#26151 = ADVANCED_FACE ( 'NONE', ( #7904 ), #19906, .F. ) ;
#26152 = CYLINDRICAL_SURFACE ( 'NONE', #25227, 1.999999999999998224 ) ;
#26153 = DIRECTION ( 'NONE',  ( 0.000000000000000000, 0.000000000000000000, -1.000000000000000000 ) ) ;
#26154 = CARTESIAN_POINT ( 'NONE',  ( 33.64310889498737822, -21.53861670882606916, 18.00000000000000000 ) ) ;
#26155 = DIRECTION ( 'NONE',  ( 0.000000000000000000, 0.000000000000000000, -1.000000000000000000 ) ) ;
#26156 = ORIENTED_EDGE ( 'NONE', *, *, #6915, .F. ) ;
#26157 = ADVANCED_FACE ( 'NONE', ( #27392 ), #26774, .F. ) ;
#26158 = CARTESIAN_POINT ( 'NONE',  ( 10.61155637842188959, -13.37681800088531503, 19.79423548914561692 ) ) ;
#26159 = LINE ( 'NONE', #9482, #27529 ) ;
#26160 = VERTEX_POINT ( 'NONE', #12428 ) ;
#26161 = VERTEX_POINT ( 'NONE', #14909 ) ;
#26162 = EDGE_CURVE ( 'NONE', #15912, #12022, #29494, .T. ) ;
#26163 = CARTESIAN_POINT ( 'NONE',  ( -15.51115086193518700, 12.62612245312785753, 7.626218077512942450 ) ) ;
#26164 = EDGE_CURVE ( 'NONE', #863, #25840, #29569, .T. ) ;
#26165 = CARTESIAN_POINT ( 'NONE',  ( 37.99999999999999289, 70.00000000000000000, -75.50000000000001421 ) ) ;
#26166 = ORIENTED_EDGE ( 'NONE', *, *, #3877, .F. ) ;
#26167 = CARTESIAN_POINT ( 'NONE',  ( 12.65169814564036521, 11.40562544919841237, 20.25336174263950184 ) ) ;
#26168 = VECTOR ( 'NONE', #15781, 1000.000000000000000 ) ;
#26169 = DIRECTION ( 'NONE',  ( 0.000000000000000000, 0.000000000000000000, 1.000000000000000000 ) ) ;
#26170 = EDGE_LOOP ( 'NONE', ( #25750, #29635, #25464, #18562, #5055, #9635, #4298 ) ) ;
#26171 = LINE ( 'NONE', #26642, #15264 ) ;
#26172 = CARTESIAN_POINT ( 'NONE',  ( 16.73033351903584176, 3.274018421667484802, 18.34838970509067479 ) ) ;
#26173 = DIRECTION ( 'NONE',  ( 0.000000000000000000, 0.000000000000000000, 1.000000000000000000 ) ) ;
#26174 = ORIENTED_EDGE ( 'NONE', *, *, #25998, .F. ) ;
#26175 = CARTESIAN_POINT ( 'NONE',  ( 0.000000000000000000, 0.000000000000000000, 1.500000000000000000 ) ) ;
#26176 = ORIENTED_EDGE ( 'NONE', *, *, #22337, .T. ) ;
#26177 = EDGE_CURVE ( 'NONE', #28625, #12261, #13070, .T. ) ;
#26178 = VECTOR ( 'NONE', #11128, 1000.000000000000000 ) ;
#26179 = ORIENTED_EDGE ( 'NONE', *, *, #24067, .F. ) ;
#26180 = ADVANCED_FACE ( 'NONE', ( #8200 ), #27224, .F. ) ;
#26181 = EDGE_CURVE ( 'NONE', #26711, #10771, #3104, .T. ) ;
#26182 = LINE ( 'NONE', #4201, #20076 ) ;
#26183 = CARTESIAN_POINT ( 'NONE',  ( 24.03057240117691862, -26.57182937991349903, -1.500000000000000000 ) ) ;
#26184 = CARTESIAN_POINT ( 'NONE',  ( 1.771654956907825262, -16.98531529776322913, 6.892848776733236704 ) ) ;
#26185 = CIRCLE ( 'NONE', #4767, 9.084132297865673777 ) ;
#26186 = CARTESIAN_POINT ( 'NONE',  ( -15.16307827826492449, -7.786259562520723598, 18.34798005863078885 ) ) ;
#26187 = CARTESIAN_POINT ( 'NONE',  ( 1.788804076106752072, -16.98411955790561123, 19.21769074125273136 ) ) ;
#26188 = CARTESIAN_POINT ( 'NONE',  ( 19.77852387640474419, 3.085824932809439591, 18.35377592296120497 ) ) ;
#26189 = ORIENTED_EDGE ( 'NONE', *, *, #16466, .F. ) ;
#26190 = CARTESIAN_POINT ( 'NONE',  ( -16.83148396119934276, 2.548526378087590416, 18.90679857307105749 ) ) ;
#26191 = DIRECTION ( 'NONE',  ( 0.000000000000000000, 1.000000000000000000, 0.000000000000000000 ) ) ;
#26192 = DIRECTION ( 'NONE',  ( 1.000000000000000000, 0.000000000000000000, -0.000000000000000000 ) ) ;
#26193 = EDGE_LOOP ( 'NONE', ( #11423, #25984, #2216, #29971 ) ) ;
#26194 = EDGE_LOOP ( 'NONE', ( #29705, #8013, #27267, #3437 ) ) ;
#26195 = DIRECTION ( 'NONE',  ( -0.8412535328311804284, 0.5406408174555987767, 0.000000000000000000 ) ) ;
#26196 = CARTESIAN_POINT ( 'NONE',  ( 22.68724997019158707, -23.22071843469717933, -16.50001200000000523 ) ) ;
#26197 = B_SPLINE_CURVE_WITH_KNOTS ( 'NONE', 3,
 ( #16465, #7251, #25830, #16764, #16159, #1814, #11335, #11488, #18655, #28160, #16314, #23469, #12411, #22214, #5229, #12563 ),
 .UNSPECIFIED., .F., .F.,
 ( 4, 2, 2, 2, 2, 2, 2, 4 ),
 ( 0.5000000000000000000, 0.6249999999999995559, 0.6874999999999997780, 0.7187500000000000000, 0.7500000000000002220, 0.8125000000000001110, 0.8750000000000000000, 1.000000000000000000 ),
 .UNSPECIFIED. ) ;
#26198 = DIRECTION ( 'NONE',  ( 0.3598999890241665334, -0.9329908884337535513, 0.000000000000000000 ) ) ;
#26199 = CARTESIAN_POINT ( 'NONE',  ( -5.941992259041529501, 19.11559255287554393, 18.34777357837151968 ) ) ;
#26200 = CARTESIAN_POINT ( 'NONE',  ( -0.9621688436940063482, -9.033033306777452864, -1.500000000000002887 ) ) ;
#26201 = CIRCLE ( 'NONE', #16249, 32.50000000000000000 ) ;
#26202 = CARTESIAN_POINT ( 'NONE',  ( -18.68130254075365215, -33.76891359627503419, 27.50000000000000711 ) ) ;
#26203 = CARTESIAN_POINT ( 'NONE',  ( -5.125804696664927995, 19.33206434738279356, 6.144783687052520094 ) ) ;
#26204 = EDGE_LOOP ( 'NONE', ( #14593, #6689, #55, #22490 ) ) ;
#26205 = CARTESIAN_POINT ( 'NONE',  ( -25.25456494851459865, -28.22455358388291202, 34.49999999999998579 ) ) ;
#26206 = DIRECTION ( 'NONE',  ( 0.000000000000000000, 0.000000000000000000, 1.000000000000000000 ) ) ;
#26207 = DIRECTION ( 'NONE',  ( 1.000000000000000000, 0.000000000000000000, 0.000000000000000000 ) ) ;
#26208 = ORIENTED_EDGE ( 'NONE', *, *, #16053, .T. ) ;
#26209 = CARTESIAN_POINT ( 'NONE',  ( 12.97958999564962568, 11.01328844340111068, 6.310736198168394928 ) ) ;
#26210 = EDGE_CURVE ( 'NONE', #27497, #23872, #27958, .T. ) ;
#26211 = CARTESIAN_POINT ( 'NONE',  ( 18.35115018089978633, -7.996680568998187688, 7.652108011868850035 ) ) ;
#26212 = ADVANCED_FACE ( 'NONE', ( #15670 ), #1945, .F. ) ;
#26213 = VECTOR ( 'NONE', #15473, 1000.000000000000000 ) ;
#26214 = FACE_OUTER_BOUND ( 'NONE', #15925, .T. ) ;
#26215 = ORIENTED_EDGE ( 'NONE', *, *, #4227, .T. ) ;
#26216 = CARTESIAN_POINT ( 'NONE',  ( 2.477745044295800891, 39.41216975536991640, 27.50000000000000000 ) ) ;
#26217 = CARTESIAN_POINT ( 'NONE',  ( 0.5595136366802240246, -4.349754824395735575, 9.000000000000001776 ) ) ;
#26218 = CARTESIAN_POINT ( 'NONE',  ( 10.52757208845869208, -13.43854510672091074, 18.73314399819311760 ) ) ;
#26219 = CARTESIAN_POINT ( 'NONE',  ( -24.03057240117691862, -26.57182937991349903, 1.500000000000000000 ) ) ;
#26220 = AXIS2_PLACEMENT_3D ( 'NONE', #10985, #18155, #20486 ) ;
#26221 = CIRCLE ( 'NONE', #16250, 0.7499999999999988898 ) ;
#26222 = CARTESIAN_POINT ( 'NONE',  ( -31.29501345865529061, -26.27841684422010360, -6.500000000000000888 ) ) ;
#26223 = CARTESIAN_POINT ( 'NONE',  ( 10.58781394000596343, -16.96782583993082838, 20.14992337338002670 ) ) ;
#26224 = ORIENTED_EDGE ( 'NONE', *, *, #13042, .F. ) ;
#26225 = DIRECTION ( 'NONE',  ( 0.000000000000000000, -0.000000000000000000, -1.000000000000000000 ) ) ;
#26226 = AXIS2_PLACEMENT_3D ( 'NONE', #11931, #17206, #7083 ) ;
#26227 = CARTESIAN_POINT ( 'NONE',  ( 12.56641067637329812, 40.32935944495179115, -1.500000000000000000 ) ) ;
#26228 = CYLINDRICAL_SURFACE ( 'NONE', #28256, 27.70876437800068359 ) ;
#26229 = VERTEX_POINT ( 'NONE', #1332 ) ;
#26230 = CARTESIAN_POINT ( 'NONE',  ( -19.84344116185556217, 2.497567387674351824, 20.34789198813115263 ) ) ;
#26231 = AXIS2_PLACEMENT_3D ( 'NONE', #23711, #21067, #25766 ) ;
#26232 = CARTESIAN_POINT ( 'NONE',  ( -17.73902742151047107, -9.275718677609281926, 20.06253562465620632 ) ) ;
#26233 = CARTESIAN_POINT ( 'NONE',  ( -32.24119420145671455, 26.76047160551536663, -16.50000600000000262 ) ) ;
#26234 = AXIS2_PLACEMENT_3D ( 'NONE', #6453, #23116, #173 ) ;
#26235 = DIRECTION ( 'NONE',  ( -0.000000000000000000, -0.000000000000000000, 1.000000000000000000 ) ) ;
#26236 = VECTOR ( 'NONE', #13601, 1000.000000000000000 ) ;
#26237 = PLANE ( 'NONE',  #16100 ) ;
#26238 = EDGE_LOOP ( 'NONE', ( #24894, #8087, #18201, #7619 ) ) ;
#26239 = CARTESIAN_POINT ( 'NONE',  ( 36.99855377474076334, 13.50962263858970225, 34.89305612718171545 ) ) ;
#26240 = PLANE ( 'NONE',  #10095 ) ;
#26241 = EDGE_LOOP ( 'NONE', ( #12451, #29418, #20496, #19520 ) ) ;
#26242 = PLANE ( 'NONE',  #17678 ) ;
#26243 = VERTEX_POINT ( 'NONE', #20806 ) ;
#26244 = CARTESIAN_POINT ( 'NONE',  ( 12.56641067637628240, -40.32935944494942504, -1.500000000000000000 ) ) ;
#26245 = CYLINDRICAL_SURFACE ( 'NONE', #19424, 9.482273699623480212 ) ;
#26246 = ORIENTED_EDGE ( 'NONE', *, *, #8648, .T. ) ;
#26247 = ORIENTED_EDGE ( 'NONE', *, *, #29230, .F. ) ;
#26248 = CARTESIAN_POINT ( 'NONE',  ( -0.6883321258581104329, 8.884323311075791096, -3.621320343559650379 ) ) ;
#26249 = ORIENTED_EDGE ( 'NONE', *, *, #23006, .F. ) ;
#26250 = AXIS2_PLACEMENT_3D ( 'NONE', #17590, #27423, #29448 ) ;
#26251 = VERTEX_POINT ( 'NONE', #11465 ) ;
#26252 = ORIENTED_EDGE ( 'NONE', *, *, #2378, .F. ) ;
#26253 = CARTESIAN_POINT ( 'NONE',  ( 0.2321890030833208829, -17.02978461145532307, 20.19668224736330941 ) ) ;
#26254 = CIRCLE ( 'NONE', #11807, 4.999999999999997335 ) ;
#26255 = CARTESIAN_POINT ( 'NONE',  ( 6.899999999999999467, -5.196152422706651564, 9.000000000000001776 ) ) ;
#26256 = VECTOR ( 'NONE', #6418, 1000.000000000000000 ) ;
#26257 = DIRECTION ( 'NONE',  ( 0.000000000000000000, 0.000000000000000000, 1.000000000000000000 ) ) ;
#26258 = CARTESIAN_POINT ( 'NONE',  ( -50.00000000000000000, 50.00000000000000000, 12.49999999999998401 ) ) ;
#26259 = ORIENTED_EDGE ( 'NONE', *, *, #1976, .T. ) ;
#26260 = CARTESIAN_POINT ( 'NONE',  ( 29.55332031600731213, 27.89853503085377895, -1.500000000000003997 ) ) ;
#26261 = CARTESIAN_POINT ( 'NONE',  ( 0.000000000000000000, 0.000000000000000000, -87.50000000000000000 ) ) ;
#26262 = CARTESIAN_POINT ( 'NONE',  ( 14.35775550668713585, 13.94852561378611711, 19.97651184436794125 ) ) ;
#26263 = DIRECTION ( 'NONE',  ( 0.000000000000000000, 1.000000000000000000, 0.000000000000000000 ) ) ;
#26264 = AXIS2_PLACEMENT_3D ( 'NONE', #25003, #24686, #996 ) ;
#26265 = EDGE_LOOP ( 'NONE', ( #8404, #20128, #7869, #29399 ) ) ;
#26266 = AXIS2_PLACEMENT_3D ( 'NONE', #17960, #8600, #20583 ) ;
#26267 = CIRCLE ( 'NONE', #12842, 0.7499999999999988898 ) ;
#26268 = LINE ( 'NONE', #17217, #6423 ) ;
#26269 = DIRECTION ( 'NONE',  ( -0.000000000000000000, 1.132880637372608986E-16, -1.000000000000000000 ) ) ;
#26270 = CARTESIAN_POINT ( 'NONE',  ( 3.221450758838616757, 1.621276839356792454, 1.500000000000000000 ) ) ;
#26271 = DIRECTION ( 'NONE',  ( 1.000000000000000000, 0.000000000000000000, 0.000000000000000000 ) ) ;
#26272 = AXIS2_PLACEMENT_3D ( 'NONE', #955, #10465, #19655 ) ;
#26273 = CARTESIAN_POINT ( 'NONE',  ( 0.8038475772933620922, 5.196152422706624030, 9.000000000000001776 ) ) ;
#26274 = CARTESIAN_POINT ( 'NONE',  ( 10.11202017158463917, -41.14070756921186955, -1.500000000000000000 ) ) ;
#26275 = VECTOR ( 'NONE', #945, 1000.000000000000000 ) ;
#26276 = VERTEX_POINT ( 'NONE', #27850 ) ;
#26277 = EDGE_LOOP ( 'NONE', ( #19941, #17195, #25756, #5458 ) ) ;
#26278 = AXIS2_PLACEMENT_3D ( 'NONE', #22180, #24516, #19073 ) ;
#26279 = AXIS2_PLACEMENT_3D ( 'NONE', #14127, #1677, #8859 ) ;
#26280 = CARTESIAN_POINT ( 'NONE',  ( -4.390207617113899730, 7.856594496258241023, 21.50000000000000000 ) ) ;
#26281 = CARTESIAN_POINT ( 'NONE',  ( -13.22505861668333083, 42.10773672057167261, -19.50000000000000355 ) ) ;
#26282 = FACE_OUTER_BOUND ( 'NONE', #30409, .T. ) ;
#26283 = DIRECTION ( 'NONE',  ( -0.000000000000000000, 1.132880637372608986E-16, -1.000000000000000000 ) ) ;
#26284 = ORIENTED_EDGE ( 'NONE', *, *, #15464, .F. ) ;
#26285 = VECTOR ( 'NONE', #17602, 1000.000000000000000 ) ;
#26286 = CARTESIAN_POINT ( 'NONE',  ( 17.92217092160593950, -8.916983838002000340, 19.33715507985239412 ) ) ;
#26287 = CARTESIAN_POINT ( 'NONE',  ( 4.917955972067796111, 16.29747060413738069, 6.211014596808754007 ) ) ;
#26288 = VECTOR ( 'NONE', #14271, 1000.000000000000000 ) ;
#26289 = ORIENTED_EDGE ( 'NONE', *, *, #17620, .F. ) ;
#26290 = CARTESIAN_POINT ( 'NONE',  ( 5.303645853345010153, 19.30241027580586177, 20.34789198813115263 ) ) ;
#26291 = AXIS2_PLACEMENT_3D ( 'NONE', #9826, #26198, #303 ) ;
#26292 = CARTESIAN_POINT ( 'NONE',  ( -2.959227181723746547, 8.499586724479465616, 21.50000000000000000 ) ) ;
#26293 = AXIS2_PLACEMENT_3D ( 'NONE', #1344, #1194, #15679 ) ;
#26294 = CARTESIAN_POINT ( 'NONE',  ( -17.09865819214518368, -39.97652765376174955, -16.50000000000000355 ) ) ;
#26295 = CARTESIAN_POINT ( 'NONE',  ( -38.30462971311529685, 8.019294621567119918, 35.00802478783429450 ) ) ;
#26296 = EDGE_LOOP ( 'NONE', ( #4193, #29468, #22785, #25622 ) ) ;
#26297 = CARTESIAN_POINT ( 'NONE',  ( 15.75094665830062723, -12.32508334119354210, 1.500000000000001332 ) ) ;
#26298 = ADVANCED_FACE ( 'NONE', ( #20946 ), #6158, .T. ) ;
#26299 = EDGE_CURVE ( 'NONE', #5590, #16236, #13949, .T. ) ;
#26300 = CARTESIAN_POINT ( 'NONE',  ( 33.26833594138172145, 9.291422874672347731, 36.21597341152490657 ) ) ;
#26301 = PLANE ( 'NONE',  #24791 ) ;
#26302 = AXIS2_PLACEMENT_3D ( 'NONE', #30506, #13842, #23173 ) ;
#26303 = VERTEX_POINT ( 'NONE', #14413 ) ;
#26304 = VECTOR ( 'NONE', #18488, 1000.000000000000000 ) ;
#26305 = CYLINDRICAL_SURFACE ( 'NONE', #30723, 0.7441270634456955690 ) ;
#26306 = DIRECTION ( 'NONE',  ( 0.000000000000000000, 0.000000000000000000, -1.000000000000000000 ) ) ;
#26307 = DIRECTION ( 'NONE',  ( 0.000000000000000000, 0.000000000000000000, -1.000000000000000000 ) ) ;
#26308 = CARTESIAN_POINT ( 'NONE',  ( 0.000000000000000000, 13.00000000000001421, 1.500000000000001332 ) ) ;
#26309 = CARTESIAN_POINT ( 'NONE',  ( -4.776122516674677878E-15, -42.50000000000000000, 27.50000000000000355 ) ) ;
#26310 = EDGE_CURVE ( 'NONE', #8541, #386, #7082, .T. ) ;
#26311 = CARTESIAN_POINT ( 'NONE',  ( -4.163336342344337027E-14, -1.387778780781445676E-14, 1.500000000000000000 ) ) ;
#26312 = CARTESIAN_POINT ( 'NONE',  ( -19.96096598928918908, 1.505335854884785274, 19.14333282897057842 ) ) ;
#26313 = DIRECTION ( 'NONE',  ( -1.000000000000000000, 0.000000000000000000, 0.000000000000000000 ) ) ;
#26314 = VERTEX_POINT ( 'NONE', #26255 ) ;
#26315 =( GEOMETRIC_REPRESENTATION_CONTEXT ( 3 ) GLOBAL_UNCERTAINTY_ASSIGNED_CONTEXT ( ( #1745 ) ) GLOBAL_UNIT_ASSIGNED_CONTEXT ( ( #891, #23970, #14468 ) ) REPRESENTATION_CONTEXT ( 'NONE', 'WORKASPACE' ) );
#26316 = AXIS2_PLACEMENT_3D ( 'NONE', #23600, #30789, #16912 ) ;
#26317 = DIRECTION ( 'NONE',  ( 0.000000000000000000, 0.000000000000000000, 1.000000000000000000 ) ) ;
#26318 = DIRECTION ( 'NONE',  ( -0.000000000000000000, -0.000000000000000000, 1.000000000000000000 ) ) ;
#26319 = AXIS2_PLACEMENT_3D ( 'NONE', #9977, #24146, #28850 ) ;
#26320 = EDGE_LOOP ( 'NONE', ( #1514, #22344, #17958, #9173 ) ) ;
#26321 = ORIENTED_EDGE ( 'NONE', *, *, #16974, .F. ) ;
#26322 = CARTESIAN_POINT ( 'NONE',  ( -49.93682080695227654, 70.00028624649445419, 53.79435855004096112 ) ) ;
#26323 = CARTESIAN_POINT ( 'NONE',  ( -14.49051644145457551, 47.85444022314150914, -51.09264228519022311 ) ) ;
#26324 = ORIENTED_EDGE ( 'NONE', *, *, #9991, .F. ) ;
#26325 = EDGE_CURVE ( 'NONE', #3062, #24994, #23916, .T. ) ;
#26326 = AXIS2_PLACEMENT_3D ( 'NONE', #12345, #14823, #163 ) ;
#26327 = DIRECTION ( 'NONE',  ( 1.000000000000000000, 0.000000000000000000, -0.000000000000000000 ) ) ;
#26328 = ADVANCED_FACE ( 'NONE', ( #24530 ), #5823, .F. ) ;
#26329 =( NAMED_UNIT ( * ) PLANE_ANGLE_UNIT ( ) SI_UNIT ( $, .RADIAN. ) );
#26330 = VERTEX_POINT ( 'NONE', #3024 ) ;
#26331 = EDGE_CURVE ( 'NONE', #23022, #580, #12008, .T. ) ;
#26332 = CARTESIAN_POINT ( 'NONE',  ( 31.76816150327698551, 26.51947378151753298, -11.49999299644477446 ) ) ;
#26333 = CARTESIAN_POINT ( 'NONE',  ( -15.84912786217080516, 12.19893545703369320, 19.96797677718664588 ) ) ;
#26334 = DIRECTION ( 'NONE',  ( -0.000000000000000000, -1.000000000000000000, -0.000000000000000000 ) ) ;
#26335 = ORIENTED_EDGE ( 'NONE', *, *, #28127, .T. ) ;
#26336 = DIRECTION ( 'NONE',  ( -0.000000000000000000, 0.000000000000000000, -1.000000000000000000 ) ) ;
#26337 = EDGE_CURVE ( 'NONE', #5196, #5082, #17552, .T. ) ;
#26338 = ORIENTED_EDGE ( 'NONE', *, *, #15125, .T. ) ;
#26339 = EDGE_CURVE ( 'NONE', #9285, #30374, #11077, .T. ) ;
#26340 = CIRCLE ( 'NONE', #2351, 0.7500000000000006661 ) ;
#26341 = CIRCLE ( 'NONE', #2931, 0.7500000000000006661 ) ;
#26342 = VECTOR ( 'NONE', #13532, 1000.000000000000114 ) ;
#26343 = ORIENTED_EDGE ( 'NONE', *, *, #21369, .T. ) ;
#26344 = EDGE_CURVE ( 'NONE', #16202, #11358, #23951, .T. ) ;
#26345 = CARTESIAN_POINT ( 'NONE',  ( 30.17204898946756586, 26.93709580362141409, 30.36897652752471188 ) ) ;
#26346 = CARTESIAN_POINT ( 'NONE',  ( -15.28186893989758310, 12.93018916568089338, 20.34789198813115263 ) ) ;
#26347 = AXIS2_PLACEMENT_3D ( 'NONE', #5881, #8545, #17581 ) ;
#26348 = ADVANCED_FACE ( 'NONE', ( #26892 ), #1061, .T. ) ;
#26349 = CARTESIAN_POINT ( 'NONE',  ( -10.32985675426556327, -17.14655349859505051, 18.37415474056476938 ) ) ;
#26350 = EDGE_CURVE ( 'NONE', #9106, #8430, #991, .T. ) ;
#26351 = DIRECTION ( 'NONE',  ( 1.000000000000000000, 2.081668171172166620E-14, 0.000000000000000000 ) ) ;
#26352 = CYLINDRICAL_SURFACE ( 'NONE', #13835, 0.7499999999999997780 ) ;
#26353 = CARTESIAN_POINT ( 'NONE',  ( -28.34828976096172681, 29.18752572968383419, 1.500000000000000000 ) ) ;
#26354 = CARTESIAN_POINT ( 'NONE',  ( 1.836970198721033928E-15, -15.00000000000004796, 29.43090101791767665 ) ) ;
#26355 = CIRCLE ( 'NONE', #11917, 12.66227964008302287 ) ;
#26356 = CARTESIAN_POINT ( 'NONE',  ( 24.44496207165490631, -7.595930209050163029, 45.15942333309103418 ) ) ;
#26357 = DIRECTION ( 'NONE',  ( 0.2817325568414296710, -0.9594929736144973687, 0.000000000000000000 ) ) ;
#26358 = VERTEX_POINT ( 'NONE', #3176 ) ;
#26359 = ORIENTED_EDGE ( 'NONE', *, *, #11225, .F. ) ;
#26360 = CARTESIAN_POINT ( 'NONE',  ( 12.50000000000000000, 1.530808498934191521E-15, -52.50000000000000000 ) ) ;
#26361 = DIRECTION ( 'NONE',  ( -0.000000000000000000, -0.000000000000000000, 1.000000000000000000 ) ) ;
#26362 = DIRECTION ( 'NONE',  ( -0.000000000000000000, -0.000000000000000000, 1.000000000000000000 ) ) ;
#26363 = CARTESIAN_POINT ( 'NONE',  ( 18.64567588040448598, -7.235161915364460405, 18.73377938172350099 ) ) ;
#26364 = DIRECTION ( 'NONE',  ( 1.000000000000000000, 0.000000000000000000, 0.000000000000000000 ) ) ;
#26365 = CIRCLE ( 'NONE', #5929, 9.084132297865673777 ) ;
#26366 = CARTESIAN_POINT ( 'NONE',  ( -29.06589025085023081, -23.33669524104240978, 27.50000000000000711 ) ) ;
#26367 = EDGE_CURVE ( 'NONE', #13653, #15949, #28441, .T. ) ;
#26368 = CARTESIAN_POINT ( 'NONE',  ( -5.027435569059562681, 19.35787894679208065, 6.386539667786100161 ) ) ;
#26369 = EDGE_LOOP ( 'NONE', ( #668, #6531, #13337, #24798 ) ) ;
#26370 = ADVANCED_FACE ( 'NONE', ( #24214 ), #5512, .F. ) ;
#26371 = CARTESIAN_POINT ( 'NONE',  ( 0.000000000000000000, 0.000000000000000000, 1.500000000000001332 ) ) ;
#26372 = AXIS2_PLACEMENT_3D ( 'NONE', #11381, #20874, #6073 ) ;
#26373 = CARTESIAN_POINT ( 'NONE',  ( -36.00000000000000000, -1.100768691257133318E-12, 34.75735931288076586 ) ) ;
#26374 = EDGE_CURVE ( 'NONE', #9927, #27254, #9577, .T. ) ;
#26375 = CARTESIAN_POINT ( 'NONE',  ( -1.687027447297492211, -8.840471615930066918, 21.50000000000000000 ) ) ;
#26376 = VERTEX_POINT ( 'NONE', #12699 ) ;
#26377 = CARTESIAN_POINT ( 'NONE',  ( 12.83215063165195424, 11.19227874472585960, 7.359006845440219102 ) ) ;
#26378 = EDGE_CURVE ( 'NONE', #3771, #13976, #3037, .T. ) ;
#26379 = ORIENTED_EDGE ( 'NONE', *, *, #22737, .T. ) ;
#26380 = CARTESIAN_POINT ( 'NONE',  ( 18.71580048965418186, -7.100988023106707736, 6.341840715582230281 ) ) ;
#26381 = EDGE_CURVE ( 'NONE', #30322, #18363, #20530, .T. ) ;
#26382 = DIRECTION ( 'NONE',  ( -0.000000000000000000, -0.000000000000000000, -1.000000000000000000 ) ) ;
#26383 = CIRCLE ( 'NONE', #12943, 0.7500000000000006661 ) ;
#26384 = DIRECTION ( 'NONE',  ( 1.000000000000000000, 0.000000000000000000, 0.000000000000000000 ) ) ;
#26385 = ORIENTED_EDGE ( 'NONE', *, *, #21926, .F. ) ;
#26386 = EDGE_CURVE ( 'NONE', #14711, #27939, #20471, .T. ) ;
#26387 = CARTESIAN_POINT ( 'NONE',  ( -4.163336342344337027E-14, 1.387778780781445676E-14, 1.500000000000000000 ) ) ;
#26388 = DIRECTION ( 'NONE',  ( 1.000000000000000000, 0.000000000000000000, 0.000000000000000000 ) ) ;
#26389 = DIRECTION ( 'NONE',  ( 0.000000000000000000, 0.000000000000000000, 1.000000000000000000 ) ) ;
#26390 = CARTESIAN_POINT ( 'NONE',  ( 0.000000000000000000, -2.435693370351110282E-15, 21.50000000000000355 ) ) ;
#26391 = CARTESIAN_POINT ( 'NONE',  ( -26.36764545593178255, -31.31467416275353344, 1.500000000000000000 ) ) ;
#26392 = CARTESIAN_POINT ( 'NONE',  ( -8.456776945386934585E-15, 29.50000000000000000, 43.10779406592839536 ) ) ;
#26393 = ORIENTED_EDGE ( 'NONE', *, *, #7533, .T. ) ;
#26394 = DIRECTION ( 'NONE',  ( 0.000000000000000000, 0.000000000000000000, -1.000000000000000000 ) ) ;
#26395 = AXIS2_PLACEMENT_3D ( 'NONE', #30320, #18482, #6469 ) ;
#26396 = CARTESIAN_POINT ( 'NONE',  ( 34.07766914600081520, 21.40380666527109810, -1.500000000000000000 ) ) ;
#26397 = CARTESIAN_POINT ( 'NONE',  ( 57.49999999999998579, 50.00000000000000000, -87.50000000000000000 ) ) ;
#26398 = VERTEX_POINT ( 'NONE', #24682 ) ;
#26399 = CARTESIAN_POINT ( 'NONE',  ( -37.16608720827707657, -65.00000000000000000, 12.49999999999999112 ) ) ;
#26400 = DIRECTION ( 'NONE',  ( -0.000000000000000000, 1.000000000000000000, 0.000000000000000000 ) ) ;
#26401 = CARTESIAN_POINT ( 'NONE',  ( 12.72536390617885438, -2.839914339433650348, 1.500000000000001332 ) ) ;
#26402 = EDGE_CURVE ( 'NONE', #10393, #23272, #13777, .T. ) ;
#26403 = CARTESIAN_POINT ( 'NONE',  ( 39.99999999999998579, 80.00000000000001421, 22.49999999999999289 ) ) ;
#26404 = ADVANCED_FACE ( 'NONE', ( #26581 ), #14708, .T. ) ;
#26405 = CIRCLE ( 'NONE', #19430, 17.00000000000000000 ) ;
#26406 = CARTESIAN_POINT ( 'NONE',  ( -23.96732207939035675, 33.98584080153585774, -1.500000000000000000 ) ) ;
#26407 = ORIENTED_EDGE ( 'NONE', *, *, #4959, .T. ) ;
#26408 = DIRECTION ( 'NONE',  ( 0.000000000000000000, 0.000000000000000000, 1.000000000000000000 ) ) ;
#26409 = CARTESIAN_POINT ( 'NONE',  ( 21.70146777712312769, 30.67724188593774670, 37.49999999988722266 ) ) ;
#26410 = CARTESIAN_POINT ( 'NONE',  ( 19.56124041029250549, 4.166605025611198165, 6.919864475265779191 ) ) ;
#26411 = VERTEX_POINT ( 'NONE', #18295 ) ;
#26412 = ORIENTED_EDGE ( 'NONE', *, *, #6530, .F. ) ;
#26413 = CARTESIAN_POINT ( 'NONE',  ( -23.12263228470263243, -11.97179573940914921, 44.71970589514035765 ) ) ;
#26414 = DIRECTION ( 'NONE',  ( 1.000000000000000000, 0.000000000000000000, 0.000000000000000000 ) ) ;
#26415 = VERTEX_POINT ( 'NONE', #13478 ) ;
#26416 = ORIENTED_EDGE ( 'NONE', *, *, #20033, .T. ) ;
#26417 = CARTESIAN_POINT ( 'NONE',  ( -10.40347366321433675, -17.08171436691437961, 7.652108011868850923 ) ) ;
#26418 = ORIENTED_EDGE ( 'NONE', *, *, #9548, .F. ) ;
#26419 = AXIS2_PLACEMENT_3D ( 'NONE', #17001, #11713, #2513 ) ;
#26420 = ORIENTED_EDGE ( 'NONE', *, *, #25579, .F. ) ;
#26421 = EDGE_LOOP ( 'NONE', ( #7073, #27088, #9110, #5422 ) ) ;
#26422 = CARTESIAN_POINT ( 'NONE',  ( -0.2365265214052963694, -17.01953242238517916, 19.33715507985239412 ) ) ;
#26423 = CARTESIAN_POINT ( 'NONE',  ( -7.671865949551465391, -15.25812906914210565, 6.672349528511551497 ) ) ;
#26424 = CARTESIAN_POINT ( 'NONE',  ( 8.840471615930072247, -1.687027447297460236, 1.500000000000001332 ) ) ;
#26425 = CARTESIAN_POINT ( 'NONE',  ( 1.795183039316617268, -16.98367886218520795, 19.36813350477385143 ) ) ;
#26426 = EDGE_LOOP ( 'NONE', ( #28822, #3622, #18231, #12964 ) ) ;
#26427 = CARTESIAN_POINT ( 'NONE',  ( 19.64114023396890829, 37.13592150528549496, -1.500000000000003997 ) ) ;
#26428 = CARTESIAN_POINT ( 'NONE',  ( 23.27838112219106392, 36.10018657900367600, -16.50000600000000262 ) ) ;
#26429 = CARTESIAN_POINT ( 'NONE',  ( 11.91933518721469554, 12.21304923692660260, 18.56793045041961321 ) ) ;
#26430 = DIRECTION ( 'NONE',  ( 0.000000000000000000, 0.000000000000000000, -1.000000000000000000 ) ) ;
#26431 = ORIENTED_EDGE ( 'NONE', *, *, #16710, .T. ) ;
#26432 = CARTESIAN_POINT ( 'NONE',  ( 37.99999999999933920, 0.000000000000000000, 82.49999999999998579 ) ) ;
#26433 = CARTESIAN_POINT ( 'NONE',  ( -14.71441417907129434, -8.667509008793196301, 6.892848776733236704 ) ) ;
#26434 = CARTESIAN_POINT ( 'NONE',  ( -6.413028646417895828, 15.82458379172922314, 7.098451512883313441 ) ) ;
#26435 = CYLINDRICAL_SURFACE ( 'NONE', #11413, 5.000000000000004441 ) ;
#26436 = CARTESIAN_POINT ( 'NONE',  ( -18.28579658156515819, -8.145820804509366297, 18.49267272388512140 ) ) ;
#26437 = AXIS2_PLACEMENT_3D ( 'NONE', #21803, #16666, #4655 ) ;
#26438 = DIRECTION ( 'NONE',  ( -0.000000000000000000, -0.000000000000000000, 1.000000000000000000 ) ) ;
#26439 = EDGE_CURVE ( 'NONE', #28591, #7862, #29682, .T. ) ;
#26440 = ORIENTED_EDGE ( 'NONE', *, *, #7801, .T. ) ;
#26441 = VERTEX_POINT ( 'NONE', #20327 ) ;
#26442 =( BOUNDED_CURVE ( )  B_SPLINE_CURVE ( 3, ( #16794, #14754, #14611, #26309 ),
 .UNSPECIFIED., .F., .T. ) 
 B_SPLINE_CURVE_WITH_KNOTS ( ( 4, 4 ),
 ( 0.000000000000000000, 3.141592653589793116 ),
 .UNSPECIFIED. ) 
 CURVE ( )  GEOMETRIC_REPRESENTATION_ITEM ( )  RATIONAL_B_SPLINE_CURVE ( ( 1.000000000000000000, 0.3333333333333333703, 0.3333333333333333703, 1.000000000000000000 ) ) 
 REPRESENTATION_ITEM ( '' )  );
#26443 = CARTESIAN_POINT ( 'NONE',  ( 7.500000000000000000, 5.196152422706624030, 9.000000000000001776 ) ) ;
#26444 = EDGE_CURVE ( 'NONE', #25866, #7224, #22458, .T. ) ;
#26445 = CARTESIAN_POINT ( 'NONE',  ( 40.89187623478217404, -5.790488632116400858, -19.50000000000000355 ) ) ;
#26446 = CARTESIAN_POINT ( 'NONE',  ( -14.68762770759668612, 13.60113105281362955, 6.755862304746362845 ) ) ;
#26447 = FACE_OUTER_BOUND ( 'NONE', #23499, .T. ) ;
#26448 = EDGE_LOOP ( 'NONE', ( #4726, #9605 ) ) ;
#26449 = APPLICATION_PROTOCOL_DEFINITION ( 'draft international standard', 'automotive_design', 1998, #3601 ) ;
#26450 = CARTESIAN_POINT ( 'NONE',  ( 16.14824862690563378, -5.544579173785682435, 19.85459532544248162 ) ) ;
#26451 = CARTESIAN_POINT ( 'NONE',  ( 1.000000000000008438, 13.00000000000001421, 1.500000000000001332 ) ) ;
#26452 = ORIENTED_EDGE ( 'NONE', *, *, #27487, .T. ) ;
#26453 = CARTESIAN_POINT ( 'NONE',  ( 4.659914667891703388, 16.37914622779766916, 20.12545155307891065 ) ) ;
#26454 = DIRECTION ( 'NONE',  ( 0.3598999890241654231, 0.9329908884337539954, 0.000000000000000000 ) ) ;
#26455 = CARTESIAN_POINT ( 'NONE',  ( -7.700393225232525118, -15.24241778594406327, 19.08844262864050023 ) ) ;
#26456 = CARTESIAN_POINT ( 'NONE',  ( -36.51119354604474410, 15.00142784232802740, 34.85629366384495853 ) ) ;
#26457 = VERTEX_POINT ( 'NONE', #16105 ) ;
#26458 = DIRECTION ( 'NONE',  ( 1.000000000000000000, 0.000000000000000000, 0.000000000000000000 ) ) ;
#26459 = VECTOR ( 'NONE', #208, 1000.000000000000000 ) ;
#26460 = CARTESIAN_POINT ( 'NONE',  ( 26.31795596221988376, 10.51822134874671022, -1.500000000000000000 ) ) ;
#26461 = VECTOR ( 'NONE', #11517, 1000.000000000000000 ) ;
#26462 = CARTESIAN_POINT ( 'NONE',  ( 8.264668169643783813, 43.16767620126012872, -16.50000000000000000 ) ) ;
#26463 = VERTEX_POINT ( 'NONE', #27506 ) ;
#26464 = CARTESIAN_POINT ( 'NONE',  ( -15.55925901137642064, -6.904021205104067249, 6.974106381145714018 ) ) ;
#26465 = CARTESIAN_POINT ( 'NONE',  ( 14.27394986618626582, 14.00917565527015896, 6.149077423860691560 ) ) ;
#26466 = CARTESIAN_POINT ( 'NONE',  ( 0.2396382576306479717, -20.01636569787185138, 5.657991946698900598 ) ) ;
#26467 = CARTESIAN_POINT ( 'NONE',  ( -8.840471615930058036, 1.687027447297517080, -1.500000000000001776 ) ) ;
#26468 = DIRECTION ( 'NONE',  ( 1.000000000000000000, 0.000000000000000000, 0.000000000000000000 ) ) ;
#26469 = CARTESIAN_POINT ( 'NONE',  ( 69.99999999999998579, -50.00000000000000000, 59.49999999999999289 ) ) ;
#26470 = FACE_OUTER_BOUND ( 'NONE', #15517, .T. ) ;
#26471 = ORIENTED_EDGE ( 'NONE', *, *, #2163, .F. ) ;
#26472 = CARTESIAN_POINT ( 'NONE',  ( -26.31094384852241319, 8.315730187098489878, -16.55003854064094426 ) ) ;
#26473 = CARTESIAN_POINT ( 'NONE',  ( 2.338573377552017440, 39.50000000000000711, 34.80090346875810781 ) ) ;
#26474 = EDGE_LOOP ( 'NONE', ( #27512, #17896, #6145, #26923 ) ) ;
#26475 = ORIENTED_EDGE ( 'NONE', *, *, #19093, .F. ) ;
#26476 = CARTESIAN_POINT ( 'NONE',  ( -26.44644203219470668, 9.801837641955994940, 1.500000000000000000 ) ) ;
#26477 = CARTESIAN_POINT ( 'NONE',  ( -12.73485997267505354, 48.35185223527960119, -62.94106308776442660 ) ) ;
#26478 = B_SPLINE_CURVE_WITH_KNOTS ( 'NONE', 3,
 ( #23096, #28101, #6722, #16234, #17154, #7800, #26523, #26373 ),
 .UNSPECIFIED., .F., .F.,
 ( 4, 2, 2, 4 ),
 ( 0.000000000000000000, 0.005288043134231363955, 0.007932064701347045499, 0.01057608626846272791 ),
 .UNSPECIFIED. ) ;
#26479 = SHAPE_REPRESENTATION_RELATIONSHIP ( 'NONE' , 'NONE' ,  #10497, #6874 ) ;
#26480 = ORIENTED_EDGE ( 'NONE', *, *, #26210, .F. ) ;
#26481 = VECTOR ( 'NONE', #18038, 1000.000000000000000 ) ;
#26482 = CARTESIAN_POINT ( 'NONE',  ( 7.869584159753955532, 10.39565510934977333, 1.500000000000001332 ) ) ;
#26483 = DIRECTION ( 'NONE',  ( 0.000000000000000000, 0.000000000000000000, 1.000000000000000000 ) ) ;
#26484 = ORIENTED_EDGE ( 'NONE', *, *, #24666, .T. ) ;
#26485 = CARTESIAN_POINT ( 'NONE',  ( 18.59495189863232412, -7.412450086248064451, 20.13759033520874908 ) ) ;
#26486 = DIRECTION ( 'NONE',  ( 0.6707505147970089787, -0.7416830501633076000, 0.000000000000000000 ) ) ;
#26487 = DIRECTION ( 'NONE',  ( -1.000000000000000000, 0.000000000000000000, 0.000000000000000000 ) ) ;
#26488 = ORIENTED_EDGE ( 'NONE', *, *, #26648, .T. ) ;
#26489 = CARTESIAN_POINT ( 'NONE',  ( 23.59634279088906439, -12.86962927293163084, 43.87962907659681377 ) ) ;
#26490 = VERTEX_POINT ( 'NONE', #25313 ) ;
#26491 = AXIS2_PLACEMENT_3D ( 'NONE', #27900, #6523, #22580 ) ;
#26492 = ORIENTED_EDGE ( 'NONE', *, *, #15630, .F. ) ;
#26493 = CARTESIAN_POINT ( 'NONE',  ( 18.35592613994001709, 37.52326638810179560, 29.29232531120126737 ) ) ;
#26494 = FACE_OUTER_BOUND ( 'NONE', #7984, .T. ) ;
#26495 = FACE_OUTER_BOUND ( 'NONE', #15210, .T. ) ;
#26496 = CIRCLE ( 'NONE', #12554, 9.084132297865673777 ) ;
#26497 = LINE ( 'NONE', #15095, #16227 ) ;
#26498 = CARTESIAN_POINT ( 'NONE',  ( -26.83043119477639493, -8.695877139419037505, -1.500000000000000000 ) ) ;
#26499 = LINE ( 'NONE', #24311, #18498 ) ;
#26500 = DIRECTION ( 'NONE',  ( -1.000000000000000000, 0.000000000000000000, 0.000000000000000000 ) ) ;
#26501 = EDGE_CURVE ( 'NONE', #26722, #8522, #8791, .T. ) ;
#26502 = ORIENTED_EDGE ( 'NONE', *, *, #15844, .F. ) ;
#26503 = EDGE_CURVE ( 'NONE', #28158, #7938, #113, .T. ) ;
#26504 = CARTESIAN_POINT ( 'NONE',  ( 10.30179067644846747, -17.16362715220463997, 6.974106381145714018 ) ) ;
#26505 = DIRECTION ( 'NONE',  ( 0.000000000000000000, -0.000000000000000000, 1.000000000000000000 ) ) ;
#26506 = DIRECTION ( 'NONE',  ( -0.000000000000000000, -0.000000000000000000, 1.000000000000000000 ) ) ;
#26507 = ORIENTED_EDGE ( 'NONE', *, *, #30549, .T. ) ;
#26508 = ORIENTED_EDGE ( 'NONE', *, *, #21750, .F. ) ;
#26509 = APPLICATION_CONTEXT ( 'automotive_design' ) ;
#26510 = DIRECTION ( 'NONE',  ( -1.000000000000000000, 0.000000000000000000, -0.000000000000000000 ) ) ;
#26511 = ADVANCED_FACE ( 'NONE', ( #13763 ), #8632, .T. ) ;
#26512 = CARTESIAN_POINT ( 'NONE',  ( -31.31394823341756251, 25.51108937476248428, -1.500000000000009992 ) ) ;
#26513 = ADVANCED_FACE ( 'NONE', ( #1906 ), #10813, .F. ) ;
#26514 = AXIS2_PLACEMENT_3D ( 'NONE', #10363, #29233, #2575 ) ;
#26515 = CARTESIAN_POINT ( 'NONE',  ( 18.57491549710361767, -7.414944001931020878, 20.15039051365864609 ) ) ;
#26516 = CARTESIAN_POINT ( 'NONE',  ( -15.27573937290510031, -7.547610621728815694, 5.676815824193227833 ) ) ;
#26517 = CARTESIAN_POINT ( 'NONE',  ( -5.199332475351345906, 19.31257985896675677, 6.033082186765055255 ) ) ;
#26518 = EDGE_CURVE ( 'NONE', #6039, #10630, #3639, .T. ) ;
#26519 = VERTEX_POINT ( 'NONE', #8325 ) ;
#26520 = ORIENTED_EDGE ( 'NONE', *, *, #5959, .T. ) ;
#26521 = CYLINDRICAL_SURFACE ( 'NONE', #6759, 20.32284676574536064 ) ;
#26522 = ADVANCED_FACE ( 'NONE', ( #25625 ), #23259, .T. ) ;
#26523 = CARTESIAN_POINT ( 'NONE',  ( -36.00000000000002842, 0.8865895960648689789, 34.75735931288077296 ) ) ;
#26524 = CARTESIAN_POINT ( 'NONE',  ( 0.000000000000000000, -2.435693370351110282E-15, 21.50000000000000355 ) ) ;
#26525 = VERTEX_POINT ( 'NONE', #11124 ) ;
#26526 = ADVANCED_FACE ( 'NONE', ( #17841 ), #15481, .T. ) ;
#26527 = CARTESIAN_POINT ( 'NONE',  ( 15.19061449783604623, 13.03728791304909329, 7.557577766377196582 ) ) ;
#26528 = ORIENTED_EDGE ( 'NONE', *, *, #2529, .F. ) ;
#26529 = CARTESIAN_POINT ( 'NONE',  ( 15.87141697993283529, -6.228091237695526416, 7.643931100913408550 ) ) ;
#26530 = CARTESIAN_POINT ( 'NONE',  ( 16.70031948171297387, 3.459335818475211877, 18.34938820207544907 ) ) ;
#26531 = CARTESIAN_POINT ( 'NONE',  ( 1.000000000000008438, 16.48749217771910125, 24.50000000000000000 ) ) ;
#26532 = ORIENTED_EDGE ( 'NONE', *, *, #17597, .F. ) ;
#26533 = CIRCLE ( 'NONE', #3628, 23.20393738267273420 ) ;
#26534 = VECTOR ( 'NONE', #24342, 1000.000000000000000 ) ;
#26535 = CARTESIAN_POINT ( 'NONE',  ( 77.99999999999998579, -42.50000000000001421, 1.500000000000000222 ) ) ;
#26536 = VECTOR ( 'NONE', #5876, 1000.000000000000000 ) ;
#26537 = DIRECTION ( 'NONE',  ( 0.7416830501633076000, -0.6707505147970089787, 0.000000000000000000 ) ) ;
#26538 = DIRECTION ( 'NONE',  ( -1.000000000000000000, 0.000000000000000000, 0.000000000000000000 ) ) ;
#26539 = CARTESIAN_POINT ( 'NONE',  ( 0.000000000000000000, -7.422978769709303177E-15, 65.52304386563415051 ) ) ;
#26540 = FACE_OUTER_BOUND ( 'NONE', #24675, .T. ) ;
#26541 = CARTESIAN_POINT ( 'NONE',  ( 10.83311381505435023, -16.83321666392360427, 20.29090034784956131 ) ) ;
#26542 = CARTESIAN_POINT ( 'NONE',  ( 10.25394813640221336, -17.17138746996170795, 19.47728749465737863 ) ) ;
#26543 = EDGE_CURVE ( 'NONE', #14704, #29877, #5038, .T. ) ;
#26544 = ORIENTED_EDGE ( 'NONE', *, *, #429, .F. ) ;
#26545 = EDGE_CURVE ( 'NONE', #18139, #11207, #12507, .T. ) ;
#26546 = CARTESIAN_POINT ( 'NONE',  ( 126.5359999999999872, 0.000000000000000000, 6.000000000000001776 ) ) ;
#26547 = EDGE_CURVE ( 'NONE', #15589, #9342, #23415, .T. ) ;
#26548 = CARTESIAN_POINT ( 'NONE',  ( -20.65888525914099105, 38.75220717792564784, -19.50000000000000355 ) ) ;
#26549 = DIRECTION ( 'NONE',  ( 1.000000000000000000, 0.000000000000000000, 0.000000000000000000 ) ) ;
#26550 = EDGE_CURVE ( 'NONE', #14452, #17402, #21068, .T. ) ;
#26551 = ORIENTED_EDGE ( 'NONE', *, *, #4046, .F. ) ;
#26552 = CARTESIAN_POINT ( 'NONE',  ( 39.99999999999998579, 87.00000000000001421, 22.49999999999999289 ) ) ;
#26553 = CYLINDRICAL_SURFACE ( 'NONE', #29674, 1.999999999999998224 ) ;
#26554 = ADVANCED_FACE ( 'NONE', ( #30444 ), #26068, .F. ) ;
#26555 = CARTESIAN_POINT ( 'NONE',  ( 3.196529495465388226, 8.413215745755008967, 21.50000000000000000 ) ) ;
#26556 = CARTESIAN_POINT ( 'NONE',  ( -0.8762659238204844048, -8.999114229549588728, -1.500000000000002665 ) ) ;
#26557 = CARTESIAN_POINT ( 'NONE',  ( -25.19442432475839055, 35.44676296258369064, -19.50000000000000355 ) ) ;
#26558 = EDGE_CURVE ( 'NONE', #30078, #12825, #9506, .T. ) ;
#26559 = FILL_AREA_STYLE_COLOUR ( '', #21352 ) ;
#26560 = CIRCLE ( 'NONE', #30534, 1.000000000000008438 ) ;
#26561 = CARTESIAN_POINT ( 'NONE',  ( 34.26660261194440693, 20.46295234328604096, 31.03790124022056318 ) ) ;
#26562 = EDGE_CURVE ( 'NONE', #14218, #20523, #168, .T. ) ;
#26564 = CIRCLE ( 'NONE', #3140, 21.71568325578132530 ) ;
#26563 = FACE_OUTER_BOUND ( 'NONE', #16910, .T. ) ;
#26565 = ORIENTED_EDGE ( 'NONE', *, *, #18571, .T. ) ;
#26566 = CARTESIAN_POINT ( 'NONE',  ( 7.706848733600955015, 5.524309650260791571, 21.50000000000000000 ) ) ;
#26567 = ORIENTED_EDGE ( 'NONE', *, *, #19528, .T. ) ;
#26568 = CYLINDRICAL_SURFACE ( 'NONE', #25666, 0.7441270634457163302 ) ;
#26569 = CARTESIAN_POINT ( 'NONE',  ( 14.87898868866547097, 13.36471831362574747, 5.652196082369964181 ) ) ;
#26570 = ORIENTED_EDGE ( 'NONE', *, *, #8098, .T. ) ;
#26571 = CIRCLE ( 'NONE', #16606, 0.7500000000000006661 ) ;
#26572 = ORIENTED_EDGE ( 'NONE', *, *, #29930, .F. ) ;
#26573 = LINE ( 'NONE', #19393, #6801 ) ;
#26574 = VERTEX_POINT ( 'NONE', #28262 ) ;
#26575 = VERTEX_POINT ( 'NONE', #14524 ) ;
#26576 = ORIENTED_EDGE ( 'NONE', *, *, #2683, .F. ) ;
#26577 = CARTESIAN_POINT ( 'NONE',  ( -0.08122345276805303937, -17.02407875822364147, 19.87181966307587544 ) ) ;
#26578 = EDGE_CURVE ( 'NONE', #19648, #29034, #23, .T. ) ;
#26579 = CARTESIAN_POINT ( 'NONE',  ( -32.02118151871192708, 18.16475142757035144, 34.49999999999999289 ) ) ;
#26580 = AXIS2_PLACEMENT_3D ( 'NONE', #13768, #29860, #13484 ) ;
#26581 = FACE_OUTER_BOUND ( 'NONE', #13544, .T. ) ;
#26582 = EDGE_CURVE ( 'NONE', #4264, #16453, #4469, .T. ) ;
#26583 = CIRCLE ( 'NONE', #673, 37.50000000000001421 ) ;
#26584 = CARTESIAN_POINT ( 'NONE',  ( -8.499586724479453181, -2.959227181723774525, 1.500000000000001332 ) ) ;
#26585 = CARTESIAN_POINT ( 'NONE',  ( -20.78475560873934569, 25.06838084537526612, -16.50001200000000168 ) ) ;
#26586 = ORIENTED_EDGE ( 'NONE', *, *, #1389, .T. ) ;
#26587 = VECTOR ( 'NONE', #8578, 1000.000000000000000 ) ;
#26588 = CYLINDRICAL_SURFACE ( 'NONE', #12387, 1.000000000000008438 ) ;
#26589 = CARTESIAN_POINT ( 'NONE',  ( -2.081668171172168513E-14, 75.00000000000001421, 37.49999999999999289 ) ) ;
#26590 = CARTESIAN_POINT ( 'NONE',  ( 14.34755844633281718, 13.95901041572539469, 18.73743063545763121 ) ) ;
#26591 = ORIENTED_EDGE ( 'NONE', *, *, #26149, .F. ) ;
#26592 = FACE_OUTER_BOUND ( 'NONE', #23016, .T. ) ;
#26593 = CARTESIAN_POINT ( 'NONE',  ( -14.83655028254229968, -8.438271213925730763, 5.951255046771932733 ) ) ;
#26594 = CARTESIAN_POINT ( 'NONE',  ( -6.240920525956804354, 15.88642679632095955, 5.951255046771932733 ) ) ;
#26595 = CARTESIAN_POINT ( 'NONE',  ( 39.52380524535562500, 7.028748154183637631, -11.49999999999999645 ) ) ;
#26596 = CARTESIAN_POINT ( 'NONE',  ( -23.36055057548231417, 12.54866584153426423, 44.23986152793528248 ) ) ;
#26597 = CARTESIAN_POINT ( 'NONE',  ( -4.163336342344337027E-14, 1.387778780781445676E-14, 24.50000000000000000 ) ) ;
#26598 = CARTESIAN_POINT ( 'NONE',  ( -8.550548372801092256, -14.74545326687210611, 7.652108011868850923 ) ) ;
#26599 = ORIENTED_EDGE ( 'NONE', *, *, #16662, .F. ) ;
#26600 = VERTEX_POINT ( 'NONE', #24022 ) ;
#26601 = DIRECTION ( 'NONE',  ( 1.000000000000000000, 0.000000000000000000, 0.000000000000000000 ) ) ;
#26602 = CARTESIAN_POINT ( 'NONE',  ( 25.19442432474404470, 35.44676296256560022, -19.50000000000000355 ) ) ;
#26603 = FACE_OUTER_BOUND ( 'NONE', #26277, .T. ) ;
#26604 = CARTESIAN_POINT ( 'NONE',  ( 30.31220697679117038, 11.23460505553742550, 1.500000000000000000 ) ) ;
#26605 = ORIENTED_EDGE ( 'NONE', *, *, #27671, .F. ) ;
#26606 = APPLICATION_PROTOCOL_DEFINITION ( 'draft international standard', 'automotive_design', 1998, #29700 ) ;
#26607 = CARTESIAN_POINT ( 'NONE',  ( -38.00000000000000000, 80.00000000000000000, -7.533656238527846826E-15 ) ) ;
#26608 = CARTESIAN_POINT ( 'NONE',  ( 7.500000000000000000, 9.184850993605147944E-16, -1.500000000000001332 ) ) ;
#26609 = AXIS2_PLACEMENT_3D ( 'NONE', #4258, #16426, #21086 ) ;
#26610 = ORIENTED_EDGE ( 'NONE', *, *, #23049, .T. ) ;
#26611 = CARTESIAN_POINT ( 'NONE',  ( 6.262709072525339593, 19.01302309856007966, 19.22654678686458141 ) ) ;
#26612 = CIRCLE ( 'NONE', #13162, 0.7499999999999997780 ) ;
#26613 = DIRECTION ( 'NONE',  ( -0.000000000000000000, 1.000000000000000000, -0.000000000000000000 ) ) ;
#26614 = FACE_OUTER_BOUND ( 'NONE', #1485, .T. ) ;
#26615 = CARTESIAN_POINT ( 'NONE',  ( -36.33684937716974872, -15.65606802492079730, 31.48606577064049006 ) ) ;
#26616 = ORIENTED_EDGE ( 'NONE', *, *, #29545, .T. ) ;
#26617 = DIRECTION ( 'NONE',  ( 0.000000000000000000, 1.132880637372608986E-16, -1.000000000000000000 ) ) ;
#26618 = EDGE_CURVE ( 'NONE', #34, #16268, #18082, .T. ) ;
#26619 = CARTESIAN_POINT ( 'NONE',  ( 33.56327786402390245, 10.34181101807379299, 35.63689980405264635 ) ) ;
#26620 = CARTESIAN_POINT ( 'NONE',  ( 9.785366065393095170, 42.77971715303853273, -16.49999999999999645 ) ) ;
#26621 = EDGE_LOOP ( 'NONE', ( #16719, #14978, #19055, #12426 ) ) ;
#26622 = CARTESIAN_POINT ( 'NONE',  ( -18.41515300997268056, -7.848447721146238010, 7.176035686813569292 ) ) ;
#26623 = FACE_OUTER_BOUND ( 'NONE', #26320, .T. ) ;
#26624 = DIRECTION ( 'NONE',  ( -1.000000000000000000, 0.000000000000000000, -0.000000000000000000 ) ) ;
#26625 = CARTESIAN_POINT ( 'NONE',  ( -70.00000000000000000, 65.00000000000000000, 12.49999999999999112 ) ) ;
#26626 = CARTESIAN_POINT ( 'NONE',  ( 6.778663211761462470, -6.630478080506934546, 21.50000000000000000 ) ) ;
#26627 = CARTESIAN_POINT ( 'NONE',  ( 33.78553947564427773, -24.40792753551981775, -16.50000000000000000 ) ) ;
#26628 = AXIS2_PLACEMENT_3D ( 'NONE', #24324, #24946, #7795 ) ;
#26629 = CARTESIAN_POINT ( 'NONE',  ( 6.543385983536347261, 6.301234758012619785, -1.500000000000001110 ) ) ;
#26630 = CARTESIAN_POINT ( 'NONE',  ( 0.000000000000000000, 0.000000000000000000, 21.50000000000000000 ) ) ;
#26631 = VERTEX_POINT ( 'NONE', #25917 ) ;
#26632 = CARTESIAN_POINT ( 'NONE',  ( 37.99999999999999289, 70.00000000000000000, -75.50000000000001421 ) ) ;
#26633 = DIRECTION ( 'NONE',  ( -0.000000000000000000, -0.000000000000000000, 1.000000000000000000 ) ) ;
#26634 = ORIENTED_EDGE ( 'NONE', *, *, #20420, .F. ) ;
#26635 = ORIENTED_EDGE ( 'NONE', *, *, #9738, .T. ) ;
#26636 = DIRECTION ( 'NONE',  ( 0.000000000000000000, 1.224646799147354933E-16, 1.000000000000000000 ) ) ;
#26637 = CARTESIAN_POINT ( 'NONE',  ( -14.61253163965172952, 47.81719550270585728, -51.57679968430688433 ) ) ;
#26638 = VERTEX_POINT ( 'NONE', #16403 ) ;
#26639 = CARTESIAN_POINT ( 'NONE',  ( 15.42025756663164948, 12.76459690492384880, 19.96783386855779341 ) ) ;
#26640 = CARTESIAN_POINT ( 'NONE',  ( -9.159129059799164807, -14.35414742152909717, 7.359006845440219102 ) ) ;
#26641 = VERTEX_POINT ( 'NONE', #2051 ) ;
#26642 = CARTESIAN_POINT ( 'NONE',  ( -29.99999999999933209, 1.755172820525642916E-14, 67.49999999999997158 ) ) ;
#26643 = CARTESIAN_POINT ( 'NONE',  ( 19.74834695364560844, 3.274018421667484802, 18.34838970509067479 ) ) ;
#26644 = CYLINDRICAL_SURFACE ( 'NONE', #25, 28.20443790117963800 ) ;
#26645 = ORIENTED_EDGE ( 'NONE', *, *, #8838, .T. ) ;
#26646 = AXIS2_PLACEMENT_3D ( 'NONE', #12375, #350, #22025 ) ;
#26647 = EDGE_LOOP ( 'NONE', ( #19758, #12484, #3229, #14224, #28167 ) ) ;
#26648 = EDGE_CURVE ( 'NONE', #2787, #24319, #23528, .T. ) ;
#26649 = VERTEX_POINT ( 'NONE', #6735 ) ;
#26650 = CARTESIAN_POINT ( 'NONE',  ( 17.21962637186833334, 38.15825840448668771, 29.23201136369613451 ) ) ;
#26651 = CARTESIAN_POINT ( 'NONE',  ( -6.936828876846347747, 18.77725343618825349, 19.36813350477385143 ) ) ;
#26652 = CARTESIAN_POINT ( 'NONE',  ( -14.68762770759668257, 13.60113105281362955, 19.45164628100866722 ) ) ;
#26653 = AXIS2_PLACEMENT_3D ( 'NONE', #9709, #28747, #14398 ) ;
#26654 = CARTESIAN_POINT ( 'NONE',  ( -9.648244442396764597, -17.53899143774386715, 19.36813350477385143 ) ) ;
#26655 = CARTESIAN_POINT ( 'NONE',  ( -38.85201932933775026, 3.754465866770057225, 32.18529919512457127 ) ) ;
#26656 = DIRECTION ( 'NONE',  ( 1.000000000000000000, 0.000000000000000000, 0.000000000000000000 ) ) ;
#26657 = DIRECTION ( 'NONE',  ( -0.000000000000000000, 0.000000000000000000, 1.000000000000000000 ) ) ;
#26658 = ORIENTED_EDGE ( 'NONE', *, *, #12059, .F. ) ;
#26659 = CARTESIAN_POINT ( 'NONE',  ( 9.582629137048309431, -14.08615220418401215, 5.701226463332907279 ) ) ;
#26660 = CARTESIAN_POINT ( 'NONE',  ( -32.05716845166662665, 24.22161781167242722, 8.060878346463965727 ) ) ;
#26661 = CARTESIAN_POINT ( 'NONE',  ( 19.87925100141003654, 2.194397331962206987, 6.518927109361849936 ) ) ;
#26662 = VERTEX_POINT ( 'NONE', #2205 ) ;
#26663 = ORIENTED_EDGE ( 'NONE', *, *, #3856, .T. ) ;
#26664 = AXIS2_PLACEMENT_3D ( 'NONE', #5304, #156, #24162 ) ;
#26665 = CARTESIAN_POINT ( 'NONE',  ( 17.99898938545033289, -8.720395568141155351, 19.96302680909623817 ) ) ;
#26666 = DIRECTION ( 'NONE',  ( 1.000000000000000000, 0.000000000000000000, 0.000000000000000000 ) ) ;
#26667 = CYLINDRICAL_SURFACE ( 'NONE', #19835, 20.00000000000000000 ) ;
#26668 = CARTESIAN_POINT ( 'NONE',  ( -15.37673962019508522, -7.325595981656019440, 5.774779864094946369 ) ) ;
#26669 = FACE_OUTER_BOUND ( 'NONE', #3656, .T. ) ;
#26670 = LINE ( 'NONE', #3123, #4951 ) ;
#26671 = VERTEX_POINT ( 'NONE', #4699 ) ;
#26672 = CARTESIAN_POINT ( 'NONE',  ( -20.76850923836823526, -32.27873595568063081, 34.50000000000000000 ) ) ;
#26673 =( GEOMETRIC_REPRESENTATION_CONTEXT ( 3 ) GLOBAL_UNCERTAINTY_ASSIGNED_CONTEXT ( ( #28562 ) ) GLOBAL_UNIT_ASSIGNED_CONTEXT ( ( #18067, #12766, #29460 ) ) REPRESENTATION_CONTEXT ( 'NONE', 'WORKASPACE' ) );
#26674 = DIRECTION ( 'NONE',  ( 0.000000000000000000, 1.000000000000000000, 1.193512090021232842E-16 ) ) ;
#26675 = ADVANCED_FACE ( 'NONE', ( #9231 ), #18746, .F. ) ;
#26676 = CARTESIAN_POINT ( 'NONE',  ( 14.87898868866547097, 13.36471831362575102, 18.34798005863227388 ) ) ;
#26677 = VERTEX_POINT ( 'NONE', #14054 ) ;
#26678 = CARTESIAN_POINT ( 'NONE',  ( 15.04974025769138990, 13.19961543621590572, 7.632642797338977658 ) ) ;
#26679 = EDGE_LOOP ( 'NONE', ( #19768, #15248, #20680, #29795 ) ) ;
#26680 = FACE_OUTER_BOUND ( 'NONE', #7570, .T. ) ;
#26681 = UNCERTAINTY_MEASURE_WITH_UNIT (LENGTH_MEASURE( 1.000000000000000082E-05 ), #27417, 'distance_accuracy_value', 'NONE');
#26682 = CARTESIAN_POINT ( 'NONE',  ( -33.67904612011425058, 24.24635139330486311, -14.83330431405463656 ) ) ;
#26683 = CARTESIAN_POINT ( 'NONE',  ( -18.58529988941444699, 7.388276390372320535, 24.50000000000000000 ) ) ;
#26684 = ORIENTED_EDGE ( 'NONE', *, *, #19265, .T. ) ;
#26685 = AXIS2_PLACEMENT_3D ( 'NONE', #17655, #798, #22013 ) ;
#26686 = CARTESIAN_POINT ( 'NONE',  ( 0.000000000000000000, 42.50000000000000000, 1.500000000000000000 ) ) ;
#26687 = EDGE_CURVE ( 'NONE', #12864, #13348, #9321, .T. ) ;
#26688 = CARTESIAN_POINT ( 'NONE',  ( -67.00000000000000000, 0.000000000000000000, 59.49999999999999289 ) ) ;
#26689 = CARTESIAN_POINT ( 'NONE',  ( -37.99999999999999289, 209.2686044187655909, -34.49999999999999289 ) ) ;
#26690 = CARTESIAN_POINT ( 'NONE',  ( 33.70141996666045259, 13.89393473031433324, 34.49999999999999289 ) ) ;
#26691 = CARTESIAN_POINT ( 'NONE',  ( -36.00000000000000000, -1.100768691257133318E-12, 34.75735931288076586 ) ) ;
#26692 = CARTESIAN_POINT ( 'NONE',  ( 10.38931136226422147, -17.11076273665785763, 19.87181966307587544 ) ) ;
#26693 = CARTESIAN_POINT ( 'NONE',  ( 0.8038475772933646457, 5.196152422706634688, -9.000000000000001776 ) ) ;
#26694 = VERTEX_POINT ( 'NONE', #21533 ) ;
#26695 = DIRECTION ( 'NONE',  ( -0.000000000000000000, -0.000000000000000000, -1.000000000000000000 ) ) ;
#26696 = DIRECTION ( 'NONE',  ( 0.000000000000000000, 1.000000000000000000, -0.000000000000000000 ) ) ;
#26697 = CARTESIAN_POINT ( 'NONE',  ( -2.552544030762004645, -42.50000000000000000, -1.500000000000000000 ) ) ;
#26698 = DIRECTION ( 'NONE',  ( 1.000000000000000000, 0.000000000000000000, 0.000000000000000000 ) ) ;
#26699 = VERTEX_POINT ( 'NONE', #12663 ) ;
#26700 = ADVANCED_FACE ( 'NONE', ( #5638 ), #29343, .T. ) ;
#26701 = B_SPLINE_CURVE_WITH_KNOTS ( 'NONE', 3,
 ( #3423, #29477, #19792, #12947, #10596, #26665, #17618, #20110, #29625, #17467, #14961, #8261, #17767, #27286, #24473, #3257, #5918, #26989 ),
 .UNSPECIFIED., .F., .F.,
 ( 4, 2, 2, 2, 2, 2, 2, 2, 4 ),
 ( 0.003174295595554365527, 0.003570702171545611300, 0.003967108747536857508, 0.004363515323528103715, 0.004759921899519349055, 0.005156328475510595262, 0.005552735051501840602, 0.005949141627493086809, 0.006345548203484333016 ),
 .UNSPECIFIED. ) ;
#26702 = CARTESIAN_POINT ( 'NONE',  ( 29.54401593347832744, -27.74630720509791004, 16.64138351564043461 ) ) ;
#26703 = LINE ( 'NONE', #5333, #22206 ) ;
#26704 = DIRECTION ( 'NONE',  ( -0.8349582046168341209, -0.5503133621338236470, 0.000000000000000000 ) ) ;
#26705 = CARTESIAN_POINT ( 'NONE',  ( -5.815855718377446415, -16.25752007041490188, -0.6213203435596476032 ) ) ;
#26706 = CARTESIAN_POINT ( 'NONE',  ( 12.56641067637628240, -40.32935944494942504, -1.500000000000000000 ) ) ;
#26707 = FACE_OUTER_BOUND ( 'NONE', #3922, .T. ) ;
#26708 = CIRCLE ( 'NONE', #30676, 0.7500000000000006661 ) ;
#26709 = CARTESIAN_POINT ( 'NONE',  ( 39.00460276462784748, -0.1210056128972753636, 35.08014749300483004 ) ) ;
#26710 = CARTESIAN_POINT ( 'NONE',  ( -2.209227181723746103, 8.499586724479465616, -1.500000000000000888 ) ) ;
#26711 = VERTEX_POINT ( 'NONE', #780 ) ;
#26712 = AXIS2_PLACEMENT_3D ( 'NONE', #6541, #21163, #1701 ) ;
#26713 = DIRECTION ( 'NONE',  ( -0.000000000000000000, -0.000000000000000000, -1.000000000000000000 ) ) ;
#26714 = ORIENTED_EDGE ( 'NONE', *, *, #10935, .T. ) ;
#26715 = FACE_OUTER_BOUND ( 'NONE', #21715, .T. ) ;
#26716 = CARTESIAN_POINT ( 'NONE',  ( 25.64627119138473432, 23.40052582045089480, -6.500000000000000888 ) ) ;
#26717 = ORIENTED_EDGE ( 'NONE', *, *, #21167, .T. ) ;
#26718 = EDGE_CURVE ( 'NONE', #10711, #16514, #19820, .T. ) ;
#26719 = ORIENTED_EDGE ( 'NONE', *, *, #7688, .T. ) ;
#26720 = EDGE_CURVE ( 'NONE', #9920, #19640, #13100, .T. ) ;
#26721 = DIRECTION ( 'NONE',  ( -0.000000000000000000, -0.000000000000000000, -1.000000000000000000 ) ) ;
#26722 = VERTEX_POINT ( 'NONE', #10303 ) ;
#26723 = ORIENTED_EDGE ( 'NONE', *, *, #29756, .F. ) ;
#26724 = CARTESIAN_POINT ( 'NONE',  ( -30.53339558441486190, -7.800891647352837133, 43.48653168448686301 ) ) ;
#26725=STYLED_ITEM('',(#30914),#2508);
#26726 = CARTESIAN_POINT ( 'NONE',  ( -42.49999999999998579, 50.00000000000000000, -87.50000000000000000 ) ) ;
#26727 = EDGE_CURVE ( 'NONE', #25497, #14711, #12812, .T. ) ;
#26728 = CARTESIAN_POINT ( 'NONE',  ( -8.413215745754975217, 3.196529495465474380, -1.500000000000001332 ) ) ;
#26729 = CARTESIAN_POINT ( 'NONE',  ( -32.98805937973593672, 22.67054169308932288, 8.000000000000003553 ) ) ;
#26730 = CARTESIAN_POINT ( 'NONE',  ( -14.58213539500865785, 7.758783772730382111, -0.6213203435596476032 ) ) ;
#26731 = ORIENTED_EDGE ( 'NONE', *, *, #10536, .T. ) ;
#26732 = EDGE_CURVE ( 'NONE', #13217, #11117, #17166, .T. ) ;
#26733 = CIRCLE ( 'NONE', #4301, 0.7500000000000006661 ) ;
#26734 = LINE ( 'NONE', #21428, #10901 ) ;
#26735 = CARTESIAN_POINT ( 'NONE',  ( 15.57266529552203416, -38.96488032230103471, 1.500000000000000000 ) ) ;
#26736 = CARTESIAN_POINT ( 'NONE',  ( 1.327349630778746237, -17.01025715289075890, 5.810767894563978686 ) ) ;
#26737 = LINE ( 'NONE', #24860, #19600 ) ;
#26738 = EDGE_CURVE ( 'NONE', #3711, #17402, #21168, .T. ) ;
#26739 = ORIENTED_EDGE ( 'NONE', *, *, #11751, .T. ) ;
#26740 = VECTOR ( 'NONE', #7280, 1000.000000000000000 ) ;
#26741 = VECTOR ( 'NONE', #7529, 1000.000000000000114 ) ;
#26742 = DIRECTION ( 'NONE',  ( 1.000000000000000000, 0.000000000000000000, -1.369518533665900312E-16 ) ) ;
#26743 = CARTESIAN_POINT ( 'NONE',  ( -14.72704883620386340, -8.644027383692558075, 6.341840715582230281 ) ) ;
#26744 = DIRECTION ( 'NONE',  ( -0.000000000000000000, -0.000000000000000000, -1.000000000000000000 ) ) ;
#26745 = ADVANCED_FACE ( 'NONE', ( #27158 ), #27010, .T. ) ;
#26746 = CARTESIAN_POINT ( 'NONE',  ( -23.21352257770656990, -10.78826658734919519, 49.40206402021038201 ) ) ;
#26747 = CARTESIAN_POINT ( 'NONE',  ( -15.53738272950673327, -6.955830428693968059, 18.90679857307105749 ) ) ;
#26748 = CARTESIAN_POINT ( 'NONE',  ( -4.102102735472397121, 8.549050687778208868, 21.50000000000000000 ) ) ;
#26749 = AXIS2_PLACEMENT_3D ( 'NONE', #20335, #10511, #19876 ) ;
#26750 = EDGE_LOOP ( 'NONE', ( #13526, #12598, #19017, #19545 ) ) ;
#26751 = EDGE_LOOP ( 'NONE', ( #3091, #22064, #26488, #7144 ) ) ;
#26752 = DIRECTION ( 'NONE',  ( 1.000000000000000000, 0.000000000000000000, 0.000000000000000000 ) ) ;
#26753 = CIRCLE ( 'NONE', #11801, 9.084132297865673777 ) ;
#26754 = CARTESIAN_POINT ( 'NONE',  ( -5.199332475351349458, 19.31257985896675322, 18.72886616302735163 ) ) ;
#26755 = CARTESIAN_POINT ( 'NONE',  ( 5.349779314757592275, 7.341751895053254096, -1.500000000000000888 ) ) ;
#26756 = CARTESIAN_POINT ( 'NONE',  ( 0.5197766397933876181, -17.03069205084988980, 5.676815824193226057 ) ) ;
#26757 = ORIENTED_EDGE ( 'NONE', *, *, #1735, .T. ) ;
#26758 = APPLICATION_PROTOCOL_DEFINITION ( 'draft international standard', 'automotive_design', 1998, #14576 ) ;
#26759 = CARTESIAN_POINT ( 'NONE',  ( 18.35307960222155899, -7.992235168165439774, 18.34798005862930736 ) ) ;
#26760 = CARTESIAN_POINT ( 'NONE',  ( -15.34618562042307843, 12.82554431217322310, 18.34798005863227388 ) ) ;
#26761 = AXIS2_PLACEMENT_3D ( 'NONE', #22001, #9847, #19653 ) ;
#26762 = EDGE_CURVE ( 'NONE', #19615, #30053, #16138, .T. ) ;
#26763 = ORIENTED_EDGE ( 'NONE', *, *, #17979, .T. ) ;
#26764 = DIRECTION ( 'NONE',  ( 0.000000000000000000, 1.000000000000000000, 1.132880637372608986E-16 ) ) ;
#26765 = ADVANCED_FACE ( 'NONE', ( #10464 ), #29497, .T. ) ;
#26766 = AXIS2_PLACEMENT_3D ( 'NONE', #27166, #14836, #10472 ) ;
#26767 = CARTESIAN_POINT ( 'NONE',  ( 9.249586724479433641, 2.959227181723830036, 21.50000000000000000 ) ) ;
#26768 = AXIS2_PLACEMENT_3D ( 'NONE', #7336, #16846, #7492 ) ;
#26769 = CARTESIAN_POINT ( 'NONE',  ( 1.073881485057738949, -0.9711784013061123266, -1.500000000000000000 ) ) ;
#26770 = ADVANCED_FACE ( 'NONE', ( #2826 ), #24809, .F. ) ;
#26771 = CARTESIAN_POINT ( 'NONE',  ( -39.07105923661990943, -0.5277388387263558522, 35.08714678962015654 ) ) ;
#26772 = ORIENTED_EDGE ( 'NONE', *, *, #29197, .T. ) ;
#26773 = CARTESIAN_POINT ( 'NONE',  ( 11.91798344328409875, -16.06126763266893320, 6.392525840300340434 ) ) ;
#26774 = CYLINDRICAL_SURFACE ( 'NONE', #20018, 0.7500000000000006661 ) ;
#26775 = CIRCLE ( 'NONE', #28254, 0.7500000000000003331 ) ;
#26776 = CARTESIAN_POINT ( 'NONE',  ( 21.79411701110929656, 37.18463376297794554, -16.49999999999999645 ) ) ;
#26777 = CARTESIAN_POINT ( 'NONE',  ( -50.00000000000000000, -67.00000000000000000, 59.49999999999999289 ) ) ;
#26778 = VECTOR ( 'NONE', #16377, 1000.000000000000000 ) ;
#26779 = ORIENTED_EDGE ( 'NONE', *, *, #22387, .F. ) ;
#26780 = CARTESIAN_POINT ( 'NONE',  ( -18.10797733959154243, -8.533081443083743167, 5.657991946698900598 ) ) ;
#26781 = FACE_BOUND ( 'NONE', #11405, .T. ) ;
#26782 = PLANE ( 'NONE',  #18779 ) ;
#26783 = CLOSED_SHELL ( 'NONE', ( #24767, #11304, #17210, #8236, #4971, #22973, #10301, #29596, #8047, #27095, #24962, #1733, #14511, #13770, #23296, #19470, #30315, #5965, #27149, #22346, #16672, #28069, #6843, #14471, #28604, #24134, #27503, #22186, #16287, #3875, #26180, #691, #11089, #15722, #25939, #4997, #4500, #4194, #25728, #17982, #9586, #15084, #4600, #15893, #21377, #23294, #17030, #10229, #8438, #23885, #11260, #26370, #19633, #22891 ) ) ;
#26784 = LINE ( 'NONE', #12739, #11789 ) ;
#26785 = VECTOR ( 'NONE', #9679, 1000.000000000000000 ) ;
#26786 = DIRECTION ( 'NONE',  ( -0.000000000000000000, -1.000000000000000000, -0.000000000000000000 ) ) ;
#26787 = VECTOR ( 'NONE', #8940, 1000.000000000000000 ) ;
#26788 = DIRECTION ( 'NONE',  ( 0.000000000000000000, 0.000000000000000000, 1.000000000000000000 ) ) ;
#26789 = CARTESIAN_POINT ( 'NONE',  ( 37.97387049854970797, -9.685240207147352010, 12.59636151973351659 ) ) ;
#26790 = FACE_OUTER_BOUND ( 'NONE', #3509, .T. ) ;
#26791 = ORIENTED_EDGE ( 'NONE', *, *, #4317, .T. ) ;
#26792 = CARTESIAN_POINT ( 'NONE',  ( 37.99999999999999289, 80.00000000000000000, 15.49999999999998934 ) ) ;
#26793 = CIRCLE ( 'NONE', #15750, 15.00000000000000000 ) ;
#26794 = LINE ( 'NONE', #14926, #13594 ) ;
#26795 = ORIENTED_EDGE ( 'NONE', *, *, #14165, .T. ) ;
#26796 = ORIENTED_EDGE ( 'NONE', *, *, #18925, .F. ) ;
#26797 = CARTESIAN_POINT ( 'NONE',  ( -3.580889173201297293, 42.33168915099381024, 19.86131920106836546 ) ) ;
#26798 = VECTOR ( 'NONE', #8000, 1000.000000000000114 ) ;
#26799 = EDGE_CURVE ( 'NONE', #12149, #26314, #323, .T. ) ;
#26800 = CARTESIAN_POINT ( 'NONE',  ( -3.897762246399228303, 49.85010185758739709, -40.50684067140829114 ) ) ;
#26801 =( LENGTH_UNIT ( ) NAMED_UNIT ( * ) SI_UNIT ( .MILLI., .METRE. ) );
#26802 = CIRCLE ( 'NONE', #14326, 9.084132297865673777 ) ;
#26803 = ORIENTED_EDGE ( 'NONE', *, *, #332, .T. ) ;
#26804 = ADVANCED_FACE ( 'NONE', ( #9848 ), #7516, .T. ) ;
#26805 = CARTESIAN_POINT ( 'NONE',  ( 15.53792925084563059, 12.62098510012954655, 19.56050940960062690 ) ) ;
#26806 = CARTESIAN_POINT ( 'NONE',  ( -10.58794734610131627, -16.98849370068515086, 5.653912893140659257 ) ) ;
#26807 = ORIENTED_EDGE ( 'NONE', *, *, #6108, .T. ) ;
#26808 = CARTESIAN_POINT ( 'NONE',  ( -16.95074943597165529, 1.765291926024247671, 7.652108011868850035 ) ) ;
#26809 = DIRECTION ( 'NONE',  ( 0.000000000000000000, 0.000000000000000000, -1.000000000000000000 ) ) ;
#26810 = AXIS2_PLACEMENT_3D ( 'NONE', #20190, #5699, #3208 ) ;
#26811 = FACE_OUTER_BOUND ( 'NONE', #6016, .T. ) ;
#26812 = ORIENTED_EDGE ( 'NONE', *, *, #27112, .T. ) ;
#26813 = VECTOR ( 'NONE', #25314, 1000.000000000000000 ) ;
#26814 = CARTESIAN_POINT ( 'NONE',  ( 23.20389136007291953, -12.24563090271730736, 44.52079389607786197 ) ) ;
#26815 = CARTESIAN_POINT ( 'NONE',  ( 1.236805935716845939, 39.48255573641029770, 27.50000000000001066 ) ) ;
#26816 = ORIENTED_EDGE ( 'NONE', *, *, #9015, .F. ) ;
#26817 = VECTOR ( 'NONE', #2335, 1000.000000000000000 ) ;
#26818 = B_SPLINE_CURVE_WITH_KNOTS ( 'NONE', 3,
 ( #12024, #23867, #19804, #2814, #17314, #619, #7348, #7186, #10137, #16697, #4841, #29165, #12337, #28872, #14357, #16859, #14512, #2511 ),
 .UNSPECIFIED., .F., .F.,
 ( 4, 2, 2, 2, 2, 2, 2, 2, 4 ),
 ( 0.000000000000000000, 0.0003967869494442872883, 0.0007935738988885745766, 0.001190360848332861973, 0.001587147797777149153, 0.001983934747221436333, 0.002380721696665723947, 0.002777508646110011126, 0.003174295595554298306 ),
 .UNSPECIFIED. ) ;
#26819 = CARTESIAN_POINT ( 'NONE',  ( -3.696774448978239480, -32.23395975793253854, 28.87158698979378002 ) ) ;
#26820 = CARTESIAN_POINT ( 'NONE',  ( -6.509484584620661707, 15.78915919539661594, 19.25672174529527325 ) ) ;
#26821 = CARTESIAN_POINT ( 'NONE',  ( -13.23068377149358987, 10.73719040084102794, 20.32842677360128292 ) ) ;
#26822 = CIRCLE ( 'NONE', #18365, 32.50000000000000000 ) ;
#26823 = VECTOR ( 'NONE', #4706, 1000.000000000000000 ) ;
#26824 = FACE_OUTER_BOUND ( 'NONE', #15892, .T. ) ;
#26825 = CARTESIAN_POINT ( 'NONE',  ( -38.37115330322435369, -7.710785714854020867, 32.03772168544337262 ) ) ;
#26826 = LINE ( 'NONE', #14793, #3554 ) ;
#26827 = CYLINDRICAL_SURFACE ( 'NONE', #916, 20.00000000000000355 ) ;
#26828 = EDGE_LOOP ( 'NONE', ( #21320, #4050, #7513, #2696 ) ) ;
#26829 = CARTESIAN_POINT ( 'NONE',  ( 10.58525311124732227, -16.99040216561238381, 5.862424720655265098 ) ) ;
#26830 = CARTESIAN_POINT ( 'NONE',  ( -30.56823942190705523, 26.39394548910274452, 8.622060075595381790 ) ) ;
#26831 = CARTESIAN_POINT ( 'NONE',  ( 6.364020599487797192, -6.482337650448430466, 13.22130136205108819 ) ) ;
#26832 = ORIENTED_EDGE ( 'NONE', *, *, #24326, .T. ) ;
#26833 = ORIENTED_EDGE ( 'NONE', *, *, #10750, .F. ) ;
#26834 = DIRECTION ( 'NONE',  ( 1.000000000000000000, 0.000000000000000000, 0.000000000000000000 ) ) ;
#26835 = CARTESIAN_POINT ( 'NONE',  ( 10.36341371996392091, -17.10561997787537436, 7.156831654632823003 ) ) ;
#26836 = CARTESIAN_POINT ( 'NONE',  ( 7.827050521741880651, -5.352643706120488787, 1.500000000000001332 ) ) ;
#26837 = CARTESIAN_POINT ( 'NONE',  ( -15.42263072605321916, -7.221902784610292336, 5.848946451764563292 ) ) ;
#26838 = EDGE_CURVE ( 'NONE', #14649, #4182, #20126, .T. ) ;
#26839 = CARTESIAN_POINT ( 'NONE',  ( -6.543385983536389894, -6.301234758012572712, -1.500000000000002442 ) ) ;
#26840 = EDGE_CURVE ( 'NONE', #13097, #18592, #30577, .T. ) ;
#26841 = DIRECTION ( 'NONE',  ( 0.000000000000000000, 0.000000000000000000, -1.000000000000000000 ) ) ;
#26842 = AXIS2_PLACEMENT_3D ( 'NONE', #12087, #21899, #21586 ) ;
#26843 = CARTESIAN_POINT ( 'NONE',  ( -31.12530087898743503, -19.95159923194576379, 34.50000000000000000 ) ) ;
#26844 = CIRCLE ( 'NONE', #17873, 0.7499999999999997780 ) ;
#26845 = DIRECTION ( 'NONE',  ( 0.000000000000000000, -1.000000000000000000, 0.000000000000000000 ) ) ;
#26846 = AXIS2_PLACEMENT_3D ( 'NONE', #15149, #19996, #10793 ) ;
#26847 = CARTESIAN_POINT ( 'NONE',  ( 19.87340826026480656, 2.401441585233818010, 7.272049892295485485 ) ) ;
#26848 = VERTEX_POINT ( 'NONE', #10150 ) ;
#26849 = CARTESIAN_POINT ( 'NONE',  ( 12.58124959699792988, 11.48680237977196406, 7.595116371587256054 ) ) ;
#26850 = EDGE_LOOP ( 'NONE', ( #26471, #17446, #13388, #11580, #13907 ) ) ;
#26851 = CARTESIAN_POINT ( 'NONE',  ( 16.19545619402288494, -5.420160174983561951, 6.560937769032974209 ) ) ;
#26852 = CARTESIAN_POINT ( 'NONE',  ( 1.073881485057738949, -0.9711784013061123266, 1.500000000000000000 ) ) ;
#26853 = VECTOR ( 'NONE', #25675, 1000.000000000000000 ) ;
#26854 = PLANE ( 'NONE',  #15520 ) ;
#26855 = VERTEX_POINT ( 'NONE', #19654 ) ;
#26856 = CARTESIAN_POINT ( 'NONE',  ( 49.01082926198596823, 69.97703016100948048, 56.88457827394385191 ) ) ;
#26857 = DIRECTION ( 'NONE',  ( 0.5406408174555976665, -0.8412535328311810945, -0.000000000000000000 ) ) ;
#26858 = FACE_OUTER_BOUND ( 'NONE', #18052, .T. ) ;
#26859 = VECTOR ( 'NONE', #25019, 1000.000000000000000 ) ;
#26860 = CARTESIAN_POINT ( 'NONE',  ( -9.406652940105976413, 1.195154792889490114, 1.500000000000001332 ) ) ;
#26861 = CARTESIAN_POINT ( 'NONE',  ( -4.677126025380957230, 39.24912351428227453, 27.50000000000000355 ) ) ;
#26862 = LINE ( 'NONE', #1110, #8849 ) ;
#26863 = CARTESIAN_POINT ( 'NONE',  ( -8.840471615930058036, 1.687027447297517080, 1.500000000000001332 ) ) ;
#26864 = ORIENTED_EDGE ( 'NONE', *, *, #25207, .T. ) ;
#26865 = DIRECTION ( 'NONE',  ( 1.000000000000000000, 0.000000000000000000, 0.000000000000000000 ) ) ;
#26866 = CIRCLE ( 'NONE', #27868, 9.084132297865673777 ) ;
#26867 = CARTESIAN_POINT ( 'NONE',  ( -13.99683207193583812, 9.784088562599670524, 19.58863275299554019 ) ) ;
#26868 = CARTESIAN_POINT ( 'NONE',  ( -7.856594496258223259, -4.390207617113929039, 1.500000000000001332 ) ) ;
#26869 = ORIENTED_EDGE ( 'NONE', *, *, #293, .T. ) ;
#26870 = CARTESIAN_POINT ( 'NONE',  ( 30.55067843133129912, -26.41807869720452473, 17.36820027845536174 ) ) ;
#26871 = CARTESIAN_POINT ( 'NONE',  ( -7.075845757273814415E-16, 65.00000000000000000, 15.49999999999998757 ) ) ;
#26872 = DIRECTION ( 'NONE',  ( -0.000000000000000000, -0.000000000000000000, -1.000000000000000000 ) ) ;
#26873 = CARTESIAN_POINT ( 'NONE',  ( 23.96732207938043402, -33.98584080152387088, -1.500000000000000000 ) ) ;
#26874 = CIRCLE ( 'NONE', #27877, 12.50000000000000000 ) ;
#26875 = PLANE ( 'NONE',  #15380 ) ;
#26876 = CARTESIAN_POINT ( 'NONE',  ( 15.64865523245225631, 38.95674053321715746, 29.15699439579599783 ) ) ;
#26877 = EDGE_CURVE ( 'NONE', #29287, #194, #29178, .T. ) ;
#26878 = CYLINDRICAL_SURFACE ( 'NONE', #15513, 20.00000000000000000 ) ;
#26879 = ORIENTED_EDGE ( 'NONE', *, *, #18423, .T. ) ;
#26880 = CIRCLE ( 'NONE', #5454, 0.7500000000000006661 ) ;
#26881 = CARTESIAN_POINT ( 'NONE',  ( 0.000000000000000000, 0.000000000000000000, 196.3477631085023631 ) ) ;
#26882 = ORIENTED_EDGE ( 'NONE', *, *, #18352, .T. ) ;
#26883 = CARTESIAN_POINT ( 'NONE',  ( -23.26222494989736234, -12.36939612486375495, 44.41134540914034545 ) ) ;
#26884 = ORIENTED_EDGE ( 'NONE', *, *, #3465, .F. ) ;
#26885 = EDGE_LOOP ( 'NONE', ( #15448, #967, #1328, #24818 ) ) ;
#26886 = CARTESIAN_POINT ( 'NONE',  ( -37.99999999999999289, 90.00000000000001421, -22.50000000000001421 ) ) ;
#26887 = ORIENTED_EDGE ( 'NONE', *, *, #16781, .F. ) ;
#26888 = PRODUCT ( 'Vane Snap Cap', 'Vane Snap Cap', '', ( #3047 ) ) ;
#26889 = EDGE_LOOP ( 'NONE', ( #2479, #10142, #26249, #25424 ) ) ;
#26890 = CYLINDRICAL_SURFACE ( 'NONE', #18373, 1.447898107987198646 ) ;
#26891 = CARTESIAN_POINT ( 'NONE',  ( -20.72875052343767521, 32.30954557037109964, 34.49999999999999289 ) ) ;
#26892 = FACE_OUTER_BOUND ( 'NONE', #28778, .T. ) ;
#26893 = CARTESIAN_POINT ( 'NONE',  ( 0.000000000000000000, 0.000000000000000000, 1.500000000000001332 ) ) ;
#26894 = MECHANICAL_DESIGN_GEOMETRIC_PRESENTATION_REPRESENTATION (  '', ( #27897 ), #21391 ) ;
#26895 = CARTESIAN_POINT ( 'NONE',  ( -22.85987860430571317, 23.19171692911513105, -16.50001200000000523 ) ) ;
#26896 = ORIENTED_EDGE ( 'NONE', *, *, #7675, .F. ) ;
#26897 = DIRECTION ( 'NONE',  ( 0.000000000000000000, 1.000000000000000000, 1.193512090021232842E-16 ) ) ;
#26898 = DIRECTION ( 'NONE',  ( 0.000000000000000000, 0.000000000000000000, 1.000000000000000000 ) ) ;
#26899 = DIRECTION ( 'NONE',  ( 0.000000000000000000, 1.000000000000000000, 0.000000000000000000 ) ) ;
#26900 = ORIENTED_EDGE ( 'NONE', *, *, #11130, .T. ) ;
#26901 = EDGE_CURVE ( 'NONE', #30435, #10893, #3703, .T. ) ;
#26902 = CARTESIAN_POINT ( 'NONE',  ( -11.19942626343432046, -16.59192963269641652, 19.96783386855779341 ) ) ;
#26903 = DIRECTION ( 'NONE',  ( 0.000000000000000000, 0.000000000000000000, -1.000000000000000000 ) ) ;
#26904 = CARTESIAN_POINT ( 'NONE',  ( -1.000000000000008438, 19.97498435543819539, 1.500000000000001332 ) ) ;
#26905 = CARTESIAN_POINT ( 'NONE',  ( 10.69045173577874053, -13.31838649416133791, 6.782048567692550378 ) ) ;
#26906 = EDGE_CURVE ( 'NONE', #10785, #26575, #10619, .T. ) ;
#26907 = ADVANCED_FACE ( 'NONE', ( #11081 ), #6553, .F. ) ;
#26908 = CARTESIAN_POINT ( 'NONE',  ( 49.99999999999998579, -50.00000000000000000, 62.49999999999999289 ) ) ;
#26909 = ORIENTED_EDGE ( 'NONE', *, *, #22349, .T. ) ;
#26910 = ORIENTED_EDGE ( 'NONE', *, *, #807, .F. ) ;
#26911 = PRESENTATION_STYLE_ASSIGNMENT (( #7728 ) ) ;
#26912 = EDGE_CURVE ( 'NONE', #30725, #22552, #30253, .T. ) ;
#26913 = CARTESIAN_POINT ( 'NONE',  ( -5.026174198947129135, 19.35820631361447397, 19.60917204426170102 ) ) ;
#26914 = CARTESIAN_POINT ( 'NONE',  ( -3.112355512349863851, -37.38886688928499069, 37.50000000001043787 ) ) ;
#26915 = EDGE_CURVE ( 'NONE', #2444, #25279, #4059, .T. ) ;
#26916 = DIRECTION ( 'NONE',  ( -0.9594929736144974797, -0.2817325568414297265, 0.000000000000000000 ) ) ;
#26917 = ORIENTED_EDGE ( 'NONE', *, *, #4642, .F. ) ;
#26918 = PRODUCT_CONTEXT ( 'NONE', #5195, 'mechanical' ) ;
#26919 = AXIS2_PLACEMENT_3D ( 'NONE', #28555, #12025, #21518 ) ;
#26920 = CARTESIAN_POINT ( 'NONE',  ( 15.78348099220816536, -6.430800111306882449, 18.34969686940296185 ) ) ;
#26921 = CARTESIAN_POINT ( 'NONE',  ( 6.900000000000000355, 7.794228634059944483, -4.500000000000004441 ) ) ;
#26922 = EDGE_CURVE ( 'NONE', #1974, #27180, #17956, .T. ) ;
#26923 = ORIENTED_EDGE ( 'NONE', *, *, #19570, .T. ) ;
#26924 = LINE ( 'NONE', #24558, #3326 ) ;
#26925 = PLANE ( 'NONE',  #10246 ) ;
#26926 = EDGE_CURVE ( 'NONE', #23449, #27382, #1265, .T. ) ;
#26927 = DIRECTION ( 'NONE',  ( 1.000000000000000000, 0.000000000000000000, 0.000000000000000000 ) ) ;
#26928 = CARTESIAN_POINT ( 'NONE',  ( -37.08962926481365940, -5.682944862436646538, 37.49999999998664890 ) ) ;
#26929 = ORIENTED_EDGE ( 'NONE', *, *, #15446, .T. ) ;
#26930 = CARTESIAN_POINT ( 'NONE',  ( 11.77028954461706789, -16.17000817291663495, 7.272192800924339728 ) ) ;
#26931 = EDGE_CURVE ( 'NONE', #28210, #1255, #14071, .T. ) ;
#26932 = CARTESIAN_POINT ( 'NONE',  ( 27.03074382657074537, -6.449748410230991880, -16.55003854064094426 ) ) ;
#26933 = CARTESIAN_POINT ( 'NONE',  ( -19.75697076387333340, 3.109827004491391378, 20.14992337338002315 ) ) ;
#26934 = ORIENTED_EDGE ( 'NONE', *, *, #1930, .F. ) ;
#26935 = APPLICATION_CONTEXT ( 'automotive_design' ) ;
#26936 = CARTESIAN_POINT ( 'NONE',  ( -33.78553954455730235, -24.40792764007751359, -16.50000000000000000 ) ) ;
#26937 = CARTESIAN_POINT ( 'NONE',  ( 32.06725342158288328, 14.54034564589948708, 35.54788606881758994 ) ) ;
#26938 = CARTESIAN_POINT ( 'NONE',  ( 16.18315216712290550, -5.452792103153281111, 6.392658652357117610 ) ) ;
#26939 = CARTESIAN_POINT ( 'NONE',  ( -49.93150111878230035, 70.00033327193624189, 21.15304995801174215 ) ) ;
#26940 = AXIS2_PLACEMENT_3D ( 'NONE', #24450, #6653, #15869 ) ;
#26941 = DIRECTION ( 'NONE',  ( -0.000000000000000000, 1.132880637372608986E-16, -1.000000000000000000 ) ) ;
#26942 = CARTESIAN_POINT ( 'NONE',  ( -50.00000000000000000, 50.00000000000000000, -87.50000000000000000 ) ) ;
#26943 = CARTESIAN_POINT ( 'NONE',  ( 37.97804311825484547, -9.665537939806041479, 13.32538434702631669 ) ) ;
#26944 = CARTESIAN_POINT ( 'NONE',  ( 0.000000000000000000, 42.50000000000000000, 27.50000000000000355 ) ) ;
#26945 = ORIENTED_EDGE ( 'NONE', *, *, #10750, .T. ) ;
#26946 = EDGE_CURVE ( 'NONE', #22873, #20218, #10824, .T. ) ;
#26947 = EDGE_CURVE ( 'NONE', #29162, #23828, #25538, .T. ) ;
#26948 = DIRECTION ( 'NONE',  ( 0.000000000000000000, 1.000000000000000000, -0.000000000000000000 ) ) ;
#26949 = CARTESIAN_POINT ( 'NONE',  ( 3.637110358602580362, -19.99473753024311762, 1.500000000000000000 ) ) ;
#26950 = VERTEX_POINT ( 'NONE', #15442 ) ;
#26951 = ADVANCED_FACE ( 'NONE', ( #27619 ), #20052, .T. ) ;
#26952 = VERTEX_POINT ( 'NONE', #24963 ) ;
#26953 = DIRECTION ( 'NONE',  ( 1.000000000000000000, 0.000000000000000000, 0.000000000000000000 ) ) ;
#26954 = CARTESIAN_POINT ( 'NONE',  ( -10.26695923285440060, 48.93580713664579207, -44.05349679880919922 ) ) ;
#26955 = EDGE_CURVE ( 'NONE', #27927, #24825, #10773, .T. ) ;
#26956 = ORIENTED_EDGE ( 'NONE', *, *, #14923, .F. ) ;
#26957 = CARTESIAN_POINT ( 'NONE',  ( -35.93563768862540542, 2.440659245201815430, 27.50000000000000355 ) ) ;
#26958 = CARTESIAN_POINT ( 'NONE',  ( 0.000000000000000000, 7.028748154183637631, -16.50000000000000000 ) ) ;
#26959 = EDGE_CURVE ( 'NONE', #3771, #23438, #26612, .T. ) ;
#26960 = EDGE_LOOP ( 'NONE', ( #14307, #16584, #28136, #2708, #27132, #12138 ) ) ;
#26961 = CARTESIAN_POINT ( 'NONE',  ( 15.84193441942127833, -6.296838616230740371, 20.34789198813115263 ) ) ;
#26962 = AXIS2_PLACEMENT_3D ( 'NONE', #10349, #19860, #10501 ) ;
#26963 = CARTESIAN_POINT ( 'NONE',  ( -27.03074382657074182, -6.449748410230987439, 47.21042702067970964 ) ) ;
#26964 = AXIS2_PLACEMENT_3D ( 'NONE', #27405, #29580, #13055 ) ;
#26965 = B_SPLINE_CURVE_WITH_KNOTS ( 'NONE', 3,
 ( #15287, #22464, #29349, #9854, #19368, #17020, #17173, #26693 ),
 .UNSPECIFIED., .F., .F.,
 ( 4, 2, 2, 4 ),
 ( 0.005257893453559900170, 0.006567392922673233845, 0.007876892391786568387, 0.01049589133001323400 ),
 .UNSPECIFIED. ) ;
#26966 = CARTESIAN_POINT ( 'NONE',  ( 0.000000000000000000, 0.000000000000000000, 1.500000000000001332 ) ) ;
#26967 = ORIENTED_EDGE ( 'NONE', *, *, #25431, .T. ) ;
#26968 = DIRECTION ( 'NONE',  ( 0.4154150130018864906, -0.9096319953545183301, 0.000000000000000000 ) ) ;
#26969 = CARTESIAN_POINT ( 'NONE',  ( 43.34097750826426676, -11.89502811014149941, 1.500000000000000000 ) ) ;
#26970 = ORIENTED_EDGE ( 'NONE', *, *, #22710, .F. ) ;
#26971 = CARTESIAN_POINT ( 'NONE',  ( -7.322557715923444732, 14.41080185948837311, 24.50000000000000000 ) ) ;
#26972 = EDGE_CURVE ( 'NONE', #14561, #27449, #25040, .T. ) ;
#26973 = CARTESIAN_POINT ( 'NONE',  ( 38.94223652925970924, 2.647167246129292550, 32.21377772506992443 ) ) ;
#26974 = CARTESIAN_POINT ( 'NONE',  ( 16.56580381663018642, 4.144794415032111878, 6.341840715582230281 ) ) ;
#26975 = CARTESIAN_POINT ( 'NONE',  ( -50.00000000000000000, -70.00000000000000000, 12.49999999999999112 ) ) ;
#26976 = EDGE_CURVE ( 'NONE', #8129, #9428, #9169, .T. ) ;
#26977 = CARTESIAN_POINT ( 'NONE',  ( -10.39297074171570401, -17.10854403003572699, 18.35718225375110180 ) ) ;
#26978 = CARTESIAN_POINT ( 'NONE',  ( -16.13886355804662998, 38.71476141167133278, 29.17969182664677419 ) ) ;
#26979 = DIRECTION ( 'NONE',  ( -1.000000000000000000, 0.000000000000000000, 0.000000000000000000 ) ) ;
#26980 = DIRECTION ( 'NONE',  ( -0.000000000000000000, -0.000000000000000000, -1.000000000000000000 ) ) ;
#26981 = ORIENTED_EDGE ( 'NONE', *, *, #16839, .F. ) ;
#26982 = CARTESIAN_POINT ( 'NONE',  ( 9.411519254647288335, -14.19511874370441262, 5.796888747622817029 ) ) ;
#26983 = CARTESIAN_POINT ( 'NONE',  ( 34.70577939417261604, -10.49309206032036634, 34.49999999999999289 ) ) ;
#26984 = AXIS2_PLACEMENT_3D ( 'NONE', #12999, #30290, #20158 ) ;
#26985 = CARTESIAN_POINT ( 'NONE',  ( 6.812559277181973627, -5.881244434206257310, 1.500000000000001332 ) ) ;
#26986 = CARTESIAN_POINT ( 'NONE',  ( 33.16313691975489064, -7.028748154183637631, -1.500000000000000000 ) ) ;
#26987 = ORIENTED_EDGE ( 'NONE', *, *, #18101, .T. ) ;
#26988 = VERTEX_POINT ( 'NONE', #22926 ) ;
#26989 = CARTESIAN_POINT ( 'NONE',  ( 18.33793066653144876, -7.982499537706464920, 18.34798005863226678 ) ) ;
#26990 = DIRECTION ( 'NONE',  ( 0.000000000000000000, 1.000000000000000000, 0.000000000000000000 ) ) ;
#26991 = FACE_OUTER_BOUND ( 'NONE', #3611, .T. ) ;
#26992 = ORIENTED_EDGE ( 'NONE', *, *, #617, .F. ) ;
#26993 = DIRECTION ( 'NONE',  ( 0.000000000000000000, 1.000000000000000000, 0.000000000000000000 ) ) ;
#26994 = DIRECTION ( 'NONE',  ( -0.000000000000000000, -0.000000000000000000, -1.000000000000000000 ) ) ;
#26995 = CARTESIAN_POINT ( 'NONE',  ( -13.38160118231794549, 10.55829203257430038, 5.652196082368482699 ) ) ;
#26996 = ORIENTED_EDGE ( 'NONE', *, *, #20679, .F. ) ;
#26997 = VECTOR ( 'NONE', #21467, 1000.000000000000000 ) ;
#26998 = CARTESIAN_POINT ( 'NONE',  ( 3.668292057956000551, -8.743977807160085547, 13.00000000000000178 ) ) ;
#26999 = CARTESIAN_POINT ( 'NONE',  ( 14.52517991353746751, 13.77415465259964478, 5.810767894563978686 ) ) ;
#27000 = CARTESIAN_POINT ( 'NONE',  ( 16.87696675355430642, 2.215034284604906922, 6.420335371522007506 ) ) ;
#27001 = ORIENTED_EDGE ( 'NONE', *, *, #9609, .T. ) ;
#27002 = CARTESIAN_POINT ( 'NONE',  ( 26.36764545593179676, 31.31467416275351923, 1.500000000000000000 ) ) ;
#27003 = VERTEX_POINT ( 'NONE', #27774 ) ;
#27004 = CARTESIAN_POINT ( 'NONE',  ( 10.18506332983503349, -29.04537757311073420, 1.500000000000001332 ) ) ;
#27005 = PRODUCT_DEFINITION_CONTEXT ( 'detailed design', #14576, 'design' ) ;
#27006 = DIRECTION ( 'NONE',  ( -0.000000000000000000, -0.000000000000000000, 1.000000000000000000 ) ) ;
#27007 = CARTESIAN_POINT ( 'NONE',  ( -25.41307773079512344, 6.523700759042258213, 44.52046879171667371 ) ) ;
#27008 = ORIENTED_EDGE ( 'NONE', *, *, #9706, .F. ) ;
#27009 = DIRECTION ( 'NONE',  ( -1.000000000000000000, 0.000000000000000000, 0.000000000000000000 ) ) ;
#27010 = PLANE ( 'NONE',  #16069 ) ;
#27011 = DIRECTION ( 'NONE',  ( 0.000000000000000000, 0.000000000000000000, 1.000000000000000000 ) ) ;
#27012 = CARTESIAN_POINT ( 'NONE',  ( 23.79391290694626093, 29.65739006622967011, 34.50000000000000711 ) ) ;
#27013 = CARTESIAN_POINT ( 'NONE',  ( -23.69412710310941961, 29.84645176427129698, 34.80090346875805096 ) ) ;
#27014 = DIRECTION ( 'NONE',  ( -0.000000000000000000, -0.000000000000000000, 1.000000000000000000 ) ) ;
#27015 = VERTEX_POINT ( 'NONE', #19164 ) ;
#27016 = CIRCLE ( 'NONE', #13573, 1.000000000000009548 ) ;
#27017 = DIRECTION ( 'NONE',  ( 0.000000000000000000, 1.000000000000000000, 0.000000000000000000 ) ) ;
#27018 = CARTESIAN_POINT ( 'NONE',  ( -14.01239083805805485, 9.763392886517387126, 19.25672174529527325 ) ) ;
#27019 = CARTESIAN_POINT ( 'NONE',  ( 23.21352257770656635, -10.78826658734920052, 49.40206402021031806 ) ) ;
#27020 = EDGE_LOOP ( 'NONE', ( #4177, #4805, #14499, #15152, #13068, #29446 ) ) ;
#27021 = CARTESIAN_POINT ( 'NONE',  ( 28.46402972798047060, -29.05374092982643575, 15.13942714145325041 ) ) ;
#27022 = DIRECTION ( 'NONE',  ( 1.000000000000000000, 0.000000000000000000, 0.000000000000000000 ) ) ;
#27023 = CARTESIAN_POINT ( 'NONE',  ( -44.99999999999955236, -4.926614671774132148E-13, 77.49999999999998579 ) ) ;
#27024 = AXIS2_PLACEMENT_3D ( 'NONE', #7858, #672, #15015 ) ;
#27025 = CARTESIAN_POINT ( 'NONE',  ( 34.07766914598172292, -21.40380666527112652, -1.500000000000000000 ) ) ;
#27026 = CARTESIAN_POINT ( 'NONE',  ( 0.000000000000000000, 0.000000000000000000, 57.49999999999999289 ) ) ;
#27027 = CARTESIAN_POINT ( 'NONE',  ( 17.48232412878148878, 37.99796894973091099, 29.24739480102024558 ) ) ;
#27028 = CARTESIAN_POINT ( 'NONE',  ( 19.55539447853113799, 4.193631725790827325, 6.788986777570706010 ) ) ;
#27029 = VERTEX_POINT ( 'NONE', #28071 ) ;
#27030 = CARTESIAN_POINT ( 'NONE',  ( -33.56595177138117947, -10.45696648424866204, 35.60059606545802779 ) ) ;
#27031 = ORIENTED_EDGE ( 'NONE', *, *, #10906, .F. ) ;
#27032 = LINE ( 'NONE', #5659, #22645 ) ;
#27033 = DIRECTION ( 'NONE',  ( 0.000000000000000000, 0.000000000000000000, 1.000000000000000000 ) ) ;
#27034 = VERTEX_POINT ( 'NONE', #134 ) ;
#27035 = CIRCLE ( 'NONE', #20541, 9.084132297865673777 ) ;
#27036 = ORIENTED_EDGE ( 'NONE', *, *, #4607, .T. ) ;
#27037 = DIRECTION ( 'NONE',  ( -0.000000000000000000, -0.000000000000000000, -1.000000000000000000 ) ) ;
#27038 = VECTOR ( 'NONE', #28007, 1000.000000000000114 ) ;
#27039 = ORIENTED_EDGE ( 'NONE', *, *, #14502, .F. ) ;
#27040 = CARTESIAN_POINT ( 'NONE',  ( 17.26937953831880534, -14.36006998371588317, -1.500000000000000000 ) ) ;
#27041 = DIRECTION ( 'NONE',  ( -1.000000000000000000, 0.000000000000000000, 0.000000000000000000 ) ) ;
#27042 = DIRECTION ( 'NONE',  ( 0.000000000000000000, -1.132880637372608986E-16, 1.000000000000000000 ) ) ;
#27043 = CARTESIAN_POINT ( 'NONE',  ( -37.47155912781716580, 11.78490175834441267, 10.78014334239690797 ) ) ;
#27044 = CARTESIAN_POINT ( 'NONE',  ( -24.27860874716794726, 23.00333360197816290, -16.50001200000000168 ) ) ;
#27045 = EDGE_CURVE ( 'NONE', #7648, #7334, #11591, .T. ) ;
#27046 = CARTESIAN_POINT ( 'NONE',  ( 5.738360882149947884, 7.548823014270664267, 13.00000000000000178 ) ) ;
#27047 = CARTESIAN_POINT ( 'NONE',  ( 8.884323311075775109, 1.438332125858202692, 21.50000000000000000 ) ) ;
#27048 = CARTESIAN_POINT ( 'NONE',  ( 24.03057240117691862, 26.57182937991349903, 26.54355021145563143 ) ) ;
#27049 = EDGE_LOOP ( 'NONE', ( #19629, #3463 ) ) ;
#27050 = CARTESIAN_POINT ( 'NONE',  ( -9.376411575904489482, -14.20642299464376990, 19.56050940960062690 ) ) ;
#27051 = CARTESIAN_POINT ( 'NONE',  ( -17.91516185886247925, -8.931344358737685951, 7.603368798681074736 ) ) ;
#27052 = CARTESIAN_POINT ( 'NONE',  ( -6.193882932557621679, 19.03538945389874115, 5.678370764302467677 ) ) ;
#27053 = CIRCLE ( 'NONE', #20560, 10.00000000000000000 ) ;
#27054 = FACE_OUTER_BOUND ( 'NONE', #4146, .T. ) ;
#27055 = AXIS2_PLACEMENT_3D ( 'NONE', #9740, #6638, #16153 ) ;
#27056 = CARTESIAN_POINT ( 'NONE',  ( 13.22505861668195237, -42.10773672056998862, -19.50000000000000355 ) ) ;
#27057 = CARTESIAN_POINT ( 'NONE',  ( 0.000000000000000000, 0.000000000000000000, 1.500000000000001332 ) ) ;
#27058 = ORIENTED_EDGE ( 'NONE', *, *, #13187, .F. ) ;
#27059 = ORIENTED_EDGE ( 'NONE', *, *, #1210, .T. ) ;
#27060 = CARTESIAN_POINT ( 'NONE',  ( 5.060094141397912360, 42.14075867279367316, 28.87075318537527835 ) ) ;
#27061 = CARTESIAN_POINT ( 'NONE',  ( 13.22505861668094340, 42.10773672057246841, -19.50000000000000355 ) ) ;
#27062 = CARTESIAN_POINT ( 'NONE',  ( 2.598297338551552205, -42.41243084101535032, 28.84727347638572681 ) ) ;
#27063 = DIRECTION ( 'NONE',  ( 0.000000000000000000, -1.000000000000000000, 0.000000000000000000 ) ) ;
#27064 = ORIENTED_EDGE ( 'NONE', *, *, #18066, .F. ) ;
#27065 = CARTESIAN_POINT ( 'NONE',  ( 16.12178322346233728, -5.613588367413085756, 18.73314399819312115 ) ) ;
#27066 = CARTESIAN_POINT ( 'NONE',  ( 5.335947603960573993, 19.29354331951100576, 5.651989602109218858 ) ) ;
#27067 = ORIENTED_EDGE ( 'NONE', *, *, #29235, .F. ) ;
#27068 = DIRECTION ( 'NONE',  ( 0.9594929736144992560, 0.2817325568414232317, 0.000000000000000000 ) ) ;
#27069 = B_SPLINE_SURFACE_WITH_KNOTS ( 'NONE', 1, 3, ( 
 ( #13680, #20526, #15852, #20070, #25205, #8383, #18198, #6033, #17900, #22554, #27414, #27872, #8544, #30047, #13528, #1208, #23010, #15383, #24908, #6496, #18046, #20674, #30197, #13214, #16006, #10560, #29589, #8223, #3544, #27561, #22702, #1357, #13373, #22866, #1516, #2109, #11630, #26281, #25978, #4608, #4296, #14108 ),
 ( #6791, #18969, #2258, #28329, #13825, #21122, #30804, #28477, #23162, #13972, #18510, #4463, #30641, #30354, #30494, #19109, #25674, #1964, #20830, #8995, #11779, #9453, #7105, #9135, #4754, #2428, #16614, #9288, #23776, #85, #28011, #26123, #14257, #23325, #11952, #4916, #6642, #21443, #28628, #21283, #23616, #18812 ) ),
 .UNSPECIFIED., .F., .T., .F.,
 ( 2, 2 ),
 ( 4, 2, 2, 2, 2, 2, 2, 2, 2, 2, 2, 2, 2, 2, 2, 2, 2, 2, 2, 2, 4 ),
 ( 0.000000000000000000, 1.000000000000000000 ),
 ( 0.000000000000000000, 0.1963495408493620697, 0.3926990816987241395, 0.7853981633974482790, 1.178097245096172418, 1.570796326794896558, 1.963495408493620697, 2.356194490192344837, 2.748893571891068976, 2.945243112740430824, 3.141592653589793116, 3.337942194439155408, 3.534291735288517255, 3.926990816987241395, 4.319689898685965090, 4.712388980384689674, 5.105088062083414258, 5.497787143782137953, 5.890486225480861648, 6.086835766330223940, 6.283185307179586232 ),
 .UNSPECIFIED. ) ;
#27070 = CARTESIAN_POINT ( 'NONE',  ( 0.1469846612282592335, -6.696526368584486022, 6.401276095386999820 ) ) ;
#27071 = CARTESIAN_POINT ( 'NONE',  ( -32.99004629359474450, -22.67711567301405395, 30.80987819614264112 ) ) ;
#27072 = ADVANCED_FACE ( 'NONE', ( #30855 ), #11687, .F. ) ;
#27073 = VERTEX_POINT ( 'NONE', #4354 ) ;
#27074 = DIRECTION ( 'NONE',  ( -0.000000000000000000, 0.000000000000000000, 1.000000000000000000 ) ) ;
#27075 = AXIS2_PLACEMENT_3D ( 'NONE', #3773, #13293, #22788 ) ;
#27076 = DIRECTION ( 'NONE',  ( 1.000000000000000000, 0.000000000000000000, 0.000000000000000000 ) ) ;
#27077 = DIRECTION ( 'NONE',  ( 1.000000000000000000, 0.000000000000000000, 0.000000000000000000 ) ) ;
#27078 = EDGE_CURVE ( 'NONE', #5571, #13268, #30411, .T. ) ;
#27079 = ORIENTED_EDGE ( 'NONE', *, *, #23292, .F. ) ;
#27080 = CARTESIAN_POINT ( 'NONE',  ( -15.21221250122201596, -7.682808169219083716, 5.657991946698900598 ) ) ;
#27081 = DIRECTION ( 'NONE',  ( 1.000000000000000000, 0.000000000000000000, 0.000000000000000000 ) ) ;
#27082 = EDGE_CURVE ( 'NONE', #9760, #5348, #23216, .T. ) ;
#27083 = CARTESIAN_POINT ( 'NONE',  ( 37.16608720827707657, 65.00000000000000000, 97.07879600563551037 ) ) ;
#27084 = LINE ( 'NONE', #3217, #28704 ) ;
#27085 = CARTESIAN_POINT ( 'NONE',  ( -37.16608720827707657, 65.00000000000000000, 12.49999999999999112 ) ) ;
#27086 = DIRECTION ( 'NONE',  ( 0.000000000000000000, 0.000000000000000000, 1.000000000000000000 ) ) ;
#27087 = CARTESIAN_POINT ( 'NONE',  ( -2.270234684139619485, 8.795879380940586856, -1.500000000000000666 ) ) ;
#27088 = ORIENTED_EDGE ( 'NONE', *, *, #7646, .F. ) ;
#27089 = DIRECTION ( 'NONE',  ( -0.000000000000000000, -0.000000000000000000, 1.000000000000000000 ) ) ;
#27090 = AXIS2_PLACEMENT_3D ( 'NONE', #9347, #2317, #11844 ) ;
#27091 = DIRECTION ( 'NONE',  ( -0.000000000000000000, -0.000000000000000000, 1.000000000000000000 ) ) ;
#27092 = EDGE_CURVE ( 'NONE', #16156, #26411, #9345, .T. ) ;
#27093 = ORIENTED_EDGE ( 'NONE', *, *, #20469, .F. ) ;
#27094 = ORIENTED_EDGE ( 'NONE', *, *, #11521, .F. ) ;
#27095 = ADVANCED_FACE ( 'NONE', ( #9048, #25883, #11543 ), #6608, .T. ) ;
#27096 = LINE ( 'NONE', #1050, #16937 ) ;
#27097 = CIRCLE ( 'NONE', #2190, 3.000000000000002665 ) ;
#27098 = CARTESIAN_POINT ( 'NONE',  ( 11.40980092660686118, 6.310027164379057751, 1.500000000000001332 ) ) ;
#27099 = LINE ( 'NONE', #1209, #20865 ) ;
#27100 = CIRCLE ( 'NONE', #11085, 0.7499999999999988898 ) ;
#27101 = CARTESIAN_POINT ( 'NONE',  ( -35.73758792595601363, 4.918610258824734238, 27.49999999999999645 ) ) ;
#27102 = CARTESIAN_POINT ( 'NONE',  ( 12.91703683527121171, 11.08965543756653283, 18.80699882434806369 ) ) ;
#27103 = ORIENTED_EDGE ( 'NONE', *, *, #20311, .T. ) ;
#27104 = ORIENTED_EDGE ( 'NONE', *, *, #9932, .F. ) ;
#27105 = CARTESIAN_POINT ( 'NONE',  ( 18.52307105101190032, -7.590397700845933571, 20.25542030744407640 ) ) ;
#27106 = CARTESIAN_POINT ( 'NONE',  ( 17.99898938545032223, -8.720395568141150022, 7.267242832833938238 ) ) ;
#27107 = LINE ( 'NONE', #19765, #24424 ) ;
#27108 = ORIENTED_EDGE ( 'NONE', *, *, #27842, .F. ) ;
#27109 = CARTESIAN_POINT ( 'NONE',  ( -4.390207617113899730, 7.856594496258241023, 1.500000000000001332 ) ) ;
#27110 = ADVANCED_FACE ( 'NONE', ( #4813 ), #23524, .F. ) ;
#27111 = ORIENTED_EDGE ( 'NONE', *, *, #2848, .F. ) ;
#27112 = EDGE_CURVE ( 'NONE', #6853, #26065, #10598, .T. ) ;
#27113 = CARTESIAN_POINT ( 'NONE',  ( 40.05104235265675783, -2.353288714521559744, -11.49999999999999645 ) ) ;
#27114 = EDGE_CURVE ( 'NONE', #22222, #11207, #13879, .T. ) ;
#27115 = ORIENTED_EDGE ( 'NONE', *, *, #14003, .T. ) ;
#27116 = VECTOR ( 'NONE', #21640, 1000.000000000000000 ) ;
#27117 = CYLINDRICAL_SURFACE ( 'NONE', #9239, 20.00000000000000355 ) ;
#27118 = EDGE_CURVE ( 'NONE', #22347, #7027, #9499, .T. ) ;
#27119 = CARTESIAN_POINT ( 'NONE',  ( 13.78074022358099704, -39.76440514451509500, 29.08269373213634168 ) ) ;
#27120 = CARTESIAN_POINT ( 'NONE',  ( 16.66826434373540877, 3.628879393376895024, 7.559636331181775581 ) ) ;
#27121 = CARTESIAN_POINT ( 'NONE',  ( -13.09601454503479445, 10.89247868135537622, 18.44501272782439827 ) ) ;
#27122 = CARTESIAN_POINT ( 'NONE',  ( -40.00000000000000000, 90.00000000000001421, 15.49999999999998934 ) ) ;
#27123 = EDGE_CURVE ( 'NONE', #13970, #7038, #1869, .T. ) ;
#27124 = CARTESIAN_POINT ( 'NONE',  ( -23.10040941844921392, -34.24922087329859721, 29.61388150951794884 ) ) ;
#27125 = DIRECTION ( 'NONE',  ( 0.000000000000000000, 0.000000000000000000, 1.000000000000000000 ) ) ;
#27126 = DIRECTION ( 'NONE',  ( 0.000000000000000000, -0.000000000000000000, -1.000000000000000000 ) ) ;
#27127 = ORIENTED_EDGE ( 'NONE', *, *, #26720, .T. ) ;
#27128 = ADVANCED_FACE ( 'NONE', ( #9654 ), #28213, .F. ) ;
#27129 = CARTESIAN_POINT ( 'NONE',  ( 10.44969336715137587, -17.07413037334559647, 6.018569869498933578 ) ) ;
#27130 = CARTESIAN_POINT ( 'NONE',  ( -29.08334023542832369, 28.31627646104946194, 9.871544281921535102 ) ) ;
#27131 = CYLINDRICAL_SURFACE ( 'NONE', #6118, 0.6002263538043630664 ) ;
#27132 = ORIENTED_EDGE ( 'NONE', *, *, #10503, .T. ) ;
#27133 = ORIENTED_EDGE ( 'NONE', *, *, #26732, .T. ) ;
#27134 = CARTESIAN_POINT ( 'NONE',  ( 33.42925964089140933, 11.06161099612213405, 35.54550565580007060 ) ) ;
#27135 = DIRECTION ( 'NONE',  ( 1.000000000000000000, 0.000000000000000000, 0.000000000000000000 ) ) ;
#27136 = DIRECTION ( 'NONE',  ( -0.000000000000000000, -0.000000000000000000, -1.000000000000000000 ) ) ;
#27137 = ORIENTED_EDGE ( 'NONE', *, *, #8661, .F. ) ;
#27138 = DIRECTION ( 'NONE',  ( 0.000000000000000000, 0.000000000000000000, -1.000000000000000000 ) ) ;
#27139 = DIRECTION ( 'NONE',  ( -0.000000000000000000, -0.000000000000000000, -1.000000000000000000 ) ) ;
#27140 = AXIS2_PLACEMENT_3D ( 'NONE', #15388, #3548, #9141 ) ;
#27141 = CARTESIAN_POINT ( 'NONE',  ( -7.749586724479453181, -2.959227181723774525, -3.621320343559650379 ) ) ;
#27142 = EDGE_CURVE ( 'NONE', #17860, #1741, #28529, .T. ) ;
#27143 = VERTEX_POINT ( 'NONE', #26032 ) ;
#27144 = CARTESIAN_POINT ( 'NONE',  ( -10.07574916981068647, -17.27697906656895199, 18.47531940416305929 ) ) ;
#27145 = DIRECTION ( 'NONE',  ( 0.000000000000000000, -0.000000000000000000, -1.000000000000000000 ) ) ;
#27146 = CARTESIAN_POINT ( 'NONE',  ( 19.84003625978226282, 2.664153601443037367, 5.796888747622817029 ) ) ;
#27147 = ORIENTED_EDGE ( 'NONE', *, *, #17633, .F. ) ;
#27148 = CARTESIAN_POINT ( 'NONE',  ( 14.89413762494257121, 13.37445394317134095, 5.652196082367002106 ) ) ;
#27149 = ADVANCED_FACE ( 'NONE', ( #14167 ), #2172, .F. ) ;
#27150 = ORIENTED_EDGE ( 'NONE', *, *, #20636, .F. ) ;
#27151 = DIRECTION ( 'NONE',  ( -0.000000000000000000, -0.000000000000000000, 1.000000000000000000 ) ) ;
#27152 = EDGE_CURVE ( 'NONE', #19059, #16046, #26182, .T. ) ;
#27153 = AXIS2_PLACEMENT_3D ( 'NONE', #5342, #14853, #14552 ) ;
#27154 = DIRECTION ( 'NONE',  ( 1.000000000000000000, 0.000000000000000000, 0.000000000000000000 ) ) ;
#27155 = EDGE_CURVE ( 'NONE', #19850, #20585, #4664, .T. ) ;
#27156 = ORIENTED_EDGE ( 'NONE', *, *, #19914, .T. ) ;
#27157 = CARTESIAN_POINT ( 'NONE',  ( 4.049916830765392106, 16.55712665160099206, 7.652108011868850035 ) ) ;
#27158 = FACE_OUTER_BOUND ( 'NONE', #5356, .T. ) ;
#27159 = LINE ( 'NONE', #20442, #11354 ) ;
#27160 = CARTESIAN_POINT ( 'NONE',  ( 34.17801210021485758, 12.44599808121550844, 34.49999999999999289 ) ) ;
#27161 = VECTOR ( 'NONE', #5813, 1000.000000000000000 ) ;
#27162 = CARTESIAN_POINT ( 'NONE',  ( 2.431858781452735485, 8.752572334588128555, 13.22130136205108997 ) ) ;
#27163 = CARTESIAN_POINT ( 'NONE',  ( -50.00000000000000000, 70.00000000000000000, 22.49999999999999289 ) ) ;
#27164 = CARTESIAN_POINT ( 'NONE',  ( -4.608906612435655248, -7.730328572437724866, 1.500000000000001332 ) ) ;
#27165 = ORIENTED_EDGE ( 'NONE', *, *, #18176, .T. ) ;
#27166 = CARTESIAN_POINT ( 'NONE',  ( -40.00000000000002842, 80.00000000000001421, 52.50000000000014921 ) ) ;
#27167 = CARTESIAN_POINT ( 'NONE',  ( -13.72472375636738562, 10.13620556525982508, 18.50655187082627862 ) ) ;
#27168 = CARTESIAN_POINT ( 'NONE',  ( 0.000000000000000000, 0.000000000000000000, 1.500000000000001332 ) ) ;
#27169 = CARTESIAN_POINT ( 'NONE',  ( -23.07950435457351190, 11.50806656539842798, 44.96784366550151191 ) ) ;
#27170 = ORIENTED_EDGE ( 'NONE', *, *, #15915, .T. ) ;
#27171 = CARTESIAN_POINT ( 'NONE',  ( 28.22957482844025989, -29.32399075545982470, 14.55061583020274441 ) ) ;
#27172 = DIRECTION ( 'NONE',  ( 0.000000000000000000, 0.000000000000000000, -1.000000000000000000 ) ) ;
#27173 = CARTESIAN_POINT ( 'NONE',  ( 12.35846533491531041, 11.73919094685904696, 7.652108011868850923 ) ) ;
#27174 = DIRECTION ( 'NONE',  ( -0.000000000000000000, -0.000000000000000000, -1.000000000000000000 ) ) ;
#27175 = DIRECTION ( 'NONE',  ( -0.8412535328311884220, -0.5406408174555862312, 0.000000000000000000 ) ) ;
#27176 = FACE_BOUND ( 'NONE', #2192, .T. ) ;
#27177 = CARTESIAN_POINT ( 'NONE',  ( 16.83292851407377455, 2.581421006753988223, 7.453286057244488561 ) ) ;
#27178 = EDGE_CURVE ( 'NONE', #4181, #27891, #27053, .T. ) ;
#27179 = B_SPLINE_CURVE_WITH_KNOTS ( 'NONE', 3,
 ( #29159, #16850, #2973, #7495, #14807, #21510, #19342, #29007, #10130, #28864, #612, #10282, #16692, #19181, #16993, #26837, #26668, #26516, #4993, #12489 ),
 .UNSPECIFIED., .F., .F.,
 ( 4, 2, 2, 2, 2, 2, 2, 2, 2, 4 ),
 ( 0.000000000000000000, 0.06250000000000045797, 0.1250000000000009159, 0.1875000000000013878, 0.2187500000000014155, 0.2500000000000014433, 0.3125000000000010547, 0.3750000000000007216, 0.4375000000000003331, 0.4999999999999999445 ),
 .UNSPECIFIED. ) ;
#27180 = VERTEX_POINT ( 'NONE', #5126 ) ;
#27181 = EDGE_CURVE ( 'NONE', #4505, #28974, #24140, .T. ) ;
#27182 = CYLINDRICAL_SURFACE ( 'NONE', #27869, 1.447898107987198646 ) ;
#27183 = CARTESIAN_POINT ( 'NONE',  ( 2.352830851074115159, 9.185733585337917617, 13.00000000000000178 ) ) ;
#27184 = DIRECTION ( 'NONE',  ( 1.000000000000000000, 0.000000000000000000, 0.000000000000000000 ) ) ;
#27185 = ORIENTED_EDGE ( 'NONE', *, *, #21704, .F. ) ;
#27186 = AXIS2_PLACEMENT_3D ( 'NONE', #14842, #12677, #10319 ) ;
#27187 = EDGE_LOOP ( 'NONE', ( #4089, #22185 ) ) ;
#27188 = DIRECTION ( 'NONE',  ( 0.000000000000000000, 0.000000000000000000, 1.000000000000000000 ) ) ;
#27189 = ORIENTED_EDGE ( 'NONE', *, *, #10099, .T. ) ;
#27190 = DIRECTION ( 'NONE',  ( 1.000000000000000000, 0.000000000000000000, 0.000000000000000000 ) ) ;
#27191 = LINE ( 'NONE', #3487, #24741 ) ;
#27192 = DIRECTION ( 'NONE',  ( 1.000000000000000000, 0.000000000000000000, 0.000000000000000000 ) ) ;
#27193 = CARTESIAN_POINT ( 'NONE',  ( 9.062880100047298271, 0.6210184355499750453, 21.50000000000000000 ) ) ;
#27194 = CARTESIAN_POINT ( 'NONE',  ( -27.03074382657074537, 6.449748410230984774, 42.96778633356043287 ) ) ;
#27195 = CARTESIAN_POINT ( 'NONE',  ( -11.19315777850256488, -16.57474394094692016, 7.267242832833947119 ) ) ;
#27196 = DIRECTION ( 'NONE',  ( 0.3598999890241647570, -0.9329908884337542174, 0.000000000000000000 ) ) ;
#27197 = CARTESIAN_POINT ( 'NONE',  ( -32.19782014694307293, -14.25394737442115733, -16.55003854064094426 ) ) ;
#27198 = DIRECTION ( 'NONE',  ( -1.000000000000000000, 0.000000000000000000, 0.000000000000000000 ) ) ;
#27199 = ORIENTED_EDGE ( 'NONE', *, *, #12678, .F. ) ;
#27200 = CARTESIAN_POINT ( 'NONE',  ( -14.88329716083761411, -8.348731837201613715, 7.441806358946449151 ) ) ;
#27201 = LINE ( 'NONE', #5837, #22518 ) ;
#27202 = CIRCLE ( 'NONE', #13274, 6.000000000000005329 ) ;
#27203 = CARTESIAN_POINT ( 'NONE',  ( 10.05214800432092837, -13.77402237313447131, 5.678370764302467677 ) ) ;
#27204 = CARTESIAN_POINT ( 'NONE',  ( 40.89187623478217404, 5.790488632116406187, -19.50000000000000355 ) ) ;
#27205 = DIRECTION ( 'NONE',  ( 1.000000000000000000, 0.000000000000000000, 0.000000000000000000 ) ) ;
#27206 = ORIENTED_EDGE ( 'NONE', *, *, #30147, .T. ) ;
#27207 = ORIENTED_EDGE ( 'NONE', *, *, #28306, .T. ) ;
#27208 = CARTESIAN_POINT ( 'NONE',  ( 0.000000000000000000, -1.324687536737320328E-14, 29.43090101791767665 ) ) ;
#27209 = CARTESIAN_POINT ( 'NONE',  ( 5.105024945674004222, 42.22604126506330857, -1.500000000000000000 ) ) ;
#27210 = CARTESIAN_POINT ( 'NONE',  ( -15.35797807371378987, 12.83915352957770573, 5.652196082367002106 ) ) ;
#27211 = CARTESIAN_POINT ( 'NONE',  ( -32.98805937973593672, 0.000000000000000000, 13.00000000000000178 ) ) ;
#27212 = ORIENTED_EDGE ( 'NONE', *, *, #18739, .T. ) ;
#27213 = FACE_OUTER_BOUND ( 'NONE', #17625, .T. ) ;
#27214 = AXIS2_PLACEMENT_3D ( 'NONE', #8247, #12937, #1233 ) ;
#27215 = CARTESIAN_POINT ( 'NONE',  ( 40.89187623478217404, -5.790488632116400858, -19.50000000000000355 ) ) ;
#27216 = ORIENTED_EDGE ( 'NONE', *, *, #6930, .F. ) ;
#27217 = CARTESIAN_POINT ( 'NONE',  ( -8.072557715923444732, 14.41080185948837311, 1.500000000000000000 ) ) ;
#27218 = DIRECTION ( 'NONE',  ( 0.9594929736144992560, 0.2817325568414232317, 0.000000000000000000 ) ) ;
#27219 = CARTESIAN_POINT ( 'NONE',  ( -25.72578587384908388, -31.97238736827291561, 29.84495957342102201 ) ) ;
#27220 = ORIENTED_EDGE ( 'NONE', *, *, #18006, .F. ) ;
#27221 = CYLINDRICAL_SURFACE ( 'NONE', #9357, 23.20393738267342698 ) ;
#27222 = AXIS2_PLACEMENT_3D ( 'NONE', #2929, #12447, #28966 ) ;
#27223 = CIRCLE ( 'NONE', #14768, 20.32284676574538906 ) ;
#27224 = PLANE ( 'NONE',  #24510 ) ;
#27225 = AXIS2_PLACEMENT_3D ( 'NONE', #12537, #17198, #14558 ) ;
#27226 = FACE_OUTER_BOUND ( 'NONE', #27790, .T. ) ;
#27227 = CARTESIAN_POINT ( 'NONE',  ( -19.77456323383488268, 2.996942905618072306, 18.47110296274025387 ) ) ;
#27228 = VERTEX_POINT ( 'NONE', #24305 ) ;
#27229 = CARTESIAN_POINT ( 'NONE',  ( -4.100931858250869588, 19.90478481566557178, 1.500000000000000000 ) ) ;
#27230 = CARTESIAN_POINT ( 'NONE',  ( 30.74147208807243103, 15.49548351932574519, 36.33144972441040466 ) ) ;
#27231 = CYLINDRICAL_SURFACE ( 'NONE', #10238, 7.500000000000000000 ) ;
#27232 = CYLINDRICAL_SURFACE ( 'NONE', #317, 23.20393738267338790 ) ;
#27233 = CIRCLE ( 'NONE', #21242, 9.084132297865673777 ) ;
#27234 = CARTESIAN_POINT ( 'NONE',  ( -28.34828976096172681, -29.18752572968383419, -1.500000000000000000 ) ) ;
#27235 = CYLINDRICAL_SURFACE ( 'NONE', #3891, 34.99999999999933920 ) ;
#27236 = CARTESIAN_POINT ( 'NONE',  ( -18.04155359371238987, -8.631455508453164782, 18.34798005863227388 ) ) ;
#27237 = PRESENTATION_LAYER_ASSIGNMENT (  '', '', ( #9803 ) ) ;
#27238 = DIRECTION ( 'NONE',  ( -1.000000000000000000, 0.000000000000000000, 0.000000000000000000 ) ) ;
#27239 = EDGE_LOOP ( 'NONE', ( #19159, #17849, #5049, #17928 ) ) ;
#27240 = DIRECTION ( 'NONE',  ( 1.000000000000000000, -0.000000000000000000, -0.000000000000000000 ) ) ;
#27241 = CARTESIAN_POINT ( 'NONE',  ( 19.64177907938615064, 36.71644397333972876, 24.50000000000000000 ) ) ;
#27242 = AXIS2_PLACEMENT_3D ( 'NONE', #859, #2197, #19043 ) ;
#27243 = ORIENTED_EDGE ( 'NONE', *, *, #21022, .T. ) ;
#27244 = ORIENTED_EDGE ( 'NONE', *, *, #8081, .T. ) ;
#27245 = VECTOR ( 'NONE', #19513, 1000.000000000000000 ) ;
#27246 = FACE_OUTER_BOUND ( 'NONE', #14887, .T. ) ;
#27247 = CARTESIAN_POINT ( 'NONE',  ( 15.75094665830062723, -12.32508334119354210, 24.50000000000000000 ) ) ;
#27248 = LINE ( 'NONE', #29738, #14877 ) ;
#27249 = CIRCLE ( 'NONE', #8335, 2.999999999999999112 ) ;
#27250 = ORIENTED_EDGE ( 'NONE', *, *, #6330, .T. ) ;
#27251 = AXIS2_PLACEMENT_3D ( 'NONE', #25596, #13739, #6101 ) ;
#27252 = LINE ( 'NONE', #13071, #2436 ) ;
#27253 = CARTESIAN_POINT ( 'NONE',  ( 15.55631266752686770, 12.59833113950373651, 19.33715507985239412 ) ) ;
#27254 = VERTEX_POINT ( 'NONE', #5597 ) ;
#27255 = ORIENTED_EDGE ( 'NONE', *, *, #12030, .T. ) ;
#27256 = EDGE_CURVE ( 'NONE', #29319, #25416, #4974, .T. ) ;
#27257 = CARTESIAN_POINT ( 'NONE',  ( 15.81223571690235019, -6.365019318618786670, 20.34789198813115263 ) ) ;
#27258 = CARTESIAN_POINT ( 'NONE',  ( 19.66823596311670030, 3.724077645907920342, 20.19593175699879595 ) ) ;
#27259 = CIRCLE ( 'NONE', #29750, 23.20393738267342698 ) ;
#27260 = DIRECTION ( 'NONE',  ( 0.000000000000000000, 0.000000000000000000, 1.000000000000000000 ) ) ;
#27261 =( BOUNDED_CURVE ( )  B_SPLINE_CURVE ( 3, ( #30522, #28655, #28504, #16797 ),
 .UNSPECIFIED., .F., .T. ) 
 B_SPLINE_CURVE_WITH_KNOTS ( ( 4, 4 ),
 ( 3.955359442064654285, 5.469418518704724619 ),
 .UNSPECIFIED. ) 
 CURVE ( )  GEOMETRIC_REPRESENTATION_ITEM ( )  RATIONAL_B_SPLINE_CURVE ( ( 1.000000000000000000, 0.8179194830933629312, 0.8179194830933629312, 1.000000000000000000 ) ) 
 REPRESENTATION_ITEM ( '' )  );
#27262 = ORIENTED_EDGE ( 'NONE', *, *, #12035, .T. ) ;
#27263 = CARTESIAN_POINT ( 'NONE',  ( -5.058868514795364923, 16.26385723645295656, 20.22273502201483453 ) ) ;
#27264 = ORIENTED_EDGE ( 'NONE', *, *, #20655, .T. ) ;
#27265 = DIRECTION ( 'NONE',  ( -0.000000000000000000, -0.000000000000000000, 1.000000000000000000 ) ) ;
#27266 = CIRCLE ( 'NONE', #12329, 0.7500000000000006661 ) ;
#27267 = ORIENTED_EDGE ( 'NONE', *, *, #1264, .F. ) ;
#27268 = AXIS2_PLACEMENT_3D ( 'NONE', #22996, #8674, #25038 ) ;
#27269 = DIRECTION ( 'NONE',  ( 0.000000000000000000, 1.000000000000000000, 0.000000000000000000 ) ) ;
#27270 = CARTESIAN_POINT ( 'NONE',  ( 35.81403885549343613, -16.83674392041570655, 31.37468618001539156 ) ) ;
#27271 = CARTESIAN_POINT ( 'NONE',  ( 16.56823697822720476, 4.133291823432031720, 6.995624166085161910 ) ) ;
#27272 = CARTESIAN_POINT ( 'NONE',  ( -12.86036580545043506, 11.15762522838069515, 18.71435384576123440 ) ) ;
#27273 = VECTOR ( 'NONE', #15936, 1000.000000000000000 ) ;
#27274 = CARTESIAN_POINT ( 'NONE',  ( -9.785592877189488448, -17.46290528139148179, 19.89182036555910571 ) ) ;
#27275 = LINE ( 'NONE', #5908, #17520 ) ;
#27276 = CARTESIAN_POINT ( 'NONE',  ( -19.90092023446657521, 2.162276205174162858, 18.39992786714538298 ) ) ;
#27277 = CARTESIAN_POINT ( 'NONE',  ( 26.80246859415415273, 7.028748154183637631, -1.499999999999999556 ) ) ;
#27278 = ORIENTED_EDGE ( 'NONE', *, *, #2301, .T. ) ;
#27279 = FACE_OUTER_BOUND ( 'NONE', #20867, .T. ) ;
#27280 = VECTOR ( 'NONE', #28076, 1000.000000000000000 ) ;
#27281 = CARTESIAN_POINT ( 'NONE',  ( -29.91502160997805149, 27.26821511153454480, 16.94723710781324399 ) ) ;
#27282 = LINE ( 'NONE', #3575, #21507 ) ;
#27283 = VECTOR ( 'NONE', #3690, 1000.000000000000000 ) ;
#27284 = VERTEX_POINT ( 'NONE', #14638 ) ;
#27285 = ORIENTED_EDGE ( 'NONE', *, *, #1560, .T. ) ;
#27286 = CARTESIAN_POINT ( 'NONE',  ( 18.08129319977584615, -8.548428815984330242, 18.54479204710283469 ) ) ;
#27287 = EDGE_CURVE ( 'NONE', #14759, #1559, #6627, .T. ) ;
#27288 = CARTESIAN_POINT ( 'NONE',  ( 11.00066062335189798, -16.70338693167701649, 5.651480102388687143 ) ) ;
#27289 = EDGE_CURVE ( 'NONE', #5438, #15872, #30527, .T. ) ;
#27290 = DIRECTION ( 'NONE',  ( -0.000000000000000000, -0.000000000000000000, 1.000000000000000000 ) ) ;
#27291 = VERTEX_POINT ( 'NONE', #19943 ) ;
#27292 = CARTESIAN_POINT ( 'NONE',  ( 0.000000000000000000, 0.000000000000000000, 85.49999999999998579 ) ) ;
#27293 = VECTOR ( 'NONE', #11503, 1000.000000000000000 ) ;
#27294 = CARTESIAN_POINT ( 'NONE',  ( 6.812559277181973627, -5.881244434206257310, 21.50000000000000000 ) ) ;
#27295 = EDGE_CURVE ( 'NONE', #9423, #15798, #13120, .T. ) ;
#27296 = CARTESIAN_POINT ( 'NONE',  ( 6.140972302510982139, 19.03394436102034604, 7.156831654632813233 ) ) ;
#27297 = ORIENTED_EDGE ( 'NONE', *, *, #8394, .F. ) ;
#27298 = EDGE_CURVE ( 'NONE', #12912, #17814, #29768, .T. ) ;
#27299 = CARTESIAN_POINT ( 'NONE',  ( -9.658933677579518928, -17.51307076256854600, 19.08830981656262082 ) ) ;
#27300 = CARTESIAN_POINT ( 'NONE',  ( 14.74216733233971510, 13.54174064842195691, 5.678370764302467677 ) ) ;
#27301 = CARTESIAN_POINT ( 'NONE',  ( 16.85539258114951267, 2.401441585233818010, 7.272049892295485485 ) ) ;
#27302 = ORIENTED_EDGE ( 'NONE', *, *, #13942, .F. ) ;
#27303 = DIRECTION ( 'NONE',  ( -0.9096319953545185522, 0.4154150130018859355, 0.000000000000000000 ) ) ;
#27304 = VERTEX_POINT ( 'NONE', #20694 ) ;
#27305 = AXIS2_PLACEMENT_3D ( 'NONE', #14806, #12789, #2805 ) ;
#27306 = ADVANCED_FACE ( 'NONE', ( #8095 ), #29765, .T. ) ;
#27307 = CARTESIAN_POINT ( 'NONE',  ( -13.99139173414502579, 9.791236547350349539, 19.08844262864049668 ) ) ;
#27308 = CARTESIAN_POINT ( 'NONE',  ( 31.10500197267672817, -15.38309308716404900, 36.05646065676224765 ) ) ;
#27309 = VERTEX_POINT ( 'NONE', #8406 ) ;
#27310 = EDGE_CURVE ( 'NONE', #29057, #11684, #15234, .T. ) ;
#27311 = AXIS2_PLACEMENT_3D ( 'NONE', #15241, #8713, #29933 ) ;
#27312 = VERTEX_POINT ( 'NONE', #24762 ) ;
#27313 = EDGE_CURVE ( 'NONE', #19828, #7486, #24957, .T. ) ;
#27314 = CARTESIAN_POINT ( 'NONE',  ( 3.835725748988833672, 16.61467071301744269, 7.627891251804737927 ) ) ;
#27315 = DIRECTION ( 'NONE',  ( -0.000000000000000000, 1.132880637372608986E-16, -1.000000000000000000 ) ) ;
#27316 = CARTESIAN_POINT ( 'NONE',  ( 5.352643706120463918, 7.827050521741900191, 13.00000000000000178 ) ) ;
#27317 = VECTOR ( 'NONE', #13117, 1000.000000000000000 ) ;
#27318 = CARTESIAN_POINT ( 'NONE',  ( 0.3567158762617962386, -19.99681059701335073, 18.34798005863227388 ) ) ;
#27319 = DIRECTION ( 'NONE',  ( 1.000000000000000000, 0.000000000000000000, 0.000000000000000000 ) ) ;
#27320 = CARTESIAN_POINT ( 'NONE',  ( 19.84141769772507402, 2.653416696629038007, 20.19668224736330941 ) ) ;
#27321 = ORIENTED_EDGE ( 'NONE', *, *, #12862, .T. ) ;
#27322 = B_SPLINE_CURVE_WITH_KNOTS ( 'NONE', 3,
 ( #537, #21596, #24089, #12717, #17229, #29401, #16926, #26913, #389, #15034, #5534, #19571, #26754, #5382, #12100, #14587, #14728, #24549 ),
 .UNSPECIFIED., .F., .F.,
 ( 4, 2, 2, 2, 2, 2, 2, 2, 4 ),
 ( 0.003174295595554313919, 0.003570702171545549284, 0.003967108747536784649, 0.004363515323528019581, 0.004759921899519254512, 0.005156328475510490311, 0.005552735051501725243, 0.005949141627492960174, 0.006345548203484195973 ),
 .UNSPECIFIED. ) ;
#27323 = CARTESIAN_POINT ( 'NONE',  ( -16.82936799811532680, 2.561302842313196493, 19.77662771831109367 ) ) ;
#27324 = CARTESIAN_POINT ( 'NONE',  ( 18.05043922081454610, -8.654756627348808351, 7.359006845440219102 ) ) ;
#27325 = CARTESIAN_POINT ( 'NONE',  ( -13.98072106069838050, 9.805336070574282914, 19.03762469184452755 ) ) ;
#27326 = CARTESIAN_POINT ( 'NONE',  ( -12.72536390617885260, -2.839914339433650348, 1.500000000000001332 ) ) ;
#27327 = CARTESIAN_POINT ( 'NONE',  ( 5.296161872597630271, 19.28602264385380849, 20.34789198813115263 ) ) ;
#27328 = VERTEX_POINT ( 'NONE', #10731 ) ;
#27329 = CARTESIAN_POINT ( 'NONE',  ( 30.29603128833749537, -26.76406484782719275, 17.21603893666378582 ) ) ;
#27330 = ADVANCED_FACE ( 'NONE', ( #15562 ), #3407, .F. ) ;
#27331 = CIRCLE ( 'NONE', #24304, 0.7500000000000006661 ) ;
#27332 = DIRECTION ( 'NONE',  ( 1.000000000000000000, 0.000000000000000000, 0.000000000000000000 ) ) ;
#27333 = ADVANCED_FACE ( 'NONE', ( #13238 ), #6369, .F. ) ;
#27334 = B_SPLINE_SURFACE_WITH_KNOTS ( 'NONE', 3, 1, ( 
 ( #16039, #18076 ),
 ( #4032, #27596 ),
 ( #5913, #8255 ),
 ( #3418, #30230 ),
 ( #29621, #8877 ),
 ( #8419, #24936 ),
 ( #22436, #3573 ),
 ( #27748, #30080 ),
 ( #17762, #17931 ),
 ( #8715, #13558 ),
 ( #1079, #13095 ),
 ( #10592, #10743 ),
 ( #29780, #13250 ),
 ( #10910, #20412 ),
 ( #15724, #4331 ),
 ( #4495, #14004 ),
 ( #6821, #2290 ),
 ( #7288, #6671 ),
 ( #16348, #14292 ),
 ( #4643, #26158 ),
 ( #13858, #9320 ),
 ( #11812, #23502 ),
 ( #2460, #30390 ),
 ( #21317, #16186 ),
 ( #28660, #11371 ),
 ( #112, #14145 ),
 ( #23647, #25862 ),
 ( #9632, #21151 ),
 ( #7142, #23190 ),
 ( #4785, #16653 ),
 ( #30835, #20864 ) ),
 .UNSPECIFIED., .F., .F., .F.,
 ( 4, 3, 3, 3, 3, 3, 3, 3, 3, 3, 4 ),
 ( 2, 2 ),
 ( 0.4999999998345686092, 0.5360336730431939367, 0.5907651151589012883, 0.6456034593241830599, 0.6998270958050434309, 0.7529536536315937223, 0.8052385063053260073, 0.8575343587103997356, 0.9106564858195042023, 0.9648414833209685293, 1.000000006602610014 ),
 ( 0.000000000000000000, 1.000000000000000000 ),
 .UNSPECIFIED. ) ;
#27335 = CARTESIAN_POINT ( 'NONE',  ( -5.279695238918637124, 19.30927203514151103, 20.05479082170252525 ) ) ;
#27336 = CARTESIAN_POINT ( 'NONE',  ( 9.755064781586030520, 13.32952022457704544, 24.50000000000000000 ) ) ;
#27337 = VECTOR ( 'NONE', #8207, 1000.000000000000000 ) ;
#27338 = CARTESIAN_POINT ( 'NONE',  ( 3.662523238938590442, -12.47340865698848056, 1.500000000000001332 ) ) ;
#27339 = CIRCLE ( 'NONE', #18863, 12.50000000000000000 ) ;
#27340 = EDGE_CURVE ( 'NONE', #1637, #20273, #15881, .T. ) ;
#27341 = DIRECTION ( 'NONE',  ( 1.000000000000000000, 0.000000000000000000, 0.000000000000000000 ) ) ;
#27342 = CARTESIAN_POINT ( 'NONE',  ( -33.42925964089141644, -11.06161099612212695, -16.55003854064094426 ) ) ;
#27343 = EDGE_CURVE ( 'NONE', #12499, #4980, #8564, .T. ) ;
#27344 = CARTESIAN_POINT ( 'NONE',  ( 2.516121109503181241, 8.728722367416590799, 13.22130136205108997 ) ) ;
#27345 = VECTOR ( 'NONE', #7252, 1000.000000000000114 ) ;
#27346 = CARTESIAN_POINT ( 'NONE',  ( -33.25379661643704310, 9.265521131796550236, 40.47962024272059267 ) ) ;
#27347 = VERTEX_POINT ( 'NONE', #1537 ) ;
#27348 = VERTEX_POINT ( 'NONE', #25693 ) ;
#27349 = ADVANCED_FACE ( 'NONE', ( #4321 ), #6661, .F. ) ;
#27350 = CARTESIAN_POINT ( 'NONE',  ( -19.80925230797850745, 2.758332870380174384, 7.626647697317573638 ) ) ;
#27351 = CARTESIAN_POINT ( 'NONE',  ( 22.58267429318971864, 26.57182937991349903, 24.50000000000000000 ) ) ;
#27352 = VERTEX_POINT ( 'NONE', #28181 ) ;
#27353 = DIRECTION ( 'NONE',  ( -0.000000000000000000, -0.000000000000000000, -1.000000000000000000 ) ) ;
#27354 = CARTESIAN_POINT ( 'NONE',  ( 19.88570912806761370, 2.296683858978088466, 18.90679857307105749 ) ) ;
#27355 = DIRECTION ( 'NONE',  ( 0.000000000000000000, -1.000000000000000000, 0.000000000000000000 ) ) ;
#27356 = CARTESIAN_POINT ( 'NONE',  ( 52.16608720827707657, 51.86186943028246787, 12.49999999999998401 ) ) ;
#27357 = CARTESIAN_POINT ( 'NONE',  ( 9.131494062835614045, 2.555255504830995061, 21.50000000000000000 ) ) ;
#27358 = CARTESIAN_POINT ( 'NONE',  ( -6.051176437752245008, 19.08139585423913331, 18.34838970509067479 ) ) ;
#27359 = VECTOR ( 'NONE', #6181, 1000.000000000000000 ) ;
#27360 = AXIS2_PLACEMENT_3D ( 'NONE', #10566, #5885, #25060 ) ;
#27361 = DIRECTION ( 'NONE',  ( 0.000000000000000000, 0.000000000000000000, 1.000000000000000000 ) ) ;
#27362 = CARTESIAN_POINT ( 'NONE',  ( 23.17581250239727808, -34.50630206824672541, 1.499999999999999778 ) ) ;
#27363 = CARTESIAN_POINT ( 'NONE',  ( 0.4302108320067680181, -20.01327865860579536, 5.652605728828374865 ) ) ;
#27364 = CARTESIAN_POINT ( 'NONE',  ( -16.83599852036188338, 2.522587596173209601, 6.143977687428010981 ) ) ;
#27365 = VERTEX_POINT ( 'NONE', #20854 ) ;
#27366 = EDGE_CURVE ( 'NONE', #353, #17425, #2150, .T. ) ;
#27367 = EDGE_CURVE ( 'NONE', #5751, #23685, #17090, .T. ) ;
#27368 = VECTOR ( 'NONE', #20604, 1000.000000000000000 ) ;
#27369 = CARTESIAN_POINT ( 'NONE',  ( -11.37681265597470137, -16.47072995046971755, 19.33715507985239412 ) ) ;
#27370 = CARTESIAN_POINT ( 'NONE',  ( -15.01939917408025238, -8.081071717223313300, 7.603368798681074736 ) ) ;
#27371 = CARTESIAN_POINT ( 'NONE',  ( -42.49999999999998579, 50.00000000000000000, 52.07879600563550326 ) ) ;
#27372 = CARTESIAN_POINT ( 'NONE',  ( 10.61155637842189314, -13.37681800088532569, 7.098451512883313441 ) ) ;
#27373 = CARTESIAN_POINT ( 'NONE',  ( -13.22505861668333083, 42.10773672057167261, -19.50000000000000355 ) ) ;
#27374 = AXIS2_PLACEMENT_3D ( 'NONE', #28743, #24362, #14689 ) ;
#27375 = CARTESIAN_POINT ( 'NONE',  ( -32.94612346989018192, 8.892333671926630601, 36.63232123319113498 ) ) ;
#27376 = EDGE_LOOP ( 'NONE', ( #19142, #22519, #22283, #3358 ) ) ;
#27377 = ORIENTED_EDGE ( 'NONE', *, *, #19476, .T. ) ;
#27378 = CARTESIAN_POINT ( 'NONE',  ( 9.864937699929956949, -13.90063973435163724, 18.34798005863078885 ) ) ;
#27379 = CARTESIAN_POINT ( 'NONE',  ( -10.11202017158235833, -41.14070756921188377, -1.500000000000000000 ) ) ;
#27380 = CARTESIAN_POINT ( 'NONE',  ( -13.16299300229363567, 10.81582545713519927, 5.701226463332907279 ) ) ;
#27381 = DIRECTION ( 'NONE',  ( 0.5503133621338236470, 0.8349582046168341209, 0.000000000000000000 ) ) ;
#27382 = VERTEX_POINT ( 'NONE', #16339 ) ;
#27383 = DIRECTION ( 'NONE',  ( 0.000000000000000000, 0.000000000000000000, -1.000000000000000000 ) ) ;
#27384 = CARTESIAN_POINT ( 'NONE',  ( 39.83602371822922095, -11.57901747687539640, -19.50000000000000355 ) ) ;
#27385 = CARTESIAN_POINT ( 'NONE',  ( -9.011666854301585872, -14.45189732017202644, 7.500898271101006820 ) ) ;
#27386 = ORIENTED_EDGE ( 'NONE', *, *, #8502, .T. ) ;
#27387 = AXIS2_PLACEMENT_3D ( 'NONE', #2553, #21559, #4885 ) ;
#27388 = CYLINDRICAL_SURFACE ( 'NONE', #13831, 20.00000000000000355 ) ;
#27389 = CARTESIAN_POINT ( 'NONE',  ( -6.588341431580430729, -36.93554111252256433, 37.49999999995496580 ) ) ;
#27390 = ORIENTED_EDGE ( 'NONE', *, *, #20240, .F. ) ;
#27391 = FACE_OUTER_BOUND ( 'NONE', #12014, .T. ) ;
#27392 = FACE_OUTER_BOUND ( 'NONE', #5353, .T. ) ;
#27393 = AXIS2_PLACEMENT_3D ( 'NONE', #23410, #23553, #11717 ) ;
#27394 = PLANE ( 'NONE',  #6838 ) ;
#27395 = B_SPLINE_CURVE_WITH_KNOTS ( 'NONE', 3,
 ( #12581, #7439, #16943, #23796, #3060, #17250, #26462, #26620, #28646, #253, #19587, #14451, #7745, #24266, #2599, #23954, #2756, #12118, #5247, #9926, #5092, #26776, #9620, #17093, #9766, #19278 ),
 .UNSPECIFIED., .F., .F.,
 ( 4, 2, 2, 2, 1, 2, 2, 2, 2, 2, 2, 1, 2, 4 ),
 ( 0.5002013267716731715, 0.5119551913427370371, 0.5237090559138010137, 0.5354629204848648794, 0.5413398527703968677, 0.5442783189131628063, 0.5472167850559288560, 0.5589706496269926106, 0.5707245141980563652, 0.5766014464835882425, 0.5824783787691202308, 0.5883553110546521081, 0.5912937771974180468, 0.5942322433401839854 ),
 .UNSPECIFIED. ) ;
#27396 = CARTESIAN_POINT ( 'NONE',  ( -19.75724448635271102, 3.108068420208395910, 18.54479204710283824 ) ) ;
#27397 = VERTEX_POINT ( 'NONE', #18530 ) ;
#27398 = CARTESIAN_POINT ( 'NONE',  ( 2.555255504830960867, -9.131494062835622927, 13.00000000000000178 ) ) ;
#27399 = CARTESIAN_POINT ( 'NONE',  ( -25.64627119138473432, -23.40052582045089480, -6.500000000000000888 ) ) ;
#27400 = DIRECTION ( 'NONE',  ( 1.000000000000000000, 0.000000000000000000, -0.000000000000000000 ) ) ;
#27401 = CYLINDRICAL_SURFACE ( 'NONE', #17269, 20.00000000000000000 ) ;
#27402 = CARTESIAN_POINT ( 'NONE',  ( -17.06629969734983376, 0.6399978984115163305, 6.783738457429056901 ) ) ;
#27404 = EDGE_CURVE ( 'NONE', #27728, #14860, #28533, .T. ) ;
#27403 = DIRECTION ( 'NONE',  ( 0.000000000000000000, 0.000000000000000000, -1.000000000000000000 ) ) ;
#27405 = CARTESIAN_POINT ( 'NONE',  ( -2.959227181723746547, 8.499586724479465616, -3.621320343559650379 ) ) ;
#27406 = CYLINDRICAL_SURFACE ( 'NONE', #3961, 0.7499999999999997780 ) ;
#27407 = VERTEX_POINT ( 'NONE', #30662 ) ;
#27408 = CARTESIAN_POINT ( 'NONE',  ( 36.00000000000000000, -1.546978760965586295E-11, 34.75735931288068059 ) ) ;
#27409 = CIRCLE ( 'NONE', #6490, 7.500000000000013323 ) ;
#27410 = CARTESIAN_POINT ( 'NONE',  ( -9.390093949354151093, -14.19700018541476005, 19.47784884541372463 ) ) ;
#27411 = VERTEX_POINT ( 'NONE', #11362 ) ;
#27412 = EDGE_LOOP ( 'NONE', ( #30441, #6808, #27768, #16510 ) ) ;
#27413 = DIRECTION ( 'NONE',  ( -0.4154150130018973153, -0.9096319953545134451, 0.000000000000000000 ) ) ;
#27414 = CARTESIAN_POINT ( 'NONE',  ( 40.89187623478217404, 5.790488632116406187, -19.50000000000000355 ) ) ;
#27415 = DIRECTION ( 'NONE',  ( 0.000000000000000000, 0.000000000000000000, 1.000000000000000000 ) ) ;
#27416 = ORIENTED_EDGE ( 'NONE', *, *, #4625, .F. ) ;
#27417 =( LENGTH_UNIT ( ) NAMED_UNIT ( * ) SI_UNIT ( .MILLI., .METRE. ) );
#27418 = VECTOR ( 'NONE', #4462, 1000.000000000000000 ) ;
#27419 = CARTESIAN_POINT ( 'NONE',  ( -5.800828033945498063, 16.03801949172214591, 18.34938820207544907 ) ) ;
#27420 = CARTESIAN_POINT ( 'NONE',  ( -50.00000000000000000, -50.00000000000000000, 59.49999999999999289 ) ) ;
#27421 = EDGE_LOOP ( 'NONE', ( #1426, #27036 ) ) ;
#27422 = ORIENTED_EDGE ( 'NONE', *, *, #18316, .T. ) ;
#27423 = DIRECTION ( 'NONE',  ( -0.000000000000000000, -0.000000000000000000, 1.000000000000000000 ) ) ;
#27424 = CARTESIAN_POINT ( 'NONE',  ( 18.33599632111990019, -7.986941774664177096, 7.652108011868850035 ) ) ;
#27425 = CARTESIAN_POINT ( 'NONE',  ( 14.87898868866547097, 13.36471831362574747, 5.652196082369964181 ) ) ;
#27426 = CARTESIAN_POINT ( 'NONE',  ( -8.848822535149219348, 41.41987577336931992, 28.93372982618284794 ) ) ;
#27427 = ORIENTED_EDGE ( 'NONE', *, *, #3304, .F. ) ;
#27428 = FACE_OUTER_BOUND ( 'NONE', #17572, .T. ) ;
#27429 = VERTEX_POINT ( 'NONE', #9160 ) ;
#27430 = AXIS2_PLACEMENT_3D ( 'NONE', #8484, #17831, #29371 ) ;
#27431 = DIRECTION ( 'NONE',  ( -0.000000000000000000, -1.000000000000000000, -0.000000000000000000 ) ) ;
#27432 = ORIENTED_EDGE ( 'NONE', *, *, #5385, .F. ) ;
#27433 = CARTESIAN_POINT ( 'NONE',  ( 6.974883619896790954, 5.687793815610376669, 1.500000000000001332 ) ) ;
#27434 = LINE ( 'NONE', #24610, #26285 ) ;
#27435 = CARTESIAN_POINT ( 'NONE',  ( -3.196529495465446402, -8.413215745754985875, -3.621320343559650379 ) ) ;
#27436 = CARTESIAN_POINT ( 'NONE',  ( -8.487288213245033575, -14.78455279991285387, 20.34789198813115263 ) ) ;
#27437 = CARTESIAN_POINT ( 'NONE',  ( -57.50000000000001421, -50.00000000000000000, 12.49999999999999112 ) ) ;
#27438 = CARTESIAN_POINT ( 'NONE',  ( -9.069887158786405834, -14.41355491436599046, 5.848946451764559740 ) ) ;
#27439 = CARTESIAN_POINT ( 'NONE',  ( 9.169883732660084164, -9.268939115642975679, 24.50000000000000000 ) ) ;
#27440 = EDGE_LOOP ( 'NONE', ( #12553, #2438, #22302, #19012 ) ) ;
#27441 = DIRECTION ( 'NONE',  ( 0.2817325568414296710, -0.9594929736144973687, 0.000000000000000000 ) ) ;
#27442 = DIRECTION ( 'NONE',  ( 0.000000000000000000, 0.000000000000000000, 1.000000000000000000 ) ) ;
#27443 = LINE ( 'NONE', #6064, #10600 ) ;
#27444 = EDGE_LOOP ( 'NONE', ( #9318, #25802, #21649, #27199 ) ) ;
#27445 = VERTEX_POINT ( 'NONE', #18674 ) ;
#27446 = CARTESIAN_POINT ( 'NONE',  ( 49.99999999999998579, 50.00000000000000000, 59.49999999999999289 ) ) ;
#27447 = DIRECTION ( 'NONE',  ( -0.000000000000000000, -0.000000000000000000, 1.000000000000000000 ) ) ;
#27448 = CARTESIAN_POINT ( 'NONE',  ( -5.055631408663416870, 19.36903233965647786, 6.310736198168394928 ) ) ;
#27449 = VERTEX_POINT ( 'NONE', #6811 ) ;
#27450 = DIRECTION ( 'NONE',  ( 0.000000000000000000, 0.000000000000000000, 1.000000000000000000 ) ) ;
#27451 = VECTOR ( 'NONE', #3090, 1000.000000000000000 ) ;
#27452 = DIRECTION ( 'NONE',  ( 0.000000000000000000, -1.132880637372608986E-16, 1.000000000000000000 ) ) ;
#27453 = CARTESIAN_POINT ( 'NONE',  ( 0.1262659238204208167, 8.999114229549594057, 21.50000000000000000 ) ) ;
#27454 = B_SPLINE_CURVE_WITH_KNOTS ( 'NONE', 3,
 ( #6373, #4173, #11050, #23187, #11365, #29773, #13245, #25084, #29931, #20858, #9023, #30225, #15407, #1540, #6057, #13090 ),
 .UNSPECIFIED., .F., .F.,
 ( 4, 2, 2, 2, 2, 2, 2, 4 ),
 ( 0.4999999999999999445, 0.6250000000000012212, 0.6875000000000018874, 0.7187500000000022204, 0.7500000000000026645, 0.8125000000000016653, 0.8750000000000006661, 1.000000000000000000 ),
 .UNSPECIFIED. ) ;
#27455 = ORIENTED_EDGE ( 'NONE', *, *, #2602, .F. ) ;
#27456 = DIRECTION ( 'NONE',  ( 0.000000000000000000, 0.000000000000000000, 1.000000000000000000 ) ) ;
#27457 = CARTESIAN_POINT ( 'NONE',  ( 11.65818676052303182, 12.48028922388247786, 6.560937769032974209 ) ) ;
#27458 = CARTESIAN_POINT ( 'NONE',  ( 16.76146518920504391, 3.081792779576176589, 7.652108011868850035 ) ) ;
#27459 = EDGE_LOOP ( 'NONE', ( #2196, #5624, #157, #10646 ) ) ;
#27460 = DIRECTION ( 'NONE',  ( 0.000000000000000000, 0.000000000000000000, 1.000000000000000000 ) ) ;
#27461 = ORIENTED_EDGE ( 'NONE', *, *, #19665, .F. ) ;
#27462 = CARTESIAN_POINT ( 'NONE',  ( -13.93204262645545377, 9.869472133065979591, 19.85459532544248518 ) ) ;
#27463 = ORIENTED_EDGE ( 'NONE', *, *, #5558, .T. ) ;
#27464 = ORIENTED_EDGE ( 'NONE', *, *, #24475, .F. ) ;
#27465 = CARTESIAN_POINT ( 'NONE',  ( 4.537370253389202190, 19.49663512434673507, 7.280727868105637768 ) ) ;
#27466 = CARTESIAN_POINT ( 'NONE',  ( 5.889883548616668740, 19.11329876149440565, 20.14992337338002670 ) ) ;
#27467 = ORIENTED_EDGE ( 'NONE', *, *, #2134, .F. ) ;
#27468 = CIRCLE ( 'NONE', #30439, 0.7500000000000006661 ) ;
#27469 = EDGE_CURVE ( 'NONE', #9122, #15261, #28033, .T. ) ;
#27470 = CARTESIAN_POINT ( 'NONE',  ( -23.69412710310941605, -29.84645176427128987, 27.50000000000000355 ) ) ;
#27471 = DIRECTION ( 'NONE',  ( -0.000000000000000000, -0.000000000000000000, 1.000000000000000000 ) ) ;
#27472 = ORIENTED_EDGE ( 'NONE', *, *, #652, .F. ) ;
#27473 = EDGE_CURVE ( 'NONE', #21864, #24108, #7452, .T. ) ;
#27474 = CARTESIAN_POINT ( 'NONE',  ( -19.70934530863873491, 3.501268498360766923, 19.45164628100866722 ) ) ;
#27475 = CARTESIAN_POINT ( 'NONE',  ( 15.76678477342441731, -6.469363178373289891, 7.652108011868850035 ) ) ;
#27476 = CARTESIAN_POINT ( 'NONE',  ( -15.35797660355606986, 12.83915183367558832, 18.34798005862662507 ) ) ;
#27477 = CARTESIAN_POINT ( 'NONE',  ( 4.523123428450326777, 19.49994255397358600, 18.73743063545763121 ) ) ;
#27478 = ORIENTED_EDGE ( 'NONE', *, *, #803, .T. ) ;
#27479 = ORIENTED_EDGE ( 'NONE', *, *, #30170, .F. ) ;
#27480 = CARTESIAN_POINT ( 'NONE',  ( 64.99999999999998579, 36.86186943028246787, 12.49999999999999112 ) ) ;
#27482 = ADVANCED_FACE ( 'NONE', ( #24222 ), #23183, .F. ) ;
#27481 = CARTESIAN_POINT ( 'NONE',  ( 14.83584055149749759, 17.84153987719500734, 1.500000000000000000 ) ) ;
#27483 = AXIS2_PLACEMENT_3D ( 'NONE', #15001, #12527, #17351 ) ;
#27484 = CARTESIAN_POINT ( 'NONE',  ( -4.850186825639134724, 16.32197540402032487, 20.05479082170252525 ) ) ;
#27485 =( NAMED_UNIT ( * ) PLANE_ANGLE_UNIT ( ) SI_UNIT ( $, .RADIAN. ) );
#27486 = FACE_OUTER_BOUND ( 'NONE', #1668, .T. ) ;
#27487 = EDGE_CURVE ( 'NONE', #17387, #11174, #25062, .T. ) ;
#27488 = CARTESIAN_POINT ( 'NONE',  ( 4.390207617113956573, -7.856594496258208160, 21.50000000000000000 ) ) ;
#27489 = EDGE_CURVE ( 'NONE', #8808, #27445, #18388, .T. ) ;
#27490 = CARTESIAN_POINT ( 'NONE',  ( 16.83255095306759586, 2.584307790288491891, 5.848946451764563292 ) ) ;
#27491 = VERTEX_POINT ( 'NONE', #15487 ) ;
#27492 = VECTOR ( 'NONE', #5872, 1000.000000000000000 ) ;
#27493 = DIRECTION ( 'NONE',  ( -0.000000000000000000, -0.000000000000000000, -1.000000000000000000 ) ) ;
#27494 = ORIENTED_EDGE ( 'NONE', *, *, #20023, .T. ) ;
#27495 = CARTESIAN_POINT ( 'NONE',  ( -33.43024933835881285, 9.611735609129382851, 40.21560466195906258 ) ) ;
#27496 = CARTESIAN_POINT ( 'NONE',  ( -37.16608720827707657, 65.00000000000000000, 97.07879600563551037 ) ) ;
#27497 = VERTEX_POINT ( 'NONE', #12550 ) ;
#27498 = VERTEX_POINT ( 'NONE', #26735 ) ;
#27499 = LINE ( 'NONE', #17666, #4306 ) ;
#27500 = LINE ( 'NONE', #6120, #29473 ) ;
#27501 = VERTEX_POINT ( 'NONE', #8024 ) ;
#27502 = CARTESIAN_POINT ( 'NONE',  ( 0.09286997694517430679, -20.00015982525766489, 5.676722608126684833 ) ) ;
#27503 = ADVANCED_FACE ( 'NONE', ( #1144 ), #17677, .F. ) ;
#27504 = CARTESIAN_POINT ( 'NONE',  ( 14.20503062814195872, 47.93995967969133432, -50.15627268418315765 ) ) ;
#27505 = EDGE_CURVE ( 'NONE', #4071, #13536, #16096, .T. ) ;
#27506 = CARTESIAN_POINT ( 'NONE',  ( 0.000000000000000000, 15.00000000000001421, 117.5000000000000000 ) ) ;
#27507 = EDGE_CURVE ( 'NONE', #13582, #1637, #12627, .T. ) ;
#27508 = CARTESIAN_POINT ( 'NONE',  ( -20.45518110071315832, -26.46109910111415431, -16.50001200000000168 ) ) ;
#27509 = DIRECTION ( 'NONE',  ( 0.000000000000000000, 1.000000000000000000, 0.000000000000000000 ) ) ;
#27510 = CARTESIAN_POINT ( 'NONE',  ( 11.21147646446735102, 30.29926891764210595, 1.500000000000000000 ) ) ;
#27511 = DIRECTION ( 'NONE',  ( 0.000000000000000000, 1.000000000000000000, 0.000000000000000000 ) ) ;
#27512 = ORIENTED_EDGE ( 'NONE', *, *, #30347, .F. ) ;
#27513 = EDGE_CURVE ( 'NONE', #29598, #18738, #21551, .T. ) ;
#27514 = AXIS2_PLACEMENT_3D ( 'NONE', #18215, #25541, #18381 ) ;
#27515 = CARTESIAN_POINT ( 'NONE',  ( -10.72135862580927146, -16.90494006806149940, 20.32842677360128292 ) ) ;
#27516 = CARTESIAN_POINT ( 'NONE',  ( -14.92657760816262424, -8.264136099378397660, 7.500147780736496017 ) ) ;
#27517 = ADVANCED_FACE ( 'NONE', ( #12704 ), #7715, .F. ) ;
#27518 = CARTESIAN_POINT ( 'NONE',  ( -6.185259412586024297, 19.03819474808296874, 7.627891251804737927 ) ) ;
#27519 = CARTESIAN_POINT ( 'NONE',  ( 10.62299781869221960, -13.36838230995977206, 6.233981582756856987 ) ) ;
#27520 = EDGE_CURVE ( 'NONE', #29034, #20557, #5829, .T. ) ;
#27521 = CARTESIAN_POINT ( 'NONE',  ( -25.19442432475474902, -35.44676296258422354, -19.50000000000000355 ) ) ;
#27522 = CARTESIAN_POINT ( 'NONE',  ( -33.37677408195396112, 9.488883682882484294, 36.05808397461573378 ) ) ;
#27523 = ORIENTED_EDGE ( 'NONE', *, *, #14389, .T. ) ;
#27524 = ORIENTED_EDGE ( 'NONE', *, *, #24076, .T. ) ;
#27525 = DIRECTION ( 'NONE',  ( 1.000000000000000000, 0.000000000000000000, 0.000000000000000000 ) ) ;
#27526 = CARTESIAN_POINT ( 'NONE',  ( 20.65888525914375862, -38.75220717792901581, -19.50000000000000355 ) ) ;
#27527 = CARTESIAN_POINT ( 'NONE',  ( -1.946983950544124875, -37.46784418063916178, 37.49999999996633449 ) ) ;
#27529 = VECTOR ( 'NONE', #11979, 1000.000000000000000 ) ;
#27528 = CARTESIAN_POINT ( 'NONE',  ( 0.000000000000000000, 10.00000000000000888, 117.5000000000000000 ) ) ;
#27530 = VERTEX_POINT ( 'NONE', #20015 ) ;
#27531 = DIRECTION ( 'NONE',  ( 0.000000000000000000, 0.000000000000000000, 1.000000000000000000 ) ) ;
#27532 = CARTESIAN_POINT ( 'NONE',  ( 10.64374042650142904, 42.96126232887663576, -19.50000000000000355 ) ) ;
#27533 = CARTESIAN_POINT ( 'NONE',  ( -9.223046300750478821, -14.31106556781055694, 7.272049892295485485 ) ) ;
#27534 = EDGE_CURVE ( 'NONE', #27498, #3343, #8320, .T. ) ;
#27535 = ORIENTED_EDGE ( 'NONE', *, *, #19665, .T. ) ;
#27536 = ADVANCED_FACE ( 'NONE', ( #10193 ), #19701, .F. ) ;
#27537 = DIRECTION ( 'NONE',  ( -0.000000000000000000, -0.000000000000000000, -1.000000000000000000 ) ) ;
#27538 = CARTESIAN_POINT ( 'NONE',  ( -18.19086450879680683, -37.70413644374980322, 29.27365136405585488 ) ) ;
#27539 = ORIENTED_EDGE ( 'NONE', *, *, #15090, .T. ) ;
#27540 = CARTESIAN_POINT ( 'NONE',  ( -8.499586724479453181, -2.959227181723774525, -1.500000000000002220 ) ) ;
#27541 = ADVANCED_FACE ( 'NONE', ( #5674 ), #14873, .F. ) ;
#27542 = CARTESIAN_POINT ( 'NONE',  ( -17.79239818699324616, -14.89473990422481187, 1.500000000000000000 ) ) ;
#27543 = ORIENTED_EDGE ( 'NONE', *, *, #2031, .F. ) ;
#27544 = CARTESIAN_POINT ( 'NONE',  ( 23.15418787629628739, 10.94208358504856804, 45.14840481401043348 ) ) ;
#27545 = AXIS2_PLACEMENT_3D ( 'NONE', #9418, #7064, #16573 ) ;
#27546 = AXIS2_PLACEMENT_3D ( 'NONE', #2989, #5165, #24495 ) ;
#27547 = CARTESIAN_POINT ( 'NONE',  ( 30.86161751192251756, 15.46691422980912911, 36.23697955569760865 ) ) ;
#27548 = CARTESIAN_POINT ( 'NONE',  ( 16.19472973927114268, -5.422090571236383383, 6.588756557121048907 ) ) ;
#27549 = VECTOR ( 'NONE', #26438, 1000.000000000000000 ) ;
#27550 = DIRECTION ( 'NONE',  ( 0.000000000000000000, -0.000000000000000000, -1.000000000000000000 ) ) ;
#27551 = CARTESIAN_POINT ( 'NONE',  ( -17.06630883447662583, 0.6398751886020394020, 6.588756557121049795 ) ) ;
#27552 = DIRECTION ( 'NONE',  ( 0.000000000000000000, 0.000000000000000000, -1.000000000000000000 ) ) ;
#27553 = LINE ( 'NONE', #6179, #4062 ) ;
#27554 = DIRECTION ( 'NONE',  ( 0.000000000000000000, 0.000000000000000000, -1.000000000000000000 ) ) ;
#27555 = FACE_BOUND ( 'NONE', #12921, .T. ) ;
#27556 = CARTESIAN_POINT ( 'NONE',  ( 33.56327786402390245, -10.34181101807379477, 39.87954049117192312 ) ) ;
#27557 = CARTESIAN_POINT ( 'NONE',  ( 0.000000000000000000, 7.347880794884121708E-16, -6.000000000000001776 ) ) ;
#27558 = VERTEX_POINT ( 'NONE', #7865 ) ;
#27559 = ORIENTED_EDGE ( 'NONE', *, *, #6510, .T. ) ;
#27560 = FACE_OUTER_BOUND ( 'NONE', #15523, .T. ) ;
#27561 = CARTESIAN_POINT ( 'NONE',  ( -39.83602371821029919, -11.57901747687044924, -19.50000000000000355 ) ) ;
#27562 = DIRECTION ( 'NONE',  ( 1.000000000000000000, 0.000000000000000000, -0.000000000000000000 ) ) ;
#27563 = EDGE_LOOP ( 'NONE', ( #7475, #13890 ) ) ;
#27564 = CARTESIAN_POINT ( 'NONE',  ( -9.454746441592954298, 0.7220001660363460916, 21.50000000000000000 ) ) ;
#27565 = FACE_OUTER_BOUND ( 'NONE', #19188, .T. ) ;
#27566 = VECTOR ( 'NONE', #23349, 1000.000000000000000 ) ;
#27567 = EDGE_CURVE ( 'NONE', #30087, #2787, #8331, .T. ) ;
#27568 = ORIENTED_EDGE ( 'NONE', *, *, #9784, .F. ) ;
#27569 = ORIENTED_EDGE ( 'NONE', *, *, #21582, .F. ) ;
#27570 = AXIS2_PLACEMENT_3D ( 'NONE', #17471, #3263, #12791 ) ;
#27571 = CARTESIAN_POINT ( 'NONE',  ( -10.73812863781238036, -16.87327681817511049, 20.32243167357988867 ) ) ;
#27572 = DIRECTION ( 'NONE',  ( -0.000000000000000000, -0.000000000000000000, 1.000000000000000000 ) ) ;
#27573 = CARTESIAN_POINT ( 'NONE',  ( 15.45664188325221744, 12.69231265181876367, 7.156831654632818562 ) ) ;
#27574 = CARTESIAN_POINT ( 'NONE',  ( -15.69812257003878742, 38.91317198416786738, 34.53890312238223714 ) ) ;
#27575 = EDGE_LOOP ( 'NONE', ( #13223, #16499, #25335, #21991 ) ) ;
#27576 = CARTESIAN_POINT ( 'NONE',  ( -5.423201225924849211, 16.15625638780175066, 18.34727598691067740 ) ) ;
#27578 = ORIENTED_EDGE ( 'NONE', *, *, #19867, .F. ) ;
#27577 = VECTOR ( 'NONE', #20794, 1000.000000000000000 ) ;
#27579 = CARTESIAN_POINT ( 'NONE',  ( -14.72786953156476386, -8.642539778695532249, 6.329955581934036069 ) ) ;
#27580 = CARTESIAN_POINT ( 'NONE',  ( -16.81375614428661791, 2.649924382790542765, 19.21496526180054332 ) ) ;
#27581 = ORIENTED_EDGE ( 'NONE', *, *, #29770, .F. ) ;
#27582 = CARTESIAN_POINT ( 'NONE',  ( -6.458857079296002723, 18.92875833827540788, 18.47531940416306284 ) ) ;
#27583 = CARTESIAN_POINT ( 'NONE',  ( 36.48404635224623149, -15.03172480188603899, 31.53210484354143617 ) ) ;
#27584 = B_SPLINE_SURFACE_WITH_KNOTS ( 'NONE', 3, 1, ( 
 ( #13010, #20167 ),
 ( #27363, #17527 ),
 ( #29688, #24688 ),
 ( #17679, #3330 ),
 ( #8332, #998 ),
 ( #17846, #7716 ),
 ( #17213, #26736 ),
 ( #14874, #24386 ),
 ( #1470, #13633 ),
 ( #19021, #27658 ),
 ( #29828, #18301 ),
 ( #11847, #9501 ),
 ( #27822, #28531 ),
 ( #3798, #16518 ),
 ( #25153, #13483 ),
 ( #14329, #28384 ),
 ( #3963, #8947 ),
 ( #23111, #26184 ),
 ( #10981, #15796 ),
 ( #1619, #20480 ),
 ( #21344, #22964 ),
 ( #15641, #7008 ),
 ( #26034, #2319 ),
 ( #7165, #1758 ),
 ( #30000, #16676 ),
 ( #4816, #23841 ),
 ( #11274, #20771 ),
 ( #8638, #20627 ),
 ( #13320, #30299 ),
 ( #18870, #4667 ),
 ( #14169, #18149 ) ),
 .UNSPECIFIED., .F., .F., .F.,
 ( 4, 3, 3, 3, 3, 3, 3, 3, 3, 3, 4 ),
 ( 2, 2 ),
 ( 0.4999999998345682761, 0.5360336730431942698, 0.5907651151589017324, 0.6456034593241839481, 0.6998270958050443191, 0.7529536536315944995, 0.8052385063053264513, 0.8575343587103996246, 0.9106564858195047574, 0.9648414833209688624, 1.000000006602610014 ),
 ( 0.000000000000000000, 1.000000000000000000 ),
 .UNSPECIFIED. ) ;
#27585 = CARTESIAN_POINT ( 'NONE',  ( 19.58381725123993888, 4.144794415032111878, 6.341840715582230281 ) ) ;
#27586 = CARTESIAN_POINT ( 'NONE',  ( -15.35797807371378987, 12.83915352957770750, 18.34798005862930736 ) ) ;
#27587 = AXIS2_PLACEMENT_3D ( 'NONE', #11938, #24073, #21730 ) ;
#27588 = CARTESIAN_POINT ( 'NONE',  ( 1.305293688651088413, -17.01213356653430964, 7.545655578832111132 ) ) ;
#27589 = DIRECTION ( 'NONE',  ( -0.000000000000000000, -0.000000000000000000, -1.000000000000000000 ) ) ;
#27590 = VECTOR ( 'NONE', #19031, 1000.000000000000000 ) ;
#27591 = CARTESIAN_POINT ( 'NONE',  ( -19.88823125026085492, 2.273432466552574027, 18.37415474056476938 ) ) ;
#27592 = CARTESIAN_POINT ( 'NONE',  ( 1.000000000000008438, 13.00000000000001421, 24.50000000000000000 ) ) ;
#27593 = VERTEX_POINT ( 'NONE', #19869 ) ;
#27594 = B_SPLINE_CURVE_WITH_KNOTS ( 'NONE', 3,
 ( #24369, #3013, #26413, #26883, #17355, #5503, #28750, #29370, #12209, #19684 ),
 .UNSPECIFIED., .F., .F.,
 ( 4, 2, 2, 2, 4 ),
 ( 0.0007598054600062436074, 0.001542965791078104807, 0.002326126122149965898, 0.003109286453221827423, 0.003892446784293688514 ),
 .UNSPECIFIED. ) ;
#27595 = VECTOR ( 'NONE', #15256, 1000.000000000000000 ) ;
#27596 = CARTESIAN_POINT ( 'NONE',  ( 9.928183626064978284, -13.85837025666176281, 18.34838970509067479 ) ) ;
#27597 = CARTESIAN_POINT ( 'NONE',  ( 21.86019681245147339, 31.48592878035296749, 27.50000000000001066 ) ) ;
#27598 = ORIENTED_EDGE ( 'NONE', *, *, #27638, .T. ) ;
#27599 = ORIENTED_EDGE ( 'NONE', *, *, #16645, .T. ) ;
#27600 = CARTESIAN_POINT ( 'NONE',  ( 47.15436764833695094, 69.79802288849539593, 15.50528903784843671 ) ) ;
#27601 = DIRECTION ( 'NONE',  ( -1.000000000000000000, 0.000000000000000000, 0.000000000000000000 ) ) ;
#27602 = CARTESIAN_POINT ( 'NONE',  ( -5.869193111140222463, 19.13804834536701804, 5.657991946698900598 ) ) ;
#27603 = VERTEX_POINT ( 'NONE', #17376 ) ;
#27604 = CARTESIAN_POINT ( 'NONE',  ( -26.36764545593177544, -31.31467416275353344, 1.500000000000000000 ) ) ;
#27605 = LINE ( 'NONE', #6227, #18171 ) ;
#27606 = CARTESIAN_POINT ( 'NONE',  ( -28.78283879316666471, 7.125616703334841873, 45.34931131770228063 ) ) ;
#27607 = VERTEX_POINT ( 'NONE', #17526 ) ;
#27608 = CARTESIAN_POINT ( 'NONE',  ( -10.39781135303994830, -17.08517550777068195, 18.34869673959212122 ) ) ;
#27609 = EDGE_CURVE ( 'NONE', #25828, #7918, #15595, .T. ) ;
#27610 = CARTESIAN_POINT ( 'NONE',  ( -19.18576292979354037, 22.55620591602727387, 1.500000000000000000 ) ) ;
#27611 = CARTESIAN_POINT ( 'NONE',  ( 0.000000000000000000, -9.742773481404436396E-15, -1.500000000000001332 ) ) ;
#27612 = ORIENTED_EDGE ( 'NONE', *, *, #7849, .T. ) ;
#27613 = DIRECTION ( 'NONE',  ( 0.000000000000000000, 1.000000000000000000, 0.000000000000000000 ) ) ;
#27614 = AXIS2_PLACEMENT_3D ( 'NONE', #17076, #2583, #7573 ) ;
#27615 = EDGE_LOOP ( 'NONE', ( #17955, #7052, #392, #2996, #12950 ) ) ;
#27616 = ORIENTED_EDGE ( 'NONE', *, *, #10327, .F. ) ;
#27617 = ORIENTED_EDGE ( 'NONE', *, *, #30393, .F. ) ;
#27618 = CARTESIAN_POINT ( 'NONE',  ( 4.414161002286807189, 19.52491365267160717, 7.098451512883313441 ) ) ;
#27619 = FACE_OUTER_BOUND ( 'NONE', #13416, .T. ) ;
#27620 = CARTESIAN_POINT ( 'NONE',  ( -39.52380524536133777, -7.028748154183623420, -6.500000000000000888 ) ) ;
#27621 = VERTEX_POINT ( 'NONE', #24687 ) ;
#27622 = CARTESIAN_POINT ( 'NONE',  ( -2.338573377552017440, -39.49999999999999289, 34.80090346875804386 ) ) ;
#27623 = CARTESIAN_POINT ( 'NONE',  ( 11.05488513857797450, -16.68841100269527544, 18.34969686940296185 ) ) ;
#27624 = CARTESIAN_POINT ( 'NONE',  ( 16.87846183053956395, 2.201534687727671802, 19.22654678686458141 ) ) ;
#27625 = ORIENTED_EDGE ( 'NONE', *, *, #7435, .T. ) ;
#27626 = CARTESIAN_POINT ( 'NONE',  ( -19.80066175015358709, 2.942692509523778366, 20.25336174263950184 ) ) ;
#27627 = CARTESIAN_POINT ( 'NONE',  ( 18.30570112562006102, -8.101025642224000123, 7.652108011868850035 ) ) ;
#27628 = CARTESIAN_POINT ( 'NONE',  ( -15.97838715008243682, 12.05808207567198487, 6.447548852708279377 ) ) ;
#27629 = CARTESIAN_POINT ( 'NONE',  ( 3.613053539807236536, 16.67204840528143350, 18.44527579819791185 ) ) ;
#27630 = ORIENTED_EDGE ( 'NONE', *, *, #14536, .F. ) ;
#27631 = ORIENTED_EDGE ( 'NONE', *, *, #26972, .F. ) ;
#27632 = AXIS2_PLACEMENT_3D ( 'NONE', #29632, #17149, #10449 ) ;
#27633 = DIRECTION ( 'NONE',  ( -0.000000000000000000, 0.000000000000000000, -1.000000000000000000 ) ) ;
#27634 = DIRECTION ( 'NONE',  ( 0.000000000000000000, 0.000000000000000000, -1.000000000000000000 ) ) ;
#27635 = CARTESIAN_POINT ( 'NONE',  ( 15.21452331804151115, 12.98203751624683733, 18.47110296274025742 ) ) ;
#27636 = CARTESIAN_POINT ( 'NONE',  ( 13.00948632770315960, 10.97642674697307896, 6.782064869129509788 ) ) ;
#27637 = CARTESIAN_POINT ( 'NONE',  ( 26.44644203219471379, 9.801837641955973623, 1.500000000000000000 ) ) ;
#27638 = EDGE_CURVE ( 'NONE', #22510, #23120, #7627, .T. ) ;
#27639 = CARTESIAN_POINT ( 'NONE',  ( -22.62322288457161790, 30.83399541182840409, 27.50000000000000711 ) ) ;
#27640 = DIRECTION ( 'NONE',  ( -1.000000000000000000, 0.000000000000000000, 0.000000000000000000 ) ) ;
#27641 = ORIENTED_EDGE ( 'NONE', *, *, #22171, .F. ) ;
#27642 = CARTESIAN_POINT ( 'NONE',  ( -32.49058853941425440, -8.555876215535434426, 37.15913391332472315 ) ) ;
#27643 = CARTESIAN_POINT ( 'NONE',  ( 14.73074142449663881, 5.627958522269737252, -0.6213203435596476032 ) ) ;
#27644 = CARTESIAN_POINT ( 'NONE',  ( 40.05104235265675783, 2.353288714454550234, -6.500000000000000888 ) ) ;
#27645 = ORIENTED_EDGE ( 'NONE', *, *, #29590, .T. ) ;
#27646 = EDGE_LOOP ( 'NONE', ( #28784, #19207, #5331, #10240, #769, #4250, #5662, #11982 ) ) ;
#27647 = CARTESIAN_POINT ( 'NONE',  ( -19.69223482763159083, 3.495123391383815559, 6.518927109361852601 ) ) ;
#27648 = EDGE_CURVE ( 'NONE', #27603, #15359, #997, .T. ) ;
#27649 = CYLINDRICAL_SURFACE ( 'NONE', #5550, 20.00000000000000355 ) ;
#27650 = ORIENTED_EDGE ( 'NONE', *, *, #16635, .T. ) ;
#27651 = CARTESIAN_POINT ( 'NONE',  ( -23.16753610420780873, -35.74416778164192010, -13.16661231005593713 ) ) ;
#27652 = AXIS2_PLACEMENT_3D ( 'NONE', #16731, #25946, #18776 ) ;
#27653 = DIRECTION ( 'NONE',  ( 0.000000000000000000, 0.000000000000000000, 1.000000000000000000 ) ) ;
#27654 = CARTESIAN_POINT ( 'NONE',  ( -16.76805339484686286, -38.38162967533393299, 23.12441181139608659 ) ) ;
#27655 = FACE_OUTER_BOUND ( 'NONE', #8731, .T. ) ;
#27656 = DIRECTION ( 'NONE',  ( 0.000000000000000000, -1.132880637372608986E-16, 1.000000000000000000 ) ) ;
#27657 = EDGE_CURVE ( 'NONE', #7501, #16188, #29535, .T. ) ;
#27658 = CARTESIAN_POINT ( 'NONE',  ( 1.583371619456037438, -16.99707458536920157, 6.041646659195333058 ) ) ;
#27659 = CARTESIAN_POINT ( 'NONE',  ( -10.18506332983503704, 29.04537757311073776, 24.50000000000000000 ) ) ;
#27660 = ORIENTED_EDGE ( 'NONE', *, *, #21127, .T. ) ;
#27661 = CARTESIAN_POINT ( 'NONE',  ( 39.83602371821015709, 11.57901747687536265, -19.50000000000000355 ) ) ;
#27662 = CARTESIAN_POINT ( 'NONE',  ( 19.64177907938615064, -36.71644397333972876, 24.50000000000000000 ) ) ;
#27663 = CARTESIAN_POINT ( 'NONE',  ( -4.950721362152968652, 16.29421905978776053, 7.453286057244488561 ) ) ;
#27664 = CARTESIAN_POINT ( 'NONE',  ( 0.8038475772933806329, -10.39230484541329247, 6.144194323733775069E-17 ) ) ;
#27665 = CARTESIAN_POINT ( 'NONE',  ( 10.11202017158463917, -41.14070756921186955, -1.500000000000000000 ) ) ;
#27666 = CARTESIAN_POINT ( 'NONE',  ( -23.27838111883973227, 36.10018642694448943, -16.50000600000000262 ) ) ;
#27667 = ORIENTED_EDGE ( 'NONE', *, *, #27924, .T. ) ;
#27668 = DIRECTION ( 'NONE',  ( -1.000000000000000000, 0.000000000000000000, 0.000000000000000000 ) ) ;
#27669 = VECTOR ( 'NONE', #7542, 1000.000000000000000 ) ;
#27670 = CARTESIAN_POINT ( 'NONE',  ( 10.11202017158463917, -41.14070756921186955, -1.500000000000000000 ) ) ;
#27671 = EDGE_CURVE ( 'NONE', #6221, #22536, #19585, .T. ) ;
#27672 = CARTESIAN_POINT ( 'NONE',  ( 17.49967083908764565, -38.01026090106176980, 34.52681008576058019 ) ) ;
#27673 = EDGE_CURVE ( 'NONE', #26314, #11068, #16251, .T. ) ;
#27674 = CARTESIAN_POINT ( 'NONE',  ( 39.52380524533145945, -7.028748154382047808, -6.500000000000000888 ) ) ;
#27675 = ORIENTED_EDGE ( 'NONE', *, *, #7927, .T. ) ;
#27676 = DIRECTION ( 'NONE',  ( 1.000000000000000000, 0.000000000000000000, 0.000000000000000000 ) ) ;
#27677 = DIRECTION ( 'NONE',  ( 0.000000000000000000, 0.000000000000000000, 1.000000000000000000 ) ) ;
#27678 = CARTESIAN_POINT ( 'NONE',  ( -11.32740345151499994, -16.50481001894685917, 6.310736198168394928 ) ) ;
#27679 = ORIENTED_EDGE ( 'NONE', *, *, #28020, .F. ) ;
#27680 = EDGE_CURVE ( 'NONE', #22039, #24056, #5130, .T. ) ;
#27681 = CARTESIAN_POINT ( 'NONE',  ( -23.26222494989734813, -12.36939612486375495, 48.65398609625962933 ) ) ;
#27682=STYLED_ITEM('',(#30886),#3432);
#27683 = DIRECTION ( 'NONE',  ( 0.000000000000000000, 1.132880637372608986E-16, -1.000000000000000000 ) ) ;
#27684 = EDGE_LOOP ( 'NONE', ( #28449, #22339, #27377, #14857, #6752, #2699, #22375, #4443 ) ) ;
#27685 = EDGE_CURVE ( 'NONE', #10191, #3847, #25152, .T. ) ;
#27686 = CARTESIAN_POINT ( 'NONE',  ( -26.58938213246210580, -6.321715805855834702, 43.42684587381948091 ) ) ;
#27687 = EDGE_CURVE ( 'NONE', #5531, #23974, #26560, .T. ) ;
#27688 = CARTESIAN_POINT ( 'NONE',  ( -14.83584055149731817, -17.84153987719691514, 1.500000000000000000 ) ) ;
#27689 = EDGE_CURVE ( 'NONE', #16328, #20004, #8637, .T. ) ;
#27690 = DIRECTION ( 'NONE',  ( -0.000000000000000000, 0.000000000000000000, 1.000000000000000000 ) ) ;
#27691 = VERTEX_POINT ( 'NONE', #22817 ) ;
#27692 = CARTESIAN_POINT ( 'NONE',  ( 11.66432357650553087, 12.47412091822526392, 19.21769074125273136 ) ) ;
#27694 = ADVANCED_FACE ( 'NONE', ( #29999 ), #16108, .T. ) ;
#27693 = VECTOR ( 'NONE', #19210, 1000.000000000000000 ) ;
#27695 = FACE_OUTER_BOUND ( 'NONE', #28229, .T. ) ;
#27696 = DIRECTION ( 'NONE',  ( 0.000000000000000000, 0.000000000000000000, 1.000000000000000000 ) ) ;
#27697 = DIRECTION ( 'NONE',  ( 0.000000000000000000, 0.000000000000000000, -1.000000000000000000 ) ) ;
#27698 = CIRCLE ( 'NONE', #1801, 9.482273699623480212 ) ;
#27699 = CARTESIAN_POINT ( 'NONE',  ( -15.37836256580256311, -7.321964739906460018, 20.22273502201483453 ) ) ;
#27700 = DIRECTION ( 'NONE',  ( 1.000000000000000000, 0.000000000000000000, 0.000000000000000000 ) ) ;
#27701 = CARTESIAN_POINT ( 'NONE',  ( 7.500000000000000000, -10.39230484541329247, 8.776157072412030708E-17 ) ) ;
#27702 = DIRECTION ( 'NONE',  ( 0.2817325568414296710, 0.9594929736144973687, 0.000000000000000000 ) ) ;
#27703 = CARTESIAN_POINT ( 'NONE',  ( -37.99999999999999289, 70.00000000000000000, -81.50000000000000000 ) ) ;
#27704 = CARTESIAN_POINT ( 'NONE',  ( -9.353104432054360373, -14.22246372585392038, 19.66962785902261857 ) ) ;
#27705 = AXIS2_PLACEMENT_3D ( 'NONE', #11015, #22399, #20369 ) ;
#27706 = ORIENTED_EDGE ( 'NONE', *, *, #17908, .T. ) ;
#27707 = ORIENTED_EDGE ( 'NONE', *, *, #3226, .F. ) ;
#27708 = CARTESIAN_POINT ( 'NONE',  ( -1.000000000000008438, 13.00000000000001421, 24.50000000000000000 ) ) ;
#27709 = CARTESIAN_POINT ( 'NONE',  ( -4.340342926365017284, -8.430595340551244377, 1.500000000000001332 ) ) ;
#27710 = EDGE_CURVE ( 'NONE', #21029, #19394, #11435, .T. ) ;
#27711 = LINE ( 'NONE', #9136, #30816 ) ;
#27712 = EDGE_CURVE ( 'NONE', #24914, #6039, #5341, .T. ) ;
#27713 = ORIENTED_EDGE ( 'NONE', *, *, #17599, .T. ) ;
#27714 = LINE ( 'NONE', #20220, #26342 ) ;
#27715 = EDGE_CURVE ( 'NONE', #23890, #19511, #1618, .T. ) ;
#27716 = LINE ( 'NONE', #11183, #4216 ) ;
#27717 = AXIS2_PLACEMENT_3D ( 'NONE', #27935, #1584, #13734 ) ;
#27718 = ORIENTED_EDGE ( 'NONE', *, *, #12771, .T. ) ;
#27719 = ORIENTED_EDGE ( 'NONE', *, *, #22530, .F. ) ;
#27720 = CARTESIAN_POINT ( 'NONE',  ( -11.19063532726251964, -16.57644352599301030, 18.72886616302735519 ) ) ;
#27721 = CIRCLE ( 'NONE', #24718, 1.000000000000000888 ) ;
#27722 = CARTESIAN_POINT ( 'NONE',  ( -31.46019086465472725, -15.19107625323260180, 35.82171084658602211 ) ) ;
#27723 = AXIS2_PLACEMENT_3D ( 'NONE', #12925, #29292, #10249 ) ;
#27724 = DIRECTION ( 'NONE',  ( -5.782411586589351722E-15, 1.000000000000000000, 0.000000000000000000 ) ) ;
#27725 = CARTESIAN_POINT ( 'NONE',  ( 5.060094141397912360, 42.14075867279367316, 28.87075318537528190 ) ) ;
#27726 = ORIENTED_EDGE ( 'NONE', *, *, #13464, .F. ) ;
#27727 = CARTESIAN_POINT ( 'NONE',  ( -8.134323311075783991, -1.438332125858144295, -3.621320343559650379 ) ) ;
#27728 = VERTEX_POINT ( 'NONE', #29858 ) ;
#27729 = EDGE_CURVE ( 'NONE', #24441, #20436, #24265, .T. ) ;
#27730 = CARTESIAN_POINT ( 'NONE',  ( -26.12047388987420149, 6.311255530320346807, 43.88527982295141783 ) ) ;
#27731 = CARTESIAN_POINT ( 'NONE',  ( -15.17592917621934490, 13.02713289664471397, 5.676722608126686609 ) ) ;
#27732 = AXIS2_PLACEMENT_3D ( 'NONE', #14457, #19444, #21624 ) ;
#27733 = EDGE_LOOP ( 'NONE', ( #16310, #13987, #28333, #28642 ) ) ;
#27734 = MECHANICAL_DESIGN_GEOMETRIC_PRESENTATION_REPRESENTATION (  '', ( #24733 ), #14757 ) ;
#27735 = CARTESIAN_POINT ( 'NONE',  ( 16.78403870106610185, 2.933703390186591875, 20.32222155561919053 ) ) ;
#27736 = CYLINDRICAL_SURFACE ( 'NONE', #6745, 28.20443790117971261 ) ;
#27737 = CARTESIAN_POINT ( 'NONE',  ( 36.04561543331149664, -16.23932455912026640, 31.42798667167778248 ) ) ;
#27738 = DIRECTION ( 'NONE',  ( -0.000000000000000000, -0.000000000000000000, 1.000000000000000000 ) ) ;
#27739 = VECTOR ( 'NONE', #6933, 1000.000000000000000 ) ;
#27740 = CARTESIAN_POINT ( 'NONE',  ( -17.84153987719600920, 14.83584055149731284, 1.500000000000000000 ) ) ;
#27741 = FACE_OUTER_BOUND ( 'NONE', #20156, .T. ) ;
#27742 = CARTESIAN_POINT ( 'NONE',  ( -9.369089179312702242, -14.21146650728334038, 6.910395520694542881 ) ) ;
#27743 = FACE_OUTER_BOUND ( 'NONE', #7965, .T. ) ;
#27744 = ORIENTED_EDGE ( 'NONE', *, *, #24444, .F. ) ;
#27745 = EDGE_CURVE ( 'NONE', #11023, #24333, #26775, .T. ) ;
#27746 = VECTOR ( 'NONE', #13516, 1000.000000000000000 ) ;
#27747 = EDGE_CURVE ( 'NONE', #2953, #27284, #30092, .T. ) ;
#27748 = CARTESIAN_POINT ( 'NONE',  ( 11.64616783614241058, -16.28139325077859922, 18.56793045041961321 ) ) ;
#27749 = CIRCLE ( 'NONE', #11312, 0.7500000000000006661 ) ;
#27750 = CARTESIAN_POINT ( 'NONE',  ( 23.69412710310940540, -29.84645176427128987, 27.50000000000000355 ) ) ;
#27751 = VERTEX_POINT ( 'NONE', #11127 ) ;
#27752 = ORIENTED_EDGE ( 'NONE', *, *, #5162, .T. ) ;
#27753 = FACE_OUTER_BOUND ( 'NONE', #30175, .T. ) ;
#27754 = CARTESIAN_POINT ( 'NONE',  ( -15.43151021478632323, 12.72345061513106579, 5.652912763329820400 ) ) ;
#27755 = B_SPLINE_CURVE_WITH_KNOTS ( 'NONE', 3,
 ( #1828, #6971, #20846, #3867 ),
 .UNSPECIFIED., .F., .F.,
 ( 4, 4 ),
 ( 3.022186913382060468E-07, 0.007932103869840216592 ),
 .UNSPECIFIED. ) ;
#27756 = CARTESIAN_POINT ( 'NONE',  ( 32.60829997825920401, -13.18983524832148113, 35.60092001944722995 ) ) ;
#27757 = ORIENTED_EDGE ( 'NONE', *, *, #17566, .F. ) ;
#27758 = DIRECTION ( 'NONE',  ( -0.000000000000000000, -0.000000000000000000, -1.000000000000000000 ) ) ;
#27759 = CIRCLE ( 'NONE', #9304, 9.482273699623480212 ) ;
#27760 = CARTESIAN_POINT ( 'NONE',  ( -12.74661400764364139, 11.28197093996912415, 6.973843882838226094 ) ) ;
#27761 = CARTESIAN_POINT ( 'NONE',  ( 0.8750451464062524165, 9.041888939645138734, 21.50000000000000000 ) ) ;
#27762 = ORIENTED_EDGE ( 'NONE', *, *, #16447, .F. ) ;
#27763 = CYLINDRICAL_SURFACE ( 'NONE', #5291, 10.00000000000000178 ) ;
#27764 = AXIS2_PLACEMENT_3D ( 'NONE', #1218, #5585, #20225 ) ;
#27765 = CYLINDRICAL_SURFACE ( 'NONE', #6514, 1.447898107987198646 ) ;
#27766 = ORIENTED_EDGE ( 'NONE', *, *, #12817, .F. ) ;
#27767 = CIRCLE ( 'NONE', #15321, 5.035999999999999588 ) ;
#27768 = ORIENTED_EDGE ( 'NONE', *, *, #8631, .T. ) ;
#27769 = DIRECTION ( 'NONE',  ( 0.000000000000000000, 0.000000000000000000, 1.000000000000000000 ) ) ;
#27770 = AXIS2_PLACEMENT_3D ( 'NONE', #20302, #29827, #17972 ) ;
#27771 = ORIENTED_EDGE ( 'NONE', *, *, #3679, .T. ) ;
#27772 = EDGE_LOOP ( 'NONE', ( #17732, #18005, #3736, #29826 ) ) ;
#27773 = CARTESIAN_POINT ( 'NONE',  ( 3.518760595952259873, 16.69517982287621649, 5.810767894563978686 ) ) ;
#27774 = CARTESIAN_POINT ( 'NONE',  ( 7.869584159753955532, 10.39565510934977333, 24.50000000000000000 ) ) ;
#27775 = DIRECTION ( 'NONE',  ( -0.000000000000000000, -0.000000000000000000, 1.000000000000000000 ) ) ;
#27776 = CIRCLE ( 'NONE', #20313, 0.7500000000000006661 ) ;
#27777 = ORIENTED_EDGE ( 'NONE', *, *, #16839, .T. ) ;
#27778 = B_SPLINE_CURVE_WITH_KNOTS ( 'NONE', 3,
 ( #1754, #16106, #1907, #8634, #25626, #22815, #1466, #21069, #11270, #28114, #27965, #18145, #17998, #11433, #27508, #25150, #20920, #30296 ),
 .UNSPECIFIED., .F., .F.,
 ( 4, 2, 2, 2, 2, 2, 2, 2, 4 ),
 ( 0.000000000000000000, 0.1250000000000000000, 0.2500000000000000000, 0.3750000000000000000, 0.5000000000000000000, 0.6250000000000000000, 0.7500000000000000000, 0.8750000000000000000, 1.000000000000000000 ),
 .UNSPECIFIED. ) ;
#27779 = AXIS2_PLACEMENT_3D ( 'NONE', #7051, #14535, #4557 ) ;
#27780 = CARTESIAN_POINT ( 'NONE',  ( 9.014152831625308337, -14.43863835250231098, 19.22654678686458141 ) ) ;
#27781 = PLANE ( 'NONE',  #8390 ) ;
#27782 = VERTEX_POINT ( 'NONE', #8498 ) ;
#27783 = AXIS2_PLACEMENT_3D ( 'NONE', #5318, #5014, #29498 ) ;
#27784 = CYLINDRICAL_SURFACE ( 'NONE', #19713, 6.000000000000005329 ) ;
#27785 = CARTESIAN_POINT ( 'NONE',  ( 15.45343642833786646, -7.142940632752242891, 6.111214848085761986 ) ) ;
#27786 = ADVANCED_FACE ( 'NONE', ( #18001 ), #30144, .F. ) ;
#27787 = CARTESIAN_POINT ( 'NONE',  ( -13.95900029477594906, 9.834024558217738132, 6.233981582756856987 ) ) ;
#27788 = CARTESIAN_POINT ( 'NONE',  ( 4.339153914952778912, 19.54170514621187138, 19.58863275299554019 ) ) ;
#27789 = ORIENTED_EDGE ( 'NONE', *, *, #19068, .F. ) ;
#27790 = EDGE_LOOP ( 'NONE', ( #8855, #2396, #1160, #6654 ) ) ;
#27791 = VECTOR ( 'NONE', #20192, 999.9999999999998863 ) ;
#27792 = EDGE_CURVE ( 'NONE', #4577, #25866, #25479, .T. ) ;
#27793 = CARTESIAN_POINT ( 'NONE',  ( 12.35522425158189108, 11.74279415389956505, 5.652196082368482699 ) ) ;
#27794 = CARTESIAN_POINT ( 'NONE',  ( 3.914781618004695041, 8.197313248159959542, 21.50000000000000000 ) ) ;
#27795 = CARTESIAN_POINT ( 'NONE',  ( 18.25048847709279443, -37.60031054104898374, 23.76984935710975577 ) ) ;
#27796 = CARTESIAN_POINT ( 'NONE',  ( -5.450136891332535427, 19.26184010647176237, 20.19668224736330941 ) ) ;
#27797 = DIRECTION ( 'NONE',  ( 0.000000000000000000, 0.000000000000000000, 1.000000000000000000 ) ) ;
#27798 = VECTOR ( 'NONE', #8973, 1000.000000000000000 ) ;
#27799 = DIRECTION ( 'NONE',  ( 1.000000000000000000, 0.000000000000000000, 0.000000000000000000 ) ) ;
#27800 = CARTESIAN_POINT ( 'NONE',  ( 23.07500649350761179, -11.56036165373734725, 49.19141369487476112 ) ) ;
#27801 = AXIS2_PLACEMENT_3D ( 'NONE', #3301, #22014, #29513 ) ;
#27802 = ORIENTED_EDGE ( 'NONE', *, *, #5575, .T. ) ;
#27803 = VECTOR ( 'NONE', #16642, 1000.000000000000000 ) ;
#27804 = CARTESIAN_POINT ( 'NONE',  ( 0.8643805006890358245, -19.98168094404550033, 5.779535427900761135 ) ) ;
#27805 = CARTESIAN_POINT ( 'NONE',  ( 33.01877980957529957, 12.12572312222181026, 39.84356070656652804 ) ) ;
#27806 = DIRECTION ( 'NONE',  ( 0.000000000000000000, 0.000000000000000000, 1.000000000000000000 ) ) ;
#27807 = ORIENTED_EDGE ( 'NONE', *, *, #27489, .F. ) ;
#27808 = CARTESIAN_POINT ( 'NONE',  ( 4.082218581380954170, 16.54825969530612895, 18.34777357837151612 ) ) ;
#27809 = VERTEX_POINT ( 'NONE', #6129 ) ;
#27810 = CARTESIAN_POINT ( 'NONE',  ( -6.437683520590121056, 6.962021646281599807, 1.500000000000001332 ) ) ;
#27811 = VECTOR ( 'NONE', #4310, 1000.000000000000000 ) ;
#27812 = DIRECTION ( 'NONE',  ( 0.000000000000000000, 0.000000000000000000, 1.000000000000000000 ) ) ;
#27813 = EDGE_LOOP ( 'NONE', ( #19553, #1876, #23935, #6585 ) ) ;
#27814 = CARTESIAN_POINT ( 'NONE',  ( -23.00100564344168674, -35.20929534199333233, -8.166629675772911767 ) ) ;
#27815 = AXIS2_PLACEMENT_3D ( 'NONE', #13917, #13315, #25768 ) ;
#27816 = CARTESIAN_POINT ( 'NONE',  ( 6.652725104973315595, 49.55738370017981964, -68.45305803092846020 ) ) ;
#27817 = CARTESIAN_POINT ( 'NONE',  ( 3.685570353517261477, -16.10136545388692397, -0.6213203435596476032 ) ) ;
#27818 = FACE_OUTER_BOUND ( 'NONE', #29678, .T. ) ;
#27819 = DIRECTION ( 'NONE',  ( 0.000000000000000000, 0.000000000000000000, -1.000000000000000000 ) ) ;
#27820 = B_SPLINE_CURVE_WITH_KNOTS ( 'NONE', 3,
 ( #18489, #20948, #22680, #6170 ),
 .UNSPECIFIED., .F., .F.,
 ( 4, 4 ),
 ( 2.143643656977390230E-07, 0.003421830178490235016 ),
 .UNSPECIFIED. ) ;
#27821 = CARTESIAN_POINT ( 'NONE',  ( 0.000000000000000000, 13.00000000000001421, 1.500000000000001332 ) ) ;
#27822 = CARTESIAN_POINT ( 'NONE',  ( 1.315538599303260447, -19.97434797600632805, 6.341840715582230281 ) ) ;
#27823 = ORIENTED_EDGE ( 'NONE', *, *, #23249, .F. ) ;
#27824 = AXIS2_PLACEMENT_3D ( 'NONE', #23451, #13956, #1951 ) ;
#27825 = AXIS2_PLACEMENT_3D ( 'NONE', #12005, #4818, #30703 ) ;
#27826 = DIRECTION ( 'NONE',  ( -0.000000000000000000, -0.000000000000000000, 1.000000000000000000 ) ) ;
#27827 = DIRECTION ( 'NONE',  ( 1.000000000000000000, 0.000000000000000000, 0.000000000000000000 ) ) ;
#27828 = CYLINDRICAL_SURFACE ( 'NONE', #19032, 1.447898107987198646 ) ;
#27829 = CARTESIAN_POINT ( 'NONE',  ( -15.16307466679258553, -7.786257835066843214, 18.34798005862662507 ) ) ;
#27830 = CARTESIAN_POINT ( 'NONE',  ( 0.1469846612282506015, 8.891930899535427812, 2.598723904613014835 ) ) ;
#27831 = LINE ( 'NONE', #3808, #10118 ) ;
#27832 = CIRCLE ( 'NONE', #14366, 1.000000000000004441 ) ;
#27833 = ORIENTED_EDGE ( 'NONE', *, *, #6552, .F. ) ;
#27834 = CARTESIAN_POINT ( 'NONE',  ( -0.6570508600772855257, -19.98920419113419200, 19.21471108562414898 ) ) ;
#27835 = DIRECTION ( 'NONE',  ( -1.000000000000000000, 0.000000000000000000, 0.000000000000000000 ) ) ;
#27836 = CARTESIAN_POINT ( 'NONE',  ( 38.04520357587708190, -9.701815779983750332, 31.93699797870259260 ) ) ;
#27837 = CARTESIAN_POINT ( 'NONE',  ( 37.99999999999999289, 70.00000000000000000, -75.50000000000001421 ) ) ;
#27838 = ORIENTED_EDGE ( 'NONE', *, *, #2199, .T. ) ;
#27839 = LINE ( 'NONE', #1779, #27577 ) ;
#27840 = CARTESIAN_POINT ( 'NONE',  ( -32.74775157610760346, -27.21557300919352329, -19.50000000000000355 ) ) ;
#27841 = CARTESIAN_POINT ( 'NONE',  ( -14.58213539500865785, 7.758783772730382111, -0.6213203435596476032 ) ) ;
#27842 = EDGE_CURVE ( 'NONE', #10610, #17425, #19152, .T. ) ;
#27843 = EDGE_LOOP ( 'NONE', ( #29845, #3577, #15374, #24563 ) ) ;
#27844 = VECTOR ( 'NONE', #12555, 1000.000000000000000 ) ;
#27845 = AXIS2_PLACEMENT_3D ( 'NONE', #13056, #3840, #5713 ) ;
#27846 = CIRCLE ( 'NONE', #24331, 2.061368542273053883 ) ;
#27847 = DIRECTION ( 'NONE',  ( 1.000000000000000000, 0.000000000000000000, 0.000000000000000000 ) ) ;
#27848 = VERTEX_POINT ( 'NONE', #8946 ) ;
#27849 = DIRECTION ( 'NONE',  ( -1.000000000000000000, 0.000000000000000000, 0.000000000000000000 ) ) ;
#27850 = CARTESIAN_POINT ( 'NONE',  ( 37.99999999999999289, 65.00000000000000000, 15.49999999999998934 ) ) ;
#27851 = CARTESIAN_POINT ( 'NONE',  ( -14.36006998371493637, -17.26937953831884442, -1.500000000000000000 ) ) ;
#27852 = VECTOR ( 'NONE', #10298, 1000.000000000000000 ) ;
#27853 = ORIENTED_EDGE ( 'NONE', *, *, #21958, .F. ) ;
#27854 = CARTESIAN_POINT ( 'NONE',  ( -7.730328572437709767, 4.608906612435681005, 1.500000000000001332 ) ) ;
#27855 = CARTESIAN_POINT ( 'NONE',  ( 16.58239702337846566, 4.066005520140572038, 7.158811349119580392 ) ) ;
#27856 = EDGE_CURVE ( 'NONE', #24053, #16566, #30298, .T. ) ;
#27857 = DIRECTION ( 'NONE',  ( -1.000000000000000000, -0.000000000000000000, -0.000000000000000000 ) ) ;
#27858 = EDGE_CURVE ( 'NONE', #11886, #16236, #1367, .T. ) ;
#27859 = CARTESIAN_POINT ( 'NONE',  ( 7.730328572437743517, -4.608906612435629491, 21.50000000000000000 ) ) ;
#27860 = CARTESIAN_POINT ( 'NONE',  ( 10.18506332983505303, 29.04537757311072710, 24.50000000000000000 ) ) ;
#27861 = DIRECTION ( 'NONE',  ( -1.000000000000000000, 0.000000000000000000, 0.000000000000000000 ) ) ;
#27862 = DIRECTION ( 'NONE',  ( -0.000000000000000000, -0.000000000000000000, -1.000000000000000000 ) ) ;
#27863 = EDGE_CURVE ( 'NONE', #14718, #3254, #4243, .T. ) ;
#27864 = CARTESIAN_POINT ( 'NONE',  ( -18.37726663805288396, -7.892083924814675910, 19.96302680909624883 ) ) ;
#27865 = EDGE_CURVE ( 'NONE', #357, #3146, #30593, .T. ) ;
#27866 = CARTESIAN_POINT ( 'NONE',  ( -18.24831633358133942, -8.229495485092105156, 20.25336174263950184 ) ) ;
#27867 = CARTESIAN_POINT ( 'NONE',  ( -8.975220329042040035, -14.47597657772637447, 18.47056384035244037 ) ) ;
#27868 = AXIS2_PLACEMENT_3D ( 'NONE', #6180, #8214, #15532 ) ;
#27869 = AXIS2_PLACEMENT_3D ( 'NONE', #20152, #29669, #22949 ) ;
#27870 = VERTEX_POINT ( 'NONE', #23882 ) ;
#27871 = CARTESIAN_POINT ( 'NONE',  ( 24.44496207165490631, -7.595930209050163029, 49.40206402021031096 ) ) ;
#27872 = CARTESIAN_POINT ( 'NONE',  ( 40.89187623478217404, -5.790488632116400858, -19.50000000000000355 ) ) ;
#27873 = EDGE_CURVE ( 'NONE', #4107, #18044, #23718, .T. ) ;
#27874 = DIRECTION ( 'NONE',  ( -0.000000000000000000, -0.000000000000000000, -1.000000000000000000 ) ) ;
#27875 = ORIENTED_EDGE ( 'NONE', *, *, #12819, .T. ) ;
#27876 = DIRECTION ( 'NONE',  ( 1.000000000000000000, 0.000000000000000000, 0.000000000000000000 ) ) ;
#27877 = AXIS2_PLACEMENT_3D ( 'NONE', #25296, #20748, #13746 ) ;
#27878 = CARTESIAN_POINT ( 'NONE',  ( -4.163336342344337027E-14, 1.387778780781445676E-14, 24.50000000000000000 ) ) ;
#27879 = EDGE_CURVE ( 'NONE', #26463, #12314, #13919, .T. ) ;
#27880 = DIRECTION ( 'NONE',  ( 1.000000000000000000, 0.000000000000000000, 0.000000000000000000 ) ) ;
#27881 = EDGE_CURVE ( 'NONE', #2587, #7648, #27776, .T. ) ;
#27882 = ORIENTED_EDGE ( 'NONE', *, *, #6309, .T. ) ;
#27883 = CARTESIAN_POINT ( 'NONE',  ( -19.71887672257058810, 3.447422735172819497, 6.310736198168394928 ) ) ;
#27884 = DIRECTION ( 'NONE',  ( 1.000000000000000000, 0.000000000000000000, 0.000000000000000000 ) ) ;
#27885 = DIRECTION ( 'NONE',  ( 0.9898214418809327952, -0.1423148382732850048, 0.000000000000000000 ) ) ;
#27886 = ORIENTED_EDGE ( 'NONE', *, *, #12257, .T. ) ;
#27887 = CARTESIAN_POINT ( 'NONE',  ( -42.49999999999998579, 50.00000000000000000, 12.49999999999999112 ) ) ;
#27888 = VERTEX_POINT ( 'NONE', #2210 ) ;
#27889 = CARTESIAN_POINT ( 'NONE',  ( 0.7788148816922458861, -17.02744011591804707, 20.34789198813115263 ) ) ;
#27890 = DIRECTION ( 'NONE',  ( 0.000000000000000000, -1.000000000000000000, 0.000000000000000000 ) ) ;
#27891 = VERTEX_POINT ( 'NONE', #9853 ) ;
#27892 = CARTESIAN_POINT ( 'NONE',  ( -39.87808514440047247, 7.028748154183623420, -14.83333104106490197 ) ) ;
#27893 = EDGE_CURVE ( 'NONE', #9405, #9920, #6893, .T. ) ;
#27894 = FILL_AREA_STYLE_COLOUR ( '', #21747 ) ;
#27895 = EDGE_CURVE ( 'NONE', #4581, #16359, #17297, .T. ) ;
#27896 = CARTESIAN_POINT ( 'NONE',  ( 46.99999999999998579, 87.00000000000001421, 22.49999999999999289 ) ) ;
#27897=STYLED_ITEM('',(#30907),#23377);
#27898 = EDGE_CURVE ( 'NONE', #13626, #2292, #9392, .T. ) ;
#27899 = CARTESIAN_POINT ( 'NONE',  ( 24.44496207165490631, -7.595930209050163029, 49.40206402021031096 ) ) ;
#27900 = CARTESIAN_POINT ( 'NONE',  ( 0.1262659238204208167, 8.999114229549594057, 21.50000000000000000 ) ) ;
#27901 = CARTESIAN_POINT ( 'NONE',  ( -8.661893131359024167, -14.67663382386235149, 7.652108011868851811 ) ) ;
#27902 = CARTESIAN_POINT ( 'NONE',  ( -7.856594496258223259, -4.390207617113929039, 1.500000000000001332 ) ) ;
#27903 = ORIENTED_EDGE ( 'NONE', *, *, #30413, .T. ) ;
#27904 = EDGE_CURVE ( 'NONE', #4157, #5507, #23418, .T. ) ;
#27905 = CARTESIAN_POINT ( 'NONE',  ( -30.54665521170317888, 26.42654420156934947, 17.37260941130015013 ) ) ;
#27906 = CARTESIAN_POINT ( 'NONE',  ( 4.677126025380961671, -39.24912351428227453, 34.80090346875809360 ) ) ;
#27907 = ORIENTED_EDGE ( 'NONE', *, *, #6134, .F. ) ;
#27908 = ORIENTED_EDGE ( 'NONE', *, *, #21350, .T. ) ;
#27909 = DIRECTION ( 'NONE',  ( 1.000000000000000000, 0.000000000000000000, 0.000000000000000000 ) ) ;
#27910 = EDGE_CURVE ( 'NONE', #19006, #10874, #7366, .T. ) ;
#27911 = CARTESIAN_POINT ( 'NONE',  ( -4.594331223478845594, 16.38995132059639914, 6.420335371522007506 ) ) ;
#27912 = ORIENTED_EDGE ( 'NONE', *, *, #19011, .F. ) ;
#27913 = DIRECTION ( 'NONE',  ( -0.000000000000000000, -1.000000000000000000, -0.000000000000000000 ) ) ;
#27914 = DIRECTION ( 'NONE',  ( -0.000000000000000000, -0.000000000000000000, 1.000000000000000000 ) ) ;
#27915 = VERTEX_POINT ( 'NONE', #18751 ) ;
#27916 = PLANE ( 'NONE',  #7301 ) ;
#27917 = AXIS2_PLACEMENT_3D ( 'NONE', #9712, #17194, #29056 ) ;
#27918 = CARTESIAN_POINT ( 'NONE',  ( 0.000000000000000000, 9.738409107444585544, 27.94260272410217638 ) ) ;
#27919 = ORIENTED_EDGE ( 'NONE', *, *, #24594, .T. ) ;
#27920 = DIRECTION ( 'NONE',  ( 0.000000000000000000, 0.000000000000000000, 1.000000000000000000 ) ) ;
#27921 = ORIENTED_EDGE ( 'NONE', *, *, #21757, .T. ) ;
#27922 = ADVANCED_FACE ( 'NONE', ( #21688 ), #7521, .F. ) ;
#27923 = CYLINDRICAL_SURFACE ( 'NONE', #2965, 0.7500000000000006661 ) ;
#27924 = EDGE_CURVE ( 'NONE', #20068, #3010, #13329, .T. ) ;
#27925 = ORIENTED_EDGE ( 'NONE', *, *, #16409, .T. ) ;
#27926 = AXIS2_PLACEMENT_3D ( 'NONE', #29873, #6298, #27525 ) ;
#27927 = VERTEX_POINT ( 'NONE', #25922 ) ;
#27928 = DIRECTION ( 'NONE',  ( 0.000000000000000000, 1.000000000000000000, -0.000000000000000000 ) ) ;
#27929 = CARTESIAN_POINT ( 'NONE',  ( 0.6479391101829744537, -17.02974303764626640, 20.34789198813115974 ) ) ;
#27930 = ORIENTED_EDGE ( 'NONE', *, *, #6331, .F. ) ;
#27931 = DIRECTION ( 'NONE',  ( -0.000000000000000000, -0.000000000000000000, 1.000000000000000000 ) ) ;
#27932 = CARTESIAN_POINT ( 'NONE',  ( 16.79425489945616334, 2.861376016183142745, 20.29090034784956131 ) ) ;
#27933 = ORIENTED_EDGE ( 'NONE', *, *, #10325, .T. ) ;
#27934 = CARTESIAN_POINT ( 'NONE',  ( -16.81771903218351483, 2.627522578025004663, 19.56050940960062690 ) ) ;
#27935 = CARTESIAN_POINT ( 'NONE',  ( -5.687793815610304726, 6.974883619896852238, -1.500000000000000888 ) ) ;
#27936 = CIRCLE ( 'NONE', #18479, 9.000000000000000000 ) ;
#27937 = CARTESIAN_POINT ( 'NONE',  ( -15.92677741484699006, 12.12620433921148688, 7.098451512883313441 ) ) ;
#27938 = CARTESIAN_POINT ( 'NONE',  ( 5.151948548241253256, 19.34356600583523544, 18.35718225375110180 ) ) ;
#27939 = VERTEX_POINT ( 'NONE', #19053 ) ;
#27940 = ORIENTED_EDGE ( 'NONE', *, *, #13051, .T. ) ;
#27941 = DIRECTION ( 'NONE',  ( 0.000000000000000000, 0.000000000000000000, 1.000000000000000000 ) ) ;
#27942 = DIRECTION ( 'NONE',  ( 1.000000000000000000, 0.000000000000000000, 0.000000000000000000 ) ) ;
#27943 = CARTESIAN_POINT ( 'NONE',  ( 15.53731853391909112, 12.59332096006129831, 19.47728749465736442 ) ) ;
#27944 = CARTESIAN_POINT ( 'NONE',  ( 13.01334791338954489, 10.97165762312714143, 6.519181285484535238 ) ) ;
#27945 = FILL_AREA_STYLE_COLOUR ( '', #7796 ) ;
#27946 = CARTESIAN_POINT ( 'NONE',  ( 7.869584159753955532, 10.39565510934977333, 1.500000000000001332 ) ) ;
#27947 = CARTESIAN_POINT ( 'NONE',  ( -8.552541667382493884, 38.37438965712765082, 27.50000000000000355 ) ) ;
#27948 = CONTEXT_DEPENDENT_SHAPE_REPRESENTATION ( #1660, #19135 ) ;
#27949 = CARTESIAN_POINT ( 'NONE',  ( -1.195154792889456363, -9.406652940105981742, 21.50000000000000000 ) ) ;
#27950 = ORIENTED_EDGE ( 'NONE', *, *, #10165, .T. ) ;
#27951 = CARTESIAN_POINT ( 'NONE',  ( -19.96096598928918908, 1.505335854884786828, 6.447548852708279377 ) ) ;
#27952 = CARTESIAN_POINT ( 'NONE',  ( 14.87898868866547097, 13.36471831362575102, 18.34798005863227388 ) ) ;
#27953 = CARTESIAN_POINT ( 'NONE',  ( 11.11118051879628155, -16.62953239715190534, 18.34798005863227388 ) ) ;
#27954 = ORIENTED_EDGE ( 'NONE', *, *, #8074, .F. ) ;
#27955 = DIRECTION ( 'NONE',  ( 0.000000000000000000, 1.132880637372608986E-16, -1.000000000000000000 ) ) ;
#27956 = VERTEX_POINT ( 'NONE', #4551 ) ;
#27957 = LINE ( 'NONE', #16, #23875 ) ;
#27958 = CIRCLE ( 'NONE', #1624, 0.7500000000000006661 ) ;
#27959 = UNCERTAINTY_MEASURE_WITH_UNIT (LENGTH_MEASURE( 1.000000000000000082E-05 ), #4005, 'distance_accuracy_value', 'NONE');
#27960 = CARTESIAN_POINT ( 'NONE',  ( -19.94482228061659512, 1.484609193405911132, 19.21940439362674624 ) ) ;
#27961 = EDGE_LOOP ( 'NONE', ( #7929, #25495, #27212, #25023 ) ) ;
#27962 = CARTESIAN_POINT ( 'NONE',  ( 127.5000000000000000, 0.000000000000000000, 0.000000000000000000 ) ) ;
#27963 = CARTESIAN_POINT ( 'NONE',  ( 49.99999999999998579, 70.00000000000000000, 52.49999999999999289 ) ) ;
#27964 = CARTESIAN_POINT ( 'NONE',  ( -9.627708240023329367, -41.19544438224844640, 20.79995618394494272 ) ) ;
#27965 = CARTESIAN_POINT ( 'NONE',  ( -21.14898501148481103, -24.45236287589831292, -16.50001200000000168 ) ) ;
#27966 = DIRECTION ( 'NONE',  ( -1.000000000000000000, -0.000000000000000000, -0.000000000000000000 ) ) ;
#27967 = CARTESIAN_POINT ( 'NONE',  ( 6.899999999999999467, -10.39230484541329247, 8.776157072412030708E-17 ) ) ;
#27968 = CYLINDRICAL_SURFACE ( 'NONE', #10158, 2.898871837527149165 ) ;
#27969 = ORIENTED_EDGE ( 'NONE', *, *, #16569, .F. ) ;
#27970 = DIRECTION ( 'NONE',  ( 1.000000000000000000, 0.000000000000000000, 0.000000000000000000 ) ) ;
#27971 = CARTESIAN_POINT ( 'NONE',  ( 12.86767874445214055, -1.850092897552706894, 1.500000000000001332 ) ) ;
#27972 = CARTESIAN_POINT ( 'NONE',  ( 14.41708049311143469, -17.22181377297010130, -1.500000000000000000 ) ) ;
#27973 = CARTESIAN_POINT ( 'NONE',  ( 0.3563104543936492230, -9.539178283403872527, 1.477658550686874017 ) ) ;
#27974 = CARTESIAN_POINT ( 'NONE',  ( 39.00000000000000000, -5.563236990218592304, -1.500000000000000000 ) ) ;
#27975 = VECTOR ( 'NONE', #8680, 1000.000000000000000 ) ;
#27976 = DIRECTION ( 'NONE',  ( 0.000000000000000000, -0.000000000000000000, 1.000000000000000000 ) ) ;
#27977 = ORIENTED_EDGE ( 'NONE', *, *, #13249, .T. ) ;
#27978 = FACE_BOUND ( 'NONE', #13, .T. ) ;
#27979 = CARTESIAN_POINT ( 'NONE',  ( -5.278755796068720585, -7.392982946727063798, 13.22130136205108819 ) ) ;
#27980 = CARTESIAN_POINT ( 'NONE',  ( 14.45970719238747115, -39.47880481153868004, 34.54750567515515769 ) ) ;
#27981 = FACE_BOUND ( 'NONE', #7380, .T. ) ;
#27982 = EDGE_LOOP ( 'NONE', ( #473, #11456, #19352, #27675 ) ) ;
#27983 = CARTESIAN_POINT ( 'NONE',  ( -13.97970881677065158, 9.806700574782176716, 6.329955581934036069 ) ) ;
#27984 = CARTESIAN_POINT ( 'NONE',  ( -2.931009552726339784, -14.22630671667915969, 1.500000000000000000 ) ) ;
#27985 = DIRECTION ( 'NONE',  ( 0.000000000000000000, 0.000000000000000000, 1.000000000000000000 ) ) ;
#27986 = VERTEX_POINT ( 'NONE', #7044 ) ;
#27987 = VECTOR ( 'NONE', #5500, 1000.000000000000000 ) ;
#27988 = CARTESIAN_POINT ( 'NONE',  ( -8.318988986562537491, -36.57037096148668098, 37.50000000002251710 ) ) ;
#27989 = ORIENTED_EDGE ( 'NONE', *, *, #1382, .T. ) ;
#27990 = CARTESIAN_POINT ( 'NONE',  ( 11.32565050298867781, -16.48467196965851045, 7.626218077512944227 ) ) ;
#27991 = CARTESIAN_POINT ( 'NONE',  ( -8.257638164125266300, -14.92340941578111746, 5.704143890883081269 ) ) ;
#27992 = AXIS2_PLACEMENT_3D ( 'NONE', #14977, #12183, #24014 ) ;
#27993 = CARTESIAN_POINT ( 'NONE',  ( -29.61203839202723032, 15.40012917324033381, 37.38016955275591613 ) ) ;
#27994 = PLANE ( 'NONE',  #30208 ) ;
#27995 = ORIENTED_EDGE ( 'NONE', *, *, #29759, .T. ) ;
#27996 = CARTESIAN_POINT ( 'NONE',  ( 0.000000000000000000, 0.000000000000000000, 1.500000000000001332 ) ) ;
#27997 = DIRECTION ( 'NONE',  ( 0.1423148382732746797, -0.9898214418809342385, 0.000000000000000000 ) ) ;
#27998 = CYLINDRICAL_SURFACE ( 'NONE', #23185, 0.7500000000000006661 ) ;
#27999 = CARTESIAN_POINT ( 'NONE',  ( -47.15881708134175199, 69.79865606594935912, 15.50986296560572875 ) ) ;
#28000 = DIRECTION ( 'NONE',  ( 1.000000000000000000, 0.000000000000000000, 0.000000000000000000 ) ) ;
#28001 = CARTESIAN_POINT ( 'NONE',  ( 49.99999999999998579, 50.00000000000000000, 97.07879600563551037 ) ) ;
#28002 = DIRECTION ( 'NONE',  ( -0.4539545692076746852, 0.8910248307962436165, 0.000000000000000000 ) ) ;
#28003 = CARTESIAN_POINT ( 'NONE',  ( -24.03057240117691862, 26.57182937991349903, -6.500000000000000888 ) ) ;
#28004 = CARTESIAN_POINT ( 'NONE',  ( 0.000000000000000000, 0.000000000000000000, 85.49999999999998579 ) ) ;
#28005 = AXIS2_PLACEMENT_3D ( 'NONE', #27972, #18612, #7053 ) ;
#28006 = CARTESIAN_POINT ( 'NONE',  ( -18.47348503376730022, -7.710222065540593306, 19.45164628100866722 ) ) ;
#28007 = DIRECTION ( 'NONE',  ( -0.7071067811865541231, 0.000000000000000000, 0.7071067811865408004 ) ) ;
#28008 = EDGE_LOOP ( 'NONE', ( #6503, #13959 ) ) ;
#28009 = VERTEX_POINT ( 'NONE', #26070 ) ;
#28010 = CARTESIAN_POINT ( 'NONE',  ( 9.131494062835614045, 2.555255504830995061, 13.00000000000000178 ) ) ;
#28011 = CARTESIAN_POINT ( 'NONE',  ( -39.00000000000000000, -5.563236990218529243, -1.500000000000000000 ) ) ;
#28012 = CARTESIAN_POINT ( 'NONE',  ( 11.80555446153501897, -11.55276080277260320, -0.6213203435596476032 ) ) ;
#28013 = EDGE_LOOP ( 'NONE', ( #2514, #16811, #22563, #19228 ) ) ;
#28014 = CARTESIAN_POINT ( 'NONE',  ( 17.92455701194924700, -8.912206770388250376, 19.45164628100866722 ) ) ;
#28015 = DIRECTION ( 'NONE',  ( 1.000000000000000000, 0.000000000000000000, 0.000000000000000000 ) ) ;
#28016 = EDGE_CURVE ( 'NONE', #25162, #23566, #28569, .T. ) ;
#28017 = ORIENTED_EDGE ( 'NONE', *, *, #23066, .T. ) ;
#28018 = CARTESIAN_POINT ( 'NONE',  ( -19.78695419347076623, 3.033347482080934299, 5.796888747622817029 ) ) ;
#28019 = CYLINDRICAL_SURFACE ( 'NONE', #10329, 1.000000000000000888 ) ;
#28020 = EDGE_CURVE ( 'NONE', #29733, #20591, #30737, .T. ) ;
#28021 = CYLINDRICAL_SURFACE ( 'NONE', #5040, 1.447898107987198646 ) ;
#28022 = ORIENTED_EDGE ( 'NONE', *, *, #11480, .F. ) ;
#28023 = CARTESIAN_POINT ( 'NONE',  ( 5.291486201320592109, 19.28729773841935469, 18.34798005863227388 ) ) ;
#28024 = AXIS2_PLACEMENT_3D ( 'NONE', #14110, #9747, #88 ) ;
#28025 = AXIS2_PLACEMENT_3D ( 'NONE', #25435, #3920, #18255 ) ;
#28026 = EDGE_CURVE ( 'NONE', #29503, #26411, #7049, .T. ) ;
#28027 = VECTOR ( 'NONE', #3382, 1000.000000000000000 ) ;
#28028 = CARTESIAN_POINT ( 'NONE',  ( -27.03074382657074537, 6.449748410230984774, 42.96778633356043287 ) ) ;
#28029 = CYLINDRICAL_SURFACE ( 'NONE', #29273, 0.7499999999999997780 ) ;
#28030 = VERTEX_POINT ( 'NONE', #19200 ) ;
#28031 = CARTESIAN_POINT ( 'NONE',  ( 16.86493654369872175, 2.320966539700319853, 19.85270094495841775 ) ) ;
#28032 = FILL_AREA_STYLE ('',( #27894 ) ) ;
#28033 = LINE ( 'NONE', #16179, #27566 ) ;
#28034 = CARTESIAN_POINT ( 'NONE',  ( -0.6129396130214317395, -20.00853051056088816, 6.974106381145714018 ) ) ;
#28035 = ADVANCED_FACE ( 'NONE', ( #28728 ), #3954, .F. ) ;
#28036 = CARTESIAN_POINT ( 'NONE',  ( -37.99999999999999289, 90.00000000000001421, -75.50000000000000000 ) ) ;
#28037 = EDGE_CURVE ( 'NONE', #4581, #27445, #491, .T. ) ;
#28038 = LINE ( 'NONE', #6665, #4075 ) ;
#28039 = CARTESIAN_POINT ( 'NONE',  ( -19.96222469201676475, 1.488090962520938865, 19.25672174529527325 ) ) ;
#28040 = DIRECTION ( 'NONE',  ( 1.000000000000000000, 0.000000000000000000, 0.000000000000000000 ) ) ;
#28041 = EDGE_LOOP ( 'NONE', ( #8894, #28802, #25174, #7158 ) ) ;
#28042 = CARTESIAN_POINT ( 'NONE',  ( 2.338573377552013888, -39.50000000000001421, 27.50000000000001066 ) ) ;
#28043 = ORIENTED_EDGE ( 'NONE', *, *, #836, .T. ) ;
#28044 = VERTEX_POINT ( 'NONE', #24815 ) ;
#28045 = VECTOR ( 'NONE', #3496, 1000.000000000000000 ) ;
#28046 = DIRECTION ( 'NONE',  ( -1.000000000000000000, 0.000000000000000000, 0.000000000000000000 ) ) ;
#28047 = AXIS2_PLACEMENT_3D ( 'NONE', #28933, #12559, #22051 ) ;
#28048 = LINE ( 'NONE', #20870, #15351 ) ;
#28049 = ORIENTED_EDGE ( 'NONE', *, *, #8260, .T. ) ;
#28050 = CARTESIAN_POINT ( 'NONE',  ( 7.538175180318423152, 5.069257791428403159, 13.22130136205108819 ) ) ;
#28051 = EDGE_CURVE ( 'NONE', #5139, #11277, #10469, .T. ) ;
#28052 = AXIS2_PLACEMENT_3D ( 'NONE', #29878, #6004, #22670 ) ;
#28053 = DIRECTION ( 'NONE',  ( 1.000000000000000000, 0.000000000000000000, 0.000000000000000000 ) ) ;
#28054 = VERTEX_POINT ( 'NONE', #19659 ) ;
#28055 = EDGE_CURVE ( 'NONE', #10205, #28599, #6353, .T. ) ;
#28056 = CARTESIAN_POINT ( 'NONE',  ( -23.17581250239728519, 34.50630206824672541, -1.499999999999999778 ) ) ;
#28057 = EDGE_CURVE ( 'NONE', #4214, #18898, #26862, .T. ) ;
#28058 = CARTESIAN_POINT ( 'NONE',  ( 4.390207617113956573, -7.856594496258208160, -1.500000000000002665 ) ) ;
#28059 = VERTEX_POINT ( 'NONE', #10623 ) ;
#28060 = DIRECTION ( 'NONE',  ( -0.000000000000000000, -0.000000000000000000, 1.000000000000000000 ) ) ;
#28061 = EDGE_CURVE ( 'NONE', #24670, #2627, #8138, .T. ) ;
#28062 = VERTEX_POINT ( 'NONE', #21856 ) ;
#28063 = FACE_OUTER_BOUND ( 'NONE', #19375, .T. ) ;
#28064 = ADVANCED_FACE ( 'NONE', ( #20135 ), #1441, .T. ) ;
#28065 = EDGE_LOOP ( 'NONE', ( #18693, #10913, #23944, #16924 ) ) ;
#28066 = ORIENTED_EDGE ( 'NONE', *, *, #3470, .T. ) ;
#28067 = ADVANCED_FACE ( 'NONE', ( #4064 ), #13445, .F. ) ;
#28068 = AXIS2_PLACEMENT_3D ( 'NONE', #11243, #23081, #20740 ) ;
#28069 = ADVANCED_FACE ( 'NONE', ( #11087 ), #23068, .F. ) ;
#28070 = AXIS2_PLACEMENT_3D ( 'NONE', #14039, #30571, #28549 ) ;
#28071 = CARTESIAN_POINT ( 'NONE',  ( -49.99999999999998579, 90.00000000000001421, -34.49999999999998579 ) ) ;
#28072 = CARTESIAN_POINT ( 'NONE',  ( -2.081668171172168513E-14, 75.00000000000001421, 37.49999999999999289 ) ) ;
#28073 = B_SPLINE_CURVE_WITH_KNOTS ( 'NONE', 3,
 ( #14018, #11222, #23376, #23210, #1864, #11389 ),
 .UNSPECIFIED., .F., .F.,
 ( 4, 2, 4 ),
 ( 0.001794032523745612293, 0.007046146517948603805, 0.01388807892444512623 ),
 .UNSPECIFIED. ) ;
#28074 = EDGE_CURVE ( 'NONE', #13253, #20986, #21795, .T. ) ;
#28075 = CARTESIAN_POINT ( 'NONE',  ( -34.83396020575241891, -10.30249279383514960, 34.80090346875805096 ) ) ;
#28076 = DIRECTION ( 'NONE',  ( 0.000000000000000000, -0.5000000000000006661, -0.8660254037844382635 ) ) ;
#28077 = CARTESIAN_POINT ( 'NONE',  ( 16.74250592919979752, 3.198927888535952668, 18.34798005862930736 ) ) ;
#28078 = EDGE_LOOP ( 'NONE', ( #26812, #7201 ) ) ;
#28079 = CARTESIAN_POINT ( 'NONE',  ( 10.58066667298599661, -16.99307187112385620, 7.429667576816606278 ) ) ;
#28080 = FACE_OUTER_BOUND ( 'NONE', #19547, .T. ) ;
#28081 = CARTESIAN_POINT ( 'NONE',  ( -15.45023549775890004, 12.72816703665372984, 20.33971507717571114 ) ) ;
#28082 = CARTESIAN_POINT ( 'NONE',  ( 4.469338653509383974, 19.51245501789046344, 19.89182036555910571 ) ) ;
#28083 = ORIENTED_EDGE ( 'NONE', *, *, #18625, .T. ) ;
#28084 = EDGE_LOOP ( 'NONE', ( #13411, #19316, #9876, #9698 ) ) ;
#28085 = CARTESIAN_POINT ( 'NONE',  ( -18.04365185506138047, -8.627086862512674870, 7.652108011868850035 ) ) ;
#28086 = CARTESIAN_POINT ( 'NONE',  ( 23.21352257770656990, 10.78826658734920230, 45.15942333309104129 ) ) ;
#28087 = DIRECTION ( 'NONE',  ( 0.000000000000000000, 0.000000000000000000, 1.000000000000000000 ) ) ;
#28088 = B_SPLINE_SURFACE_WITH_KNOTS ( 'NONE', 1, 3, ( 
 ( #10059, #7884, #29088, #28939, #27061, #7730, #26602, #231, #9744, #19258, #7417, #26445, #17390, #5074, #12243, #29702, #27526, #20641, #15503, #3512, #25167, #15182, #10520, #8346, #25332, #15653, #25020, #13026, #22831, #1013, #12878, #24704, #1482, #22377, #3973, #22977, #18163, #6147, #20493, #8655, #29552, #17862 ),
 ( #10672, #22513, #27209, #1162, #13493, #3659, #3811, #10994, #5846, #13334, #20031, #8186, #11144, #22666, #15812, #30014, #15346, #30160, #27670, #8792, #18319, #6299, #1317, #27379, #5686, #24876, #5999, #3346, #13173, #10836, #20344, #29874, #8514, #14072, #11743, #30769, #23129, #23734, #6609, #23581, #6755, #16270 ) ),
 .UNSPECIFIED., .F., .T., .F.,
 ( 2, 2 ),
 ( 4, 2, 2, 2, 2, 2, 2, 2, 2, 2, 2, 2, 2, 2, 2, 2, 2, 2, 2, 2, 4 ),
 ( 0.000000000000000000, 1.000000000000000000 ),
 ( 0.000000000000000000, 0.1963495408493620697, 0.3926990816987241395, 0.7853981633974482790, 1.178097245096172418, 1.570796326794896558, 1.963495408493620697, 2.356194490192344837, 2.748893571891068976, 2.945243112740430824, 3.141592653589793116, 3.337942194439155408, 3.534291735288517255, 3.926990816987241395, 4.319689898685965090, 4.712388980384689674, 5.105088062083414258, 5.497787143782137953, 5.890486225480861648, 6.086835766330223940, 6.283185307179586232 ),
 .UNSPECIFIED. ) ;
#28089 = CARTESIAN_POINT ( 'NONE',  ( -5.332709978455694610, 16.18357461815304532, 18.36582235739946611 ) ) ;
#28090 = LINE ( 'NONE', #18888, #23062 ) ;
#28091 = CARTESIAN_POINT ( 'NONE',  ( -29.06918585179853665, 23.33130127174517554, 27.50000000000000711 ) ) ;
#28092 = AXIS2_PLACEMENT_3D ( 'NONE', #25793, #16570, #11450 ) ;
#28093 = CONTEXT_DEPENDENT_SHAPE_REPRESENTATION ( #10992, #202 ) ;
#28094 = EDGE_CURVE ( 'NONE', #22863, #10221, #13125, .T. ) ;
#28095 = DIRECTION ( 'NONE',  ( -0.000000000000000000, -0.000000000000000000, -1.000000000000000000 ) ) ;
#28096 = ORIENTED_EDGE ( 'NONE', *, *, #14936, .T. ) ;
#28097 = AXIS2_PLACEMENT_3D ( 'NONE', #25116, #16065, #1713 ) ;
#28098 = ADVANCED_FACE ( 'NONE', ( #22619 ), #13729, .F. ) ;
#28099 = B_SPLINE_CURVE_WITH_KNOTS ( 'NONE', 3,
 ( #8721, #18235, #27756, #29628 ),
 .UNSPECIFIED., .F., .F.,
 ( 4, 4 ),
 ( 2.143643656948718959E-07, 0.003421830178490221138 ),
 .UNSPECIFIED. ) ;
#28100 = CARTESIAN_POINT ( 'NONE',  ( 0.9714284548196548963, -19.97661650614235995, 7.454606537396340826 ) ) ;
#28101 = CARTESIAN_POINT ( 'NONE',  ( -35.13802340818978820, 8.772855875111229551, 34.58409965093399308 ) ) ;
#28102 = EDGE_CURVE ( 'NONE', #9249, #9573, #4849, .T. ) ;
#28103 = CARTESIAN_POINT ( 'NONE',  ( 32.28307784207223108, 8.475829241206289666, 41.62281023987511475 ) ) ;
#28104 = VERTEX_POINT ( 'NONE', #11232 ) ;
#28105 = CARTESIAN_POINT ( 'NONE',  ( -50.00000000000000000, 50.00000000000000000, 97.07879600563551037 ) ) ;
#28106 = EDGE_LOOP ( 'NONE', ( #5045, #6383 ) ) ;
#28107 = CARTESIAN_POINT ( 'NONE',  ( -4.281329142241829366, -42.25336671256035004, 28.86098669521330251 ) ) ;
#28108 = CARTESIAN_POINT ( 'NONE',  ( -22.44164183933027701, 36.72099769060108088, -16.50000000000000000 ) ) ;
#28109 = VERTEX_POINT ( 'NONE', #20728 ) ;
#28110 = CARTESIAN_POINT ( 'NONE',  ( 0.3567147238643512130, -19.99681861211370659, 5.652196082369963293 ) ) ;
#28111 = APPLICATION_CONTEXT ( 'automotive_design' ) ;
#28112 = CARTESIAN_POINT ( 'NONE',  ( -40.00000000000002842, 80.00000000000001421, 52.50000000000014921 ) ) ;
#28113 = CARTESIAN_POINT ( 'NONE',  ( 2.168404344971008868E-16, 42.50000000000000711, -1.500000000000000000 ) ) ;
#28114 = CARTESIAN_POINT ( 'NONE',  ( -21.37787209074186734, -24.17206580633116175, -16.50001200000000523 ) ) ;
#28115 = CARTESIAN_POINT ( 'NONE',  ( -5.686690470302443678, 16.07334902597871462, 20.33971507717571114 ) ) ;
#28116 = VECTOR ( 'NONE', #10567, 1000.000000000000000 ) ;
#28117 = DIRECTION ( 'NONE',  ( 0.000000000000000000, 0.000000000000000000, -1.000000000000000000 ) ) ;
#28118 = DIRECTION ( 'NONE',  ( -1.000000000000000000, 0.000000000000000000, 0.000000000000000000 ) ) ;
#28119 = ORIENTED_EDGE ( 'NONE', *, *, #28270, .F. ) ;
#28120 = DIRECTION ( 'NONE',  ( 0.000000000000000000, 0.000000000000000000, 1.000000000000000000 ) ) ;
#28121 = CYLINDRICAL_SURFACE ( 'NONE', #10808, 1.447898107987170890 ) ;
#28122 = VERTEX_POINT ( 'NONE', #30108 ) ;
#28123 = DIRECTION ( 'NONE',  ( 0.000000000000000000, 1.000000000000000000, 0.000000000000000000 ) ) ;
#28124 = CARTESIAN_POINT ( 'NONE',  ( -14.92167319134950176, -8.273715889511853661, 18.50655187082627862 ) ) ;
#28125 = EDGE_CURVE ( 'NONE', #9621, #20672, #15308, .T. ) ;
#28126 = FILL_AREA_STYLE ('',( #13780 ) ) ;
#28127 = EDGE_CURVE ( 'NONE', #16284, #19910, #3362, .T. ) ;
#28128 = DIRECTION ( 'NONE',  ( 0.9329908884337522190, 0.3598999890241700306, 0.000000000000000000 ) ) ;
#28129 = ORIENTED_EDGE ( 'NONE', *, *, #29040, .F. ) ;
#28130 = FACE_OUTER_BOUND ( 'NONE', #12382, .T. ) ;
#28131 = CARTESIAN_POINT ( 'NONE',  ( 37.99999999999999289, 90.00000000000001421, -28.49999999999999645 ) ) ;
#28132 = CARTESIAN_POINT ( 'NONE',  ( 24.45718231057517400, -33.13439223474804862, 29.72618443979869696 ) ) ;
#28133 = CARTESIAN_POINT ( 'NONE',  ( -4.163336342344337027E-14, 1.387778780781445676E-14, 24.50000000000000000 ) ) ;
#28134 = ORIENTED_EDGE ( 'NONE', *, *, #4959, .F. ) ;
#28135 = CARTESIAN_POINT ( 'NONE',  ( -33.42925964089141644, -11.06161099612212695, 35.54550565580013455 ) ) ;
#28136 = ORIENTED_EDGE ( 'NONE', *, *, #18563, .F. ) ;
#28137 = CARTESIAN_POINT ( 'NONE',  ( -2.552544031601109875, 42.50000000001772094, -1.500000000000000000 ) ) ;
#28138 = CARTESIAN_POINT ( 'NONE',  ( -19.84344116185557283, 2.497567387674354489, 7.652108011868850035 ) ) ;
#28139 = ORIENTED_EDGE ( 'NONE', *, *, #7710, .T. ) ;
#28140 = CARTESIAN_POINT ( 'NONE',  ( 37.16608720827707657, -65.00000000000000000, 57.49999999999999289 ) ) ;
#28141 = VERTEX_POINT ( 'NONE', #11547 ) ;
#28142 = CARTESIAN_POINT ( 'NONE',  ( 7.856594496258195726, 4.390207617113981442, 1.500000000000001332 ) ) ;
#28143 = CARTESIAN_POINT ( 'NONE',  ( 1.750000000000008660, 16.48749217771910125, -0.6213203435596476032 ) ) ;
#28144 = ORIENTED_EDGE ( 'NONE', *, *, #15805, .T. ) ;
#28145 = CARTESIAN_POINT ( 'NONE',  ( 18.67280747382545769, -7.164419611389377884, 6.149077423860698666 ) ) ;
#28146 = CARTESIAN_POINT ( 'NONE',  ( -5.976018955020172108, 19.08630078664910812, 18.34798005863227388 ) ) ;
#28147 = DIRECTION ( 'NONE',  ( 0.000000000000000000, 0.000000000000000000, 1.000000000000000000 ) ) ;
#28148 = CYLINDRICAL_SURFACE ( 'NONE', #30071, 0.7500000000000006661 ) ;
#28149 = ORIENTED_EDGE ( 'NONE', *, *, #16290, .T. ) ;
#28150 = CARTESIAN_POINT ( 'NONE',  ( -7.869584159753960861, 10.39565510934976977, 24.50000000000000000 ) ) ;
#28151 = DIRECTION ( 'NONE',  ( -0.000000000000000000, -0.000000000000000000, -1.000000000000000000 ) ) ;
#28152 = DIRECTION ( 'NONE',  ( 0.000000000000000000, 1.000000000000000000, 0.000000000000000000 ) ) ;
#28153 = CARTESIAN_POINT ( 'NONE',  ( 0.8981854125223266427, 42.50000000000000711, 19.72227980406324832 ) ) ;
#28154 = CARTESIAN_POINT ( 'NONE',  ( -24.18487066411276487, 13.30660647122584983, 43.15349873716021278 ) ) ;
#28155 = FACE_OUTER_BOUND ( 'NONE', #12686, .T. ) ;
#28156 = CARTESIAN_POINT ( 'NONE',  ( -4.102102735472396233, 8.549050687778207092, 13.00000000000000178 ) ) ;
#28157 = ORIENTED_EDGE ( 'NONE', *, *, #18141, .T. ) ;
#28158 = VERTEX_POINT ( 'NONE', #4669 ) ;
#28159 = CARTESIAN_POINT ( 'NONE',  ( 32.82330813384650270, 22.94799032727486932, -1.500000000000000000 ) ) ;
#28160 = CARTESIAN_POINT ( 'NONE',  ( -7.671759676023399699, -15.25818751172876198, 6.783738457429058677 ) ) ;
#28161 = CARTESIAN_POINT ( 'NONE',  ( -14.36006998371493637, -17.26937953831884442, 1.500000000000000000 ) ) ;
#28162 = ORIENTED_EDGE ( 'NONE', *, *, #20033, .F. ) ;
#28163 = CARTESIAN_POINT ( 'NONE',  ( 0.000000000000000000, 0.000000000000000000, 0.000000000000000000 ) ) ;
#28164 = CARTESIAN_POINT ( 'NONE',  ( 15.51722275458701894, -7.010743380608707831, 18.63641924841378028 ) ) ;
#28165 = PRESENTATION_LAYER_ASSIGNMENT (  '', '', ( #24238 ) ) ;
#28166 = CARTESIAN_POINT ( 'NONE',  ( 4.270667257859593668, 16.49544336893745111, 7.632642797338977658 ) ) ;
#28167 = ORIENTED_EDGE ( 'NONE', *, *, #15854, .F. ) ;
#28168 = CARTESIAN_POINT ( 'NONE',  ( -19.73562743738981951, 3.350138464993958287, 6.111214848085761986 ) ) ;
#28169 = CARTESIAN_POINT ( 'NONE',  ( 11.66141461333273810, 12.47704237144458084, 6.782048567692550378 ) ) ;
#28170 = CARTESIAN_POINT ( 'NONE',  ( -35.86518915568154142, 11.02596425420269100, 37.50000000003379341 ) ) ;
#28171 = ORIENTED_EDGE ( 'NONE', *, *, #25028, .T. ) ;
#28172 = PLANE ( 'NONE',  #20818 ) ;
#28173 = AXIS2_PLACEMENT_3D ( 'NONE', #3204, #5543, #29098 ) ;
#28174 = B_SPLINE_CURVE_WITH_KNOTS ( 'NONE', 3,
 ( #20375, #3541, #1659, #1350, #25200, #3844, #18505, #27704, #6333, #27410, #15848, #25365, #3998, #8379, #8830, #30192, #27867, #20209, #11329, #6028 ),
 .UNSPECIFIED., .F., .F.,
 ( 4, 2, 2, 2, 2, 2, 2, 2, 2, 4 ),
 ( 0.000000000000000000, 0.06250000000000163758, 0.1250000000000032752, 0.1875000000000049127, 0.2187500000000050793, 0.2500000000000052736, 0.3125000000000039413, 0.3750000000000026645, 0.4375000000000013323, 0.5000000000000000000 ),
 .UNSPECIFIED. ) ;
#28175 = DIRECTION ( 'NONE',  ( 0.000000000000000000, 0.000000000000000000, -1.000000000000000000 ) ) ;
#28176 = CIRCLE ( 'NONE', #15734, 1.447898107987198646 ) ;
#28177 = CARTESIAN_POINT ( 'NONE',  ( 7.856594496258195726, 4.390207617113981442, 1.500000000000001332 ) ) ;
#28178 = ORIENTED_EDGE ( 'NONE', *, *, #4837, .T. ) ;
#28179 = CARTESIAN_POINT ( 'NONE',  ( 16.87925085231059796, 2.194398682741037554, 19.21496526180053621 ) ) ;
#28180 = PLANE ( 'NONE',  #17775 ) ;
#28181 = CARTESIAN_POINT ( 'NONE',  ( -30.75232512042845556, -9.966982604840850968, -1.500000000000000000 ) ) ;
#28182 = CARTESIAN_POINT ( 'NONE',  ( -0.09481216811183805493, -20.01790837231453679, 7.557577766377196582 ) ) ;
#28183 = CIRCLE ( 'NONE', #21693, 14.52510309069105965 ) ;
#28184 = CARTESIAN_POINT ( 'NONE',  ( 25.41307773079512344, -6.523700759042262654, 48.76310947883586522 ) ) ;
#28185 = CARTESIAN_POINT ( 'NONE',  ( -3.221450758838616757, -1.621276839356792454, 1.500000000000000000 ) ) ;
#28186 = CARTESIAN_POINT ( 'NONE',  ( -17.06158983937614337, 0.7019473037495057577, 19.69140814234746273 ) ) ;
#28187 = LINE ( 'NONE', #30386, #23834 ) ;
#28188 = ORIENTED_EDGE ( 'NONE', *, *, #26145, .F. ) ;
#28189 = CARTESIAN_POINT ( 'NONE',  ( -6.476765594709835483, 15.80122980073540084, 6.392658652357120275 ) ) ;
#28190 = FACE_OUTER_BOUND ( 'NONE', #27459, .T. ) ;
#28191 = ORIENTED_EDGE ( 'NONE', *, *, #5617, .T. ) ;
#28192 = EDGE_LOOP ( 'NONE', ( #15343, #4292, #12067, #17902 ) ) ;
#28193 = VECTOR ( 'NONE', #10236, 1000.000000000000000 ) ;
#28194 = EDGE_CURVE ( 'NONE', #18819, #2982, #2187, .T. ) ;
#28195 = CARTESIAN_POINT ( 'NONE',  ( -15.66344362052393002, 12.43669181132026580, 7.528076282304597022 ) ) ;
#28196 = EDGE_CURVE ( 'NONE', #27328, #20523, #24775, .T. ) ;
#28197 = CARTESIAN_POINT ( 'NONE',  ( 46.99999999999998579, 90.00000000000001421, 22.49999999999999289 ) ) ;
#28198 = ORIENTED_EDGE ( 'NONE', *, *, #1199, .F. ) ;
#28199 = VECTOR ( 'NONE', #11602, 1000.000000000000000 ) ;
#28200 = DIRECTION ( 'NONE',  ( 1.000000000000000000, 0.000000000000000000, 0.000000000000000000 ) ) ;
#28201 = VERTEX_POINT ( 'NONE', #7327 ) ;
#28202 = CARTESIAN_POINT ( 'NONE',  ( 8.999114229549594057, -0.1262659238204522361, 1.500000000000001332 ) ) ;
#28203 = VECTOR ( 'NONE', #12276, 1000.000000000000000 ) ;
#28204 = DIRECTION ( 'NONE',  ( -0.000000000000000000, 1.132880637372608986E-16, -1.000000000000000000 ) ) ;
#28205 = VERTEX_POINT ( 'NONE', #23843 ) ;
#28206 = CARTESIAN_POINT ( 'NONE',  ( 16.91972452348793610, -3.442972353390052920, 24.50000000000000000 ) ) ;
#28207 = ORIENTED_EDGE ( 'NONE', *, *, #24240, .T. ) ;
#28208 = DIRECTION ( 'NONE',  ( 1.000000000000000000, 0.000000000000000000, 0.000000000000000000 ) ) ;
#28209 = ORIENTED_EDGE ( 'NONE', *, *, #28350, .F. ) ;
#28210 = VERTEX_POINT ( 'NONE', #18568 ) ;
#28211 = CIRCLE ( 'NONE', #24219, 0.7500000000000006661 ) ;
#28212 = AXIS2_PLACEMENT_3D ( 'NONE', #10398, #17886, #24423 ) ;
#28213 = CYLINDRICAL_SURFACE ( 'NONE', #3651, 10.00000000000000000 ) ;
#28214 = DIRECTION ( 'NONE',  ( 0.000000000000000000, 1.000000000000000000, 0.000000000000000000 ) ) ;
#28215 = EDGE_CURVE ( 'NONE', #21196, #9030, #23277, .T. ) ;
#28216 = AXIS2_PLACEMENT_3D ( 'NONE', #10987, #20635, #30154 ) ;
#28217 = CARTESIAN_POINT ( 'NONE',  ( -14.71865621670870894, -8.659590923294997467, 19.08844262864050023 ) ) ;
#28218 = CARTESIAN_POINT ( 'NONE',  ( 1.590931199639277205, -16.99685872686718824, 18.73314399819311760 ) ) ;
#28219 = CARTESIAN_POINT ( 'NONE',  ( 16.77777292147013810, 2.975267875541937723, 18.36582235739946611 ) ) ;
#28220 = EDGE_CURVE ( 'NONE', #22179, #25840, #22295, .T. ) ;
#28221 = ORIENTED_EDGE ( 'NONE', *, *, #4558, .F. ) ;
#28222 = ADVANCED_FACE ( 'NONE', ( #28689 ), #26352, .F. ) ;
#28223 = CARTESIAN_POINT ( 'NONE',  ( -16.81737828845395910, 2.629481162813160910, 19.11611934778430921 ) ) ;
#28224 = CARTESIAN_POINT ( 'NONE',  ( 0.000000000000000000, -3.165563358393047634E-15, 27.94260272410217638 ) ) ;
#28225 = CARTESIAN_POINT ( 'NONE',  ( -15.85879827683067944, 12.21494667905097131, 6.041646659195333058 ) ) ;
#28226 = AXIS2_PLACEMENT_3D ( 'NONE', #7873, #26903, #3801 ) ;
#28227 = CARTESIAN_POINT ( 'NONE',  ( 10.47960520055065992, -7.757439966934453146, 1.500000000000001332 ) ) ;
#28228 = ORIENTED_EDGE ( 'NONE', *, *, #35, .T. ) ;
#28229 = EDGE_LOOP ( 'NONE', ( #12381, #13715 ) ) ;
#28230 = CARTESIAN_POINT ( 'NONE',  ( -25.64627119138473432, 23.40052582045089480, -16.50001200000000168 ) ) ;
#28231 =( GEOMETRIC_REPRESENTATION_CONTEXT ( 3 ) GLOBAL_UNCERTAINTY_ASSIGNED_CONTEXT ( ( #16703 ) ) GLOBAL_UNIT_ASSIGNED_CONTEXT ( ( #9309, #1836, #2133 ) ) REPRESENTATION_CONTEXT ( 'NONE', 'WORKASPACE' ) );
#28232 = EDGE_CURVE ( 'NONE', #11068, #26161, #2020, .T. ) ;
#28233 = DIRECTION ( 'NONE',  ( 0.000000000000000000, 0.000000000000000000, 1.000000000000000000 ) ) ;
#28234 = EDGE_CURVE ( 'NONE', #12141, #7038, #1095, .T. ) ;
#28235 = CARTESIAN_POINT ( 'NONE',  ( 15.52089561533224504, 12.61365839305098646, 19.60917204426169747 ) ) ;
#28236 = DIRECTION ( 'NONE',  ( 0.000000000000000000, 0.000000000000000000, 1.000000000000000000 ) ) ;
#28237 = CARTESIAN_POINT ( 'NONE',  ( 8.999114229549594057, -0.1262659238204522361, 1.500000000000001332 ) ) ;
#28238 = VECTOR ( 'NONE', #14046, 1000.000000000000000 ) ;
#28239 = CARTESIAN_POINT ( 'NONE',  ( -31.54493124927535419, 19.07059040393068727, 27.50000000000000711 ) ) ;
#28240 = AXIS2_PLACEMENT_3D ( 'NONE', #12226, #14418, #9436 ) ;
#28241 = CARTESIAN_POINT ( 'NONE',  ( 8.303920738747214259, 3.683253992019856149, 13.22130136205108819 ) ) ;
#28242 = EDGE_CURVE ( 'NONE', #950, #15032, #373, .T. ) ;
#28243 = ORIENTED_EDGE ( 'NONE', *, *, #24861, .T. ) ;
#28244 = AXIS2_PLACEMENT_3D ( 'NONE', #28003, #15411, #3571 ) ;
#28245 = CARTESIAN_POINT ( 'NONE',  ( -16.98316914218901985, 1.504314895146021236, 7.643931100913408550 ) ) ;
#28246 = EDGE_CURVE ( 'NONE', #3032, #21118, #11849, .T. ) ;
#28247 = CARTESIAN_POINT ( 'NONE',  ( 14.53924466656745018, 13.73408656550489937, 20.22386025856689074 ) ) ;
#28248 = DIRECTION ( 'NONE',  ( 1.000000000000000000, 0.000000000000000000, 0.000000000000000000 ) ) ;
#28249 = ORIENTED_EDGE ( 'NONE', *, *, #13973, .T. ) ;
#28250 = EDGE_CURVE ( 'NONE', #28714, #11382, #9503, .T. ) ;
#28251 = DIRECTION ( 'NONE',  ( -0.4495526574063634095, -0.8932538319083086487, 0.000000000000000000 ) ) ;
#28252 = ORIENTED_EDGE ( 'NONE', *, *, #12317, .T. ) ;
#28253 = CARTESIAN_POINT ( 'NONE',  ( 18.70304204834580020, -7.134633872344111616, 6.233981582756856987 ) ) ;
#28254 = AXIS2_PLACEMENT_3D ( 'NONE', #13159, #22651, #1303 ) ;
#28255 = CYLINDRICAL_SURFACE ( 'NONE', #10540, 0.7500000000000002220 ) ;
#28256 = AXIS2_PLACEMENT_3D ( 'NONE', #29037, #19524, #334 ) ;
#28257 = SHAPE_REPRESENTATION ( 'Double-Lip Hydraulic Vanes', ( #7396 ), #3406 ) ;
#28258 = ORIENTED_EDGE ( 'NONE', *, *, #414, .T. ) ;
#28259 = CARTESIAN_POINT ( 'NONE',  ( 33.02695388770936802, 15.72686850277320936, 27.50000000000000355 ) ) ;
#28260 = VECTOR ( 'NONE', #27775, 1000.000000000000000 ) ;
#28261 = FACE_OUTER_BOUND ( 'NONE', #11229, .T. ) ;
#28262 = CARTESIAN_POINT ( 'NONE',  ( 0.000000000000000000, 42.50000000000000000, 27.50000000000000355 ) ) ;
#28263 = FACE_OUTER_BOUND ( 'NONE', #23037, .T. ) ;
#28264 = CIRCLE ( 'NONE', #877, 0.7500000000000011102 ) ;
#28265 = CARTESIAN_POINT ( 'NONE',  ( -6.789382699754180628, 18.83122862112907470, 19.89182036555910571 ) ) ;
#28266 = AXIS2_PLACEMENT_3D ( 'NONE', #25393, #27890, #6515 ) ;
#28267 = DIRECTION ( 'NONE',  ( 1.000000000000000000, 0.000000000000000000, 0.000000000000000000 ) ) ;
#28268 = DIRECTION ( 'NONE',  ( 0.6548607339452890974, 0.7557495743542548272, 0.000000000000000000 ) ) ;
#28269 = CARTESIAN_POINT ( 'NONE',  ( 28.37932450449293853, 10.51822134874671022, 1.500000000000000000 ) ) ;
#28270 = EDGE_CURVE ( 'NONE', #16046, #14399, #19322, .T. ) ;
#28271 = VERTEX_POINT ( 'NONE', #23421 ) ;
#28272 = ADVANCED_FACE ( 'NONE', ( #8642 ), #30150, .T. ) ;
#28273 = DIRECTION ( 'NONE',  ( -0.000000000000000000, -0.000000000000000000, 1.000000000000000000 ) ) ;
#28274 = AXIS2_PLACEMENT_3D ( 'NONE', #12786, #5459, #928 ) ;
#28275 = LINE ( 'NONE', #13637, #13351 ) ;
#28276 = DIRECTION ( 'NONE',  ( 0.000000000000000000, 1.000000000000000000, 1.193512090021232842E-16 ) ) ;
#28277 = EDGE_CURVE ( 'NONE', #20793, #1845, #21075, .T. ) ;
#28278 = ORIENTED_EDGE ( 'NONE', *, *, #1859, .T. ) ;
#28279 = DIRECTION ( 'NONE',  ( -0.000000000000000000, -0.000000000000000000, 1.000000000000000000 ) ) ;
#28280 = DIRECTION ( 'NONE',  ( 0.000000000000000000, 0.000000000000000000, -1.000000000000000000 ) ) ;
#28281 = CIRCLE ( 'NONE', #30761, 9.482273699623480212 ) ;
#28282 = DIRECTION ( 'NONE',  ( 0.000000000000000000, -0.000000000000000000, -1.000000000000000000 ) ) ;
#28283 = ADVANCED_FACE ( 'NONE', ( #25483 ), #20631, .F. ) ;
#28284 = CARTESIAN_POINT ( 'NONE',  ( 37.98493438987956949, 11.12428508576150143, -1.500000000000000000 ) ) ;
#28285 = AXIS2_PLACEMENT_3D ( 'NONE', #18154, #30597, #2059 ) ;
#28286 = CARTESIAN_POINT ( 'NONE',  ( -4.163336342344337027E-14, 1.387778780781445676E-14, 1.500000000000000000 ) ) ;
#28287 = VECTOR ( 'NONE', #23316, 1000.000000000000000 ) ;
#28288 = VERTEX_POINT ( 'NONE', #15800 ) ;
#28289 = DIRECTION ( 'NONE',  ( -0.000000000000000000, 0.000000000000000000, 1.000000000000000000 ) ) ;
#28290 = CARTESIAN_POINT ( 'NONE',  ( 24.35970437652574816, -13.37404834226503958, -16.55003854064094426 ) ) ;
#28291 = CARTESIAN_POINT ( 'NONE',  ( 12.47055468150928625, -35.37063655238940640, 37.50000000000014211 ) ) ;
#28292 = EDGE_CURVE ( 'NONE', #12174, #19662, #25809, .T. ) ;
#28293 = DIRECTION ( 'NONE',  ( -0.4154150130018860465, -0.9096319953545185522, 0.000000000000000000 ) ) ;
#28294 = ORIENTED_EDGE ( 'NONE', *, *, #2515, .F. ) ;
#28295 = CARTESIAN_POINT ( 'NONE',  ( -13.88720712120798240, 9.928229803729504255, 6.037360021877314686 ) ) ;
#28296 = VECTOR ( 'NONE', #4766, 1000.000000000000000 ) ;
#28297 = CARTESIAN_POINT ( 'NONE',  ( 7.730328572437743517, -4.608906612435629491, 21.50000000000000000 ) ) ;
#28298 = CARTESIAN_POINT ( 'NONE',  ( 6.482337650448408262, 6.364020599487815844, -1.500000000000001110 ) ) ;
#28299 = VECTOR ( 'NONE', #13352, 1000.000000000000000 ) ;
#28300 = ORIENTED_EDGE ( 'NONE', *, *, #18240, .T. ) ;
#28301 = VERTEX_POINT ( 'NONE', #30303 ) ;
#28302 = DIRECTION ( 'NONE',  ( 1.000000000000000000, 0.000000000000000000, 0.000000000000000000 ) ) ;
#28303 = VERTEX_POINT ( 'NONE', #25633 ) ;
#28304 = CARTESIAN_POINT ( 'NONE',  ( -0.6388627779519727712, -20.00771244368417712, 19.11611934778430921 ) ) ;
#28305 = AXIS2_PLACEMENT_3D ( 'NONE', #23365, #4793, #23509 ) ;
#28306 = EDGE_CURVE ( 'NONE', #29624, #25948, #26802, .T. ) ;
#28307 = CARTESIAN_POINT ( 'NONE',  ( -7.726154291500659355, -15.22816856119838924, 6.995624166085161910 ) ) ;
#28308 = EDGE_CURVE ( 'NONE', #5896, #17481, #6744, .T. ) ;
#28309 = CARTESIAN_POINT ( 'NONE',  ( 16.17735844207722806, -3.336236224685152685, 24.50000000000000000 ) ) ;
#28310 = CARTESIAN_POINT ( 'NONE',  ( 1.638502901550995761, -16.99392728441679878, 19.89182036555910571 ) ) ;
#28311 = AXIS2_PLACEMENT_3D ( 'NONE', #25087, #1542, #3730 ) ;
#28312 = ORIENTED_EDGE ( 'NONE', *, *, #24038, .T. ) ;
#28313 = CARTESIAN_POINT ( 'NONE',  ( 0.000000000000000000, -36.71644397333972165, 24.50000000000000000 ) ) ;
#28314 = LINE ( 'NONE', #22997, #2928 ) ;
#28315 = LINE ( 'NONE', #23310, #283 ) ;
#28316 = CARTESIAN_POINT ( 'NONE',  ( 19.54426622602687758, -37.07991288358297055, -1.499999999999999778 ) ) ;
#28317 = EDGE_LOOP ( 'NONE', ( #10471, #9725, #9261, #19496 ) ) ;
#28318 = AXIS2_PLACEMENT_3D ( 'NONE', #10344, #22491, #15320 ) ;
#28319 = CARTESIAN_POINT ( 'NONE',  ( -5.127072262013854242, -42.13114360820154047, 28.87158698979397897 ) ) ;
#28320 = CARTESIAN_POINT ( 'NONE',  ( -13.29453093330978319, 10.66243031780445527, 20.34789198813115974 ) ) ;
#28321 = CARTESIAN_POINT ( 'NONE',  ( -38.00000000000000711, 80.00000000000001421, 27.08257569495566841 ) ) ;
#28322 = DIRECTION ( 'NONE',  ( 1.000000000000000000, 0.000000000000000000, 0.000000000000000000 ) ) ;
#28323 = CARTESIAN_POINT ( 'NONE',  ( -18.30192086700451881, -8.065271870204643534, 20.14992337338002315 ) ) ;
#28324 = CARTESIAN_POINT ( 'NONE',  ( -15.39438215884103478, -7.285634741961048988, 20.19668224736330941 ) ) ;
#28325 = PLANE ( 'NONE',  #29546 ) ;
#28326 = ORIENTED_EDGE ( 'NONE', *, *, #6189, .F. ) ;
#28327 = ORIENTED_EDGE ( 'NONE', *, *, #19894, .T. ) ;
#28328 = CARTESIAN_POINT ( 'NONE',  ( 33.14492811172536335, 23.43596546612559806, -6.499905845448985531 ) ) ;
#28329 = CARTESIAN_POINT ( 'NONE',  ( 10.11202017158399968, 41.14070756921128691, -1.500000000000000000 ) ) ;
#28330 = PRODUCT_DEFINITION_FORMATION_WITH_SPECIFIED_SOURCE ( 'ANY', '', #22131, .NOT_KNOWN. ) ;
#28331 = DIRECTION ( 'NONE',  ( -0.000000000000000000, -0.000000000000000000, 1.000000000000000000 ) ) ;
#28332 = CARTESIAN_POINT ( 'NONE',  ( -7.548823014270604759, 5.738360882150024267, 21.50000000000000000 ) ) ;
#28333 = ORIENTED_EDGE ( 'NONE', *, *, #28242, .F. ) ;
#28334 = CARTESIAN_POINT ( 'NONE',  ( 0.000000000000000000, 0.000000000000000000, 0.000000000000000000 ) ) ;
#28335 = CARTESIAN_POINT ( 'NONE',  ( 15.42605794595426971, -7.198932956632622115, 19.77662771831109367 ) ) ;
#28336 = CARTESIAN_POINT ( 'NONE',  ( 6.249808329856143985, 19.01727106391103916, 6.420335371522007506 ) ) ;
#28337 = VERTEX_POINT ( 'NONE', #4105 ) ;
#28338 = CARTESIAN_POINT ( 'NONE',  ( 6.071284049926378934, 19.07508289763275400, 19.96783386855779341 ) ) ;
#28339 = DIRECTION ( 'NONE',  ( 0.000000000000000000, 1.000000000000000000, -0.000000000000000000 ) ) ;
#28340 = VECTOR ( 'NONE', #11631, 1000.000000000000000 ) ;
#28341 = LINE ( 'NONE', #14122, #9344 ) ;
#28342 = CARTESIAN_POINT ( 'NONE',  ( -35.58199486000248157, 17.45398116881282391, 34.79408014406299543 ) ) ;
#28343 = ORIENTED_EDGE ( 'NONE', *, *, #25932, .T. ) ;
#28344 = CARTESIAN_POINT ( 'NONE',  ( -8.728722367416567707, 2.516121109503271835, 21.50000000000000000 ) ) ;
#28345 = CARTESIAN_POINT ( 'NONE',  ( -8.999114229549592281, 0.1262659238205133538, 21.50000000000000000 ) ) ;
#28346 = CARTESIAN_POINT ( 'NONE',  ( -14.69412328735588069, 13.56780452301002526, 6.913388067999404640 ) ) ;
#28347 = EDGE_CURVE ( 'NONE', #24333, #12567, #2904, .T. ) ;
#28348 = ORIENTED_EDGE ( 'NONE', *, *, #431, .T. ) ;
#28349 = CARTESIAN_POINT ( 'NONE',  ( -15.46558767506644116, -7.123678207069781720, 7.359006845440219102 ) ) ;
#28350 = EDGE_CURVE ( 'NONE', #8430, #23138, #28275, .T. ) ;
#28351 = CARTESIAN_POINT ( 'NONE',  ( 16.74250988114177474, 3.198928528055117404, 18.34798005863078885 ) ) ;
#28352 = DIRECTION ( 'NONE',  ( -0.000000000000000000, -0.000000000000000000, -1.000000000000000000 ) ) ;
#28353 = DIRECTION ( 'NONE',  ( 1.000000000000000000, 0.000000000000000000, 0.000000000000000000 ) ) ;
#28354 = B_SPLINE_SURFACE_WITH_KNOTS ( 'NONE', 3, 1, ( 
 ( #16848, #16531 ),
 ( #21508, #4991 ),
 ( #18885, #26049 ),
 ( #9669, #14503 ),
 ( #20991, #13848 ),
 ( #11196, #23030 ) ),
 .UNSPECIFIED., .F., .F., .F.,
 ( 4, 2, 4 ),
 ( 2, 2 ),
 ( 1.408367944312347353, 1.570796326794896558, 1.733224709277802811 ),
 ( 0.000000000000000000, 1.000000000000000000 ),
 .UNSPECIFIED. ) ;
#28355 = CARTESIAN_POINT ( 'NONE',  ( -0.4512825100096616859, -20.01288639008904724, 7.272049892295485485 ) ) ;
#28356 = AXIS2_PLACEMENT_3D ( 'NONE', #12634, #19628, #24470 ) ;
#28357 = CARTESIAN_POINT ( 'NONE',  ( 26.58597676761596418, -6.321098805557485711, 47.67294373134342322 ) ) ;
#28358 = FACE_OUTER_BOUND ( 'NONE', #26421, .T. ) ;
#28359 = CARTESIAN_POINT ( 'NONE',  ( -16.96496223448354357, 1.652369715233089176, 20.34789198813115263 ) ) ;
#28360 = DIRECTION ( 'NONE',  ( 1.000000000000000000, 0.000000000000000000, 0.000000000000000000 ) ) ;
#28361 = ORIENTED_EDGE ( 'NONE', *, *, #27865, .F. ) ;
#28362 = CARTESIAN_POINT ( 'NONE',  ( -24.44496207165490276, 7.595930209050158588, -16.55003854064094426 ) ) ;
#28363 = AXIS2_PLACEMENT_3D ( 'NONE', #16229, #28095, #25608 ) ;
#28364 = CARTESIAN_POINT ( 'NONE',  ( -2.446529495465445958, -8.413215745754985875, -1.500000000000002665 ) ) ;
#28365 = ORIENTED_EDGE ( 'NONE', *, *, #17933, .F. ) ;
#28366 = EDGE_LOOP ( 'NONE', ( #308, #2490, #12028, #29654 ) ) ;
#28367 = CARTESIAN_POINT ( 'NONE',  ( 5.035381156335493991, 19.35612728853641329, 18.37545668562167478 ) ) ;
#28368 =( NAMED_UNIT ( * ) SI_UNIT ( $, .STERADIAN. ) SOLID_ANGLE_UNIT ( ) );
#28369 = ORIENTED_EDGE ( 'NONE', *, *, #9968, .T. ) ;
#28370 = VECTOR ( 'NONE', #8127, 1000.000000000000000 ) ;
#28371 = DIRECTION ( 'NONE',  ( -0.000000000000000000, -0.000000000000000000, -1.000000000000000000 ) ) ;
#28372 = ORIENTED_EDGE ( 'NONE', *, *, #16623, .F. ) ;
#28373 = CARTESIAN_POINT ( 'NONE',  ( 16.18635831298871963, -5.444400941729615973, 19.58863275299554019 ) ) ;
#28374 = FACE_OUTER_BOUND ( 'NONE', #4588, .T. ) ;
#28375 = LINE ( 'NONE', #4966, #11992 ) ;
#28376 = ORIENTED_EDGE ( 'NONE', *, *, #28456, .T. ) ;
#28377 = VERTEX_POINT ( 'NONE', #16111 ) ;
#28378 = ORIENTED_EDGE ( 'NONE', *, *, #25764, .T. ) ;
#28379 = CIRCLE ( 'NONE', #23398, 9.084132297865673777 ) ;
#28380 = ORIENTED_EDGE ( 'NONE', *, *, #27473, .F. ) ;
#28381 = DIRECTION ( 'NONE',  ( 0.000000000000000000, 0.000000000000000000, -1.000000000000000000 ) ) ;
#28382 = CARTESIAN_POINT ( 'NONE',  ( 0.6517800496514684072, -17.02970683165549914, 18.34727598691068096 ) ) ;
#28383 = AXIS2_PLACEMENT_3D ( 'NONE', #20215, #17899, #27413 ) ;
#28384 = CARTESIAN_POINT ( 'NONE',  ( 1.795183039316615270, -16.98367886218520795, 6.672349528511551497 ) ) ;
#28385 = CARTESIAN_POINT ( 'NONE',  ( -15.16517293421788537, -7.781889191988407006, 20.34789198813115263 ) ) ;
#28386 = CARTESIAN_POINT ( 'NONE',  ( 5.687793815610356241, -6.974883619896809606, 1.500000000000001332 ) ) ;
#28387 = CARTESIAN_POINT ( 'NONE',  ( 16.76050819728944319, 3.085824932809439591, 18.35377592296120497 ) ) ;
#28388 = ORIENTED_EDGE ( 'NONE', *, *, #23926, .T. ) ;
#28389 = CARTESIAN_POINT ( 'NONE',  ( -19.71887672257059165, 3.447422735172823050, 19.00652017443069752 ) ) ;
#28390 = CARTESIAN_POINT ( 'NONE',  ( 13.81384208584302975, -36.54172128922432705, 34.50000000000000000 ) ) ;
#28391 = FACE_BOUND ( 'NONE', #1045, .T. ) ;
#28392 = CARTESIAN_POINT ( 'NONE',  ( 4.608906612435600181, 7.730328572437758616, 21.50000000000000000 ) ) ;
#28393 = EDGE_LOOP ( 'NONE', ( #5877, #27912, #14164, #14886 ) ) ;
#28394 = ORIENTED_EDGE ( 'NONE', *, *, #15667, .F. ) ;
#28395 = CARTESIAN_POINT ( 'NONE',  ( 39.52380524533145945, -7.028748154382047808, -11.49999999999999645 ) ) ;
#28396 = CARTESIAN_POINT ( 'NONE',  ( 20.46975788395958418, -26.57181885929544407, -16.50000600000000262 ) ) ;
#28397 = DIRECTION ( 'NONE',  ( -0.000000000000000000, -0.000000000000000000, 1.000000000000000000 ) ) ;
#28398 = CARTESIAN_POINT ( 'NONE',  ( 37.99999999999999289, 209.2686044187655909, -69.50000000000000000 ) ) ;
#28399 = DIRECTION ( 'NONE',  ( 0.000000000000000000, 0.000000000000000000, -1.000000000000000000 ) ) ;
#28400 = CIRCLE ( 'NONE', #13991, 7.500000000000008882 ) ;
#28401 = CARTESIAN_POINT ( 'NONE',  ( -26.44471942863318148, -26.80494974449361933, 27.50000000000000000 ) ) ;
#28402 = CARTESIAN_POINT ( 'NONE',  ( 0.3593302862868688052, 3.504574740656565712, -9.000000000000003553 ) ) ;
#28403 = EDGE_LOOP ( 'NONE', ( #28494, #146 ) ) ;
#28404 = CARTESIAN_POINT ( 'NONE',  ( -19.94392260440443110, 1.716525891962611183, 7.280727868105637768 ) ) ;
#28405 = CARTESIAN_POINT ( 'NONE',  ( -14.89473990422384198, 17.79239818699320708, 1.500000000000000000 ) ) ;
#28406 = DIRECTION ( 'NONE',  ( 1.000000000000000000, 0.000000000000000000, 0.000000000000000000 ) ) ;
#28407 = ORIENTED_EDGE ( 'NONE', *, *, #26912, .T. ) ;
#28408 = CARTESIAN_POINT ( 'NONE',  ( -6.364020599487749230, 6.482337650448472210, 21.50000000000000000 ) ) ;
#28409 = EDGE_LOOP ( 'NONE', ( #23588, #23739, #17059, #17787 ) ) ;
#28410 = DIRECTION ( 'NONE',  ( 0.5406408174555974444, 0.8412535328311813165, 0.000000000000000000 ) ) ;
#28411 = DIRECTION ( 'NONE',  ( -0.000000000000000000, -0.000000000000000000, 1.000000000000000000 ) ) ;
#28412 = EDGE_CURVE ( 'NONE', #19937, #11840, #6901, .T. ) ;
#28413 = EDGE_LOOP ( 'NONE', ( #21264, #5888 ) ) ;
#28414 = CARTESIAN_POINT ( 'NONE',  ( 18.68937984944595954, -33.86068137868598171, 27.50000000000000000 ) ) ;
#28415 = CARTESIAN_POINT ( 'NONE',  ( 7.532524345205997562, 49.43623389526102585, -41.99159057664593320 ) ) ;
#28416 = EDGE_CURVE ( 'NONE', #4932, #24522, #23303, .T. ) ;
#28417 = DIRECTION ( 'NONE',  ( -0.000000000000000000, -0.000000000000000000, -1.000000000000000000 ) ) ;
#28418 = DIRECTION ( 'NONE',  ( -0.000000000000000000, -0.000000000000000000, -1.000000000000000000 ) ) ;
#28419 = CIRCLE ( 'NONE', #8015, 9.084132297865673777 ) ;
#28420 = CARTESIAN_POINT ( 'NONE',  ( -6.065925884476026653, 15.94726461227263847, 18.50655187082627862 ) ) ;
#28421 = CARTESIAN_POINT ( 'NONE',  ( -10.51100353655187192, -17.01524272303503338, 5.652196082369963293 ) ) ;
#28422 = DIRECTION ( 'NONE',  ( -0.000000000000000000, 0.000000000000000000, 1.000000000000000000 ) ) ;
#28423 = ORIENTED_EDGE ( 'NONE', *, *, #29545, .F. ) ;
#28424 = DIRECTION ( 'NONE',  ( -1.000000000000000000, 0.000000000000000000, 0.000000000000000000 ) ) ;
#28425 = EDGE_CURVE ( 'NONE', #1760, #22306, #1396, .T. ) ;
#28426 = CARTESIAN_POINT ( 'NONE',  ( -32.74775157610409337, 27.21557300919391054, -19.50000000000000355 ) ) ;
#28427 = DIRECTION ( 'NONE',  ( -0.000000000000000000, -0.000000000000000000, -1.000000000000000000 ) ) ;
#28428 = ORIENTED_EDGE ( 'NONE', *, *, #16501, .F. ) ;
#28429 = LINE ( 'NONE', #9094, #30488 ) ;
#28430 = EDGE_CURVE ( 'NONE', #23872, #10205, #11133, .T. ) ;
#28431 = LINE ( 'NONE', #28580, #21762 ) ;
#28432 = CARTESIAN_POINT ( 'NONE',  ( 12.72536390617885438, -2.839914339433650348, 24.50000000000000000 ) ) ;
#28433 = CARTESIAN_POINT ( 'NONE',  ( 5.009972004274191093, 16.26741710164063548, 6.782064869129510676 ) ) ;
#28434 = CARTESIAN_POINT ( 'NONE',  ( -33.42925964089140933, 11.06161099612212695, 35.54550565580014876 ) ) ;
#28435 = VERTEX_POINT ( 'NONE', #11279 ) ;
#28436 = CARTESIAN_POINT ( 'NONE',  ( -0.6573828633908636032, -19.98919327533018020, 19.47728749465737863 ) ) ;
#28437 = DIRECTION ( 'NONE',  ( -1.000000000000000000, 0.000000000000000000, 0.000000000000000000 ) ) ;
#28438 = CARTESIAN_POINT ( 'NONE',  ( 38.33765298566224544, 8.216851622513988929, 32.02327563374863928 ) ) ;
#28439 = CARTESIAN_POINT ( 'NONE',  ( 1.073881485057738949, 0.9711784013061123266, 1.500000000000000000 ) ) ;
#28440 = ORIENTED_EDGE ( 'NONE', *, *, #5540, .T. ) ;
#28441 = CIRCLE ( 'NONE', #8032, 9.000000000000000000 ) ;
#28442 = VECTOR ( 'NONE', #8375, 1000.000000000000000 ) ;
#28443 = CARTESIAN_POINT ( 'NONE',  ( -14.00715867683510751, 9.770345079980357283, 6.521906765011494578 ) ) ;
#28444 = FACE_OUTER_BOUND ( 'NONE', #837, .T. ) ;
#28445 =( BOUNDED_SURFACE ( )  B_SPLINE_SURFACE ( 3, 2, ( 
 ( #27725, #8699, #18057 ),
 ( #6356, #1980, #13840 ),
 ( #11501, #23021, #25386 ),
 ( #29753, #13541, #4014 ),
 ( #11187, #1371, #8399 ),
 ( #27426, #6507, #20684 ),
 ( #4308, #30211, #25221 ),
 ( #6044, #15553, #3715 ),
 ( #11350, #20844, #13229 ),
 ( #10886, #27574, #6200 ),
 ( #15703, #3865, #9299 ),
 ( #6969, #9465, #14123 ),
 ( #14597, #23948, #23483 ),
 ( #9615, #28493, #18825 ),
 ( #18980, #2271, #21132 ),
 ( #11792, #24103, #5087 ),
 ( #2751, #14272, #7120 ),
 ( #20985, #4764, #16632 ),
 ( #26136, #16939, #13986 ),
 ( #23792, #30504, #19274 ),
 ( #16327, #28793, #25995 ),
 ( #4931, #2443, #16478 ),
 ( #2122, #9151, #11964 ),
 ( #11641, #18665, #7432 ),
 ( #16778, #28342, #21298 ),
 ( #4622, #26456, #14447 ),
 ( #23627, #21454, #30818 ),
 ( #2595, #25846, #28170 ),
 ( #7266, #98, #19125 ),
 ( #28641, #26295, #12113 ),
 ( #30651, #21612, #247 ),
 ( #6803, #9759, #4478 ),
 ( #19582, #24714, #22390 ),
 ( #10220, #12890, #8051 ),
 ( #2909, #26771, #14741 ),
 ( #15358, #19432, #24886 ),
 ( #5545, #5856, #26928 ),
 ( #15192, #7901, #8196 ),
 ( #17087, #15047, #12260 ),
 ( #29564, #7586, #10534 ),
 ( #17243, #5243, #24562 ),
 ( #17701, #29100, #28950 ),
 ( #26615, #5399, #404 ),
 ( #862, #19730, #20042 ),
 ( #3206, #12728, #24259 ),
 ( #22225, #10386, #12425 ),
 ( #27071, #3357, #21920 ),
 ( #548, #29416, #22068 ),
 ( #29257, #24412, #19901 ),
 ( #21765, #10071, #17554 ),
 ( #1026, #7741, #5697 ),
 ( #27219, #14905, #9919 ),
 ( #3054, #17408, #12577 ),
 ( #704, #25031, #18025 ),
 ( #6472, #29884, #8807 ),
 ( #6621, #16134, #3525 ),
 ( #3822, #8524, #8969 ),
 ( #27538, #15983, #1179 ),
 ( #4127, #25504, #13506 ),
 ( #20187, #6162, #25343 ),
 ( #13346, #1326, #22988 ),
 ( #23139, #20801, #20359 ),
 ( #15665, #25177, #27988 ),
 ( #6008, #13656, #27389 ),
 ( #10848, #1786, #22675 ),
 ( #18484, #20652, #22528 ) ),
 .UNSPECIFIED., .F., .F., .T. ) 
 B_SPLINE_SURFACE_WITH_KNOTS ( ( 4, 2, 2, 2, 2, 2, 2, 2, 2, 2, 2, 2, 2, 2, 2, 2, 2, 2, 2, 2, 2, 2, 2, 2, 2, 2, 2, 2, 2, 2, 2, 2, 4 ),
 ( 3, 3 ),
 ( 0.000000000000000000, 0.006029285522234034342, 0.009043928283351050645, 0.01205857104446806868, 0.01507321380558508499, 0.01658053518614359401, 0.01808785656670210129, 0.02411714208893613737, 0.02562446346949464465, 0.02713178485005315194, 0.03014642761117016997, 0.03617571313340420258, 0.03919035589452121715, 0.04220499865563823866, 0.04521964141675526017, 0.04672696279731376745, 0.04823428417787227473, 0.05426356970010630387, 0.05727821246122331844, 0.05878553384178182573, 0.06029285522234033995, 0.06632214074457437603, 0.06933678350569139059, 0.07084410488624989788, 0.07235142626680840516, 0.07838071178904243430, 0.08139535455015944887, 0.08290267593071795615, 0.08440999731127647732, 0.09043928283351052033, 0.09194660421406902762, 0.09345392559462753490, 0.09646856835574454947 ),
 ( 0.000000000000000000, 1.000000000000000000 ),
 .UNSPECIFIED. ) 
 GEOMETRIC_REPRESENTATION_ITEM ( )  RATIONAL_B_SPLINE_SURFACE ( (
 ( 1.000000000000000000, 0.8675023601337629175, 1.000000000000000000),
 ( 1.000000000000000000, 0.8658666847259426369, 1.000000000000000000),
 ( 1.000000000000000000, 0.8655958742315080778, 1.000000000000000000),
 ( 1.000000000000000000, 0.8671900595434904879, 1.000000000000000000),
 ( 1.000000000000000000, 0.8680562056017228079, 1.000000000000000000),
 ( 1.000000000000000000, 0.8704419788917913126, 1.000000000000000000),
 ( 1.000000000000000000, 0.8719392239578002135, 1.000000000000000000),
 ( 1.000000000000000000, 0.8754638309335783797, 1.000000000000000000),
 ( 1.000000000000000000, 0.8774913221368225713, 1.000000000000000000),
 ( 1.000000000000000000, 0.8808764947177999405, 1.000000000000000000),
 ( 1.000000000000000000, 0.8820622495001770869, 1.000000000000000000),
 ( 1.000000000000000000, 0.8845398562658981501, 1.000000000000000000),
 ( 1.000000000000000000, 0.8858356588747311466, 1.000000000000000000),
 ( 1.000000000000000000, 0.8924978076758027790, 1.000000000000000000),
 ( 1.000000000000000000, 0.8984086608255127393, 1.000000000000000000),
 ( 1.000000000000000000, 0.9060753982733059653, 1.000000000000000000),
 ( 1.000000000000000000, 0.9076229079092951180, 1.000000000000000000),
 ( 1.000000000000000000, 0.9107356538043366312, 1.000000000000000000),
 ( 1.000000000000000000, 0.9123045924019421715, 1.000000000000000000),
 ( 1.000000000000000000, 0.9169824489404084789, 1.000000000000000000),
 ( 1.000000000000000000, 0.9200684232435814014, 1.000000000000000000),
 ( 1.000000000000000000, 0.9291119025149430222, 1.000000000000000000),
 ( 1.000000000000000000, 0.9348565328406341912, 1.000000000000000000),
 ( 1.000000000000000000, 0.9425865537118557347, 1.000000000000000000),
 ( 1.000000000000000000, 0.9449872438562321175, 1.000000000000000000),
 ( 1.000000000000000000, 0.9493613651927652608, 1.000000000000000000),
 ( 1.000000000000000000, 0.9513387435488267485, 1.000000000000000000),
 ( 1.000000000000000000, 0.9548238729109979062, 1.000000000000000000),
 ( 1.000000000000000000, 0.9563316464886052470, 1.000000000000000000),
 ( 1.000000000000000000, 0.9582033662281566055, 1.000000000000000000),
 ( 1.000000000000000000, 0.9587622799799166984, 1.000000000000000000),
 ( 1.000000000000000000, 0.9597437750956563374, 1.000000000000000000),
 ( 1.000000000000000000, 0.9601664819861042144, 1.000000000000000000),
 ( 1.000000000000000000, 0.9619094554756278947, 1.000000000000000000),
 ( 1.000000000000000000, 0.9621362728652917973, 1.000000000000000000),
 ( 1.000000000000000000, 0.9607577752117092418, 1.000000000000000000),
 ( 1.000000000000000000, 0.9600123908336705147, 1.000000000000000000),
 ( 1.000000000000000000, 0.9584744574991911348, 1.000000000000000000),
 ( 1.000000000000000000, 0.9578918694617124530, 1.000000000000000000),
 ( 1.000000000000000000, 0.9565886671613721415, 1.000000000000000000),
 ( 1.000000000000000000, 0.9558692645217879980, 1.000000000000000000),
 ( 1.000000000000000000, 0.9519759472186718474, 1.000000000000000000),
 ( 1.000000000000000000, 0.9478928039660258209, 1.000000000000000000),
 ( 1.000000000000000000, 0.9406739587686179238, 1.000000000000000000),
 ( 1.000000000000000000, 0.9380850758978200865, 1.000000000000000000),
 ( 1.000000000000000000, 0.9339721408369989764, 1.000000000000000000),
 ( 1.000000000000000000, 0.9325593384373154215, 1.000000000000000000),
 ( 1.000000000000000000, 0.9296829639154353675, 1.000000000000000000),
 ( 1.000000000000000000, 0.9282220600982826753, 1.000000000000000000),
 ( 1.000000000000000000, 0.9208300713421492256, 1.000000000000000000),
 ( 1.000000000000000000, 0.9146367548417139171, 1.000000000000000000),
 ( 1.000000000000000000, 0.9054116939033787226, 1.000000000000000000),
 ( 1.000000000000000000, 0.9023473709286883304, 1.000000000000000000),
 ( 1.000000000000000000, 0.8978322988697580165, 1.000000000000000000),
 ( 1.000000000000000000, 0.8963369152402574924, 1.000000000000000000),
 ( 1.000000000000000000, 0.8934211100373304903, 1.000000000000000000),
 ( 1.000000000000000000, 0.8919972686373036641, 1.000000000000000000),
 ( 1.000000000000000000, 0.8850723860929040621, 1.000000000000000000),
 ( 1.000000000000000000, 0.8801508607758546932, 1.000000000000000000),
 ( 1.000000000000000000, 0.8751780230577477226, 1.000000000000000000),
 ( 1.000000000000000000, 0.8742426755642516145, 1.000000000000000000),
 ( 1.000000000000000000, 0.8725019882397289095, 1.000000000000000000),
 ( 1.000000000000000000, 0.8716945872086134806, 1.000000000000000000),
 ( 1.000000000000000000, 0.8695096448583727877, 1.000000000000000000),
 ( 1.000000000000000000, 0.8683626000225895814, 1.000000000000000000),
 ( 1.000000000000000000, 0.8675417673879197711, 1.000000000000000000) ) ) 
 REPRESENTATION_ITEM ( '' )  SURFACE ( )  );
#28446 = CARTESIAN_POINT ( 'NONE',  ( -50.00000000000000000, 50.00000000000000000, 59.49999999999999289 ) ) ;
#28447 = EDGE_LOOP ( 'NONE', ( #5265, #10770, #30647, #30845 ) ) ;
#28448 = ADVANCED_FACE ( 'NONE', ( #16256 ), #22840, .T. ) ;
#28449 = ORIENTED_EDGE ( 'NONE', *, *, #29903, .F. ) ;
#28450 = ADVANCED_FACE ( 'NONE', ( #24503 ), #18120, .T. ) ;
#28451 = CARTESIAN_POINT ( 'NONE',  ( -31.22486525274646851, -15.32888848509419510, 35.97296397489743924 ) ) ;
#28452 = ADVANCED_FACE ( 'NONE', ( #4367 ), #1436, .F. ) ;
#28453 = ORIENTED_EDGE ( 'NONE', *, *, #12253, .T. ) ;
#28454 = ORIENTED_EDGE ( 'NONE', *, *, #10312, .T. ) ;
#28455 = CARTESIAN_POINT ( 'NONE',  ( -0.5107318660475972383, -20.01137538934480631, 19.87181966307587544 ) ) ;
#28456 = EDGE_CURVE ( 'NONE', #14399, #10610, #22797, .T. ) ;
#28457 = CARTESIAN_POINT ( 'NONE',  ( -8.423436389728856000, -14.82351904252669250, 7.643931100913408550 ) ) ;
#28458 = DIRECTION ( 'NONE',  ( 0.000000000000000000, 0.000000000000000000, -1.000000000000000000 ) ) ;
#28459 = CARTESIAN_POINT ( 'NONE',  ( 1.367976436446960209, -19.97081545247030476, 19.25672174529527325 ) ) ;
#28460 = EDGE_LOOP ( 'NONE', ( #3443, #28597, #5197, #17495, #1571, #6639 ) ) ;
#28461 = EDGE_CURVE ( 'NONE', #18599, #15417, #3888, .T. ) ;
#28462 = DIRECTION ( 'NONE',  ( 0.000000000000000000, 0.000000000000000000, -1.000000000000000000 ) ) ;
#28463 = DIRECTION ( 'NONE',  ( -0.000000000000000000, 1.000000000000000000, -0.000000000000000000 ) ) ;
#28464 = CARTESIAN_POINT ( 'NONE',  ( 14.52517991353747107, 13.77415465259964655, 18.50655187082627862 ) ) ;
#28465 = FACE_OUTER_BOUND ( 'NONE', #15159, .T. ) ;
#28466 = ADVANCED_FACE ( 'NONE', ( #22782 ), #13401, .T. ) ;
#28467 = ORIENTED_EDGE ( 'NONE', *, *, #29177, .T. ) ;
#28468 = VECTOR ( 'NONE', #9445, 1000.000000000000000 ) ;
#28469 = DIRECTION ( 'NONE',  ( 1.000000000000000000, 0.000000000000000000, 0.000000000000000000 ) ) ;
#28470 = DIRECTION ( 'NONE',  ( 0.000000000000000000, 0.000000000000000000, -1.000000000000000000 ) ) ;
#28471 = FACE_OUTER_BOUND ( 'NONE', #17721, .T. ) ;
#28472 = CARTESIAN_POINT ( 'NONE',  ( -18.15420570657826005, -8.392844156286328072, 18.37250658438898654 ) ) ;
#28473 = CARTESIAN_POINT ( 'NONE',  ( 33.36623411648999848, -9.470136927103574465, 36.07330332824747643 ) ) ;
#28474 = ORIENTED_EDGE ( 'NONE', *, *, #5920, .F. ) ;
#28475 = ORIENTED_EDGE ( 'NONE', *, *, #13014, .T. ) ;
#28476 = CARTESIAN_POINT ( 'NONE',  ( 7.869584159753955532, 10.39565510934977333, 24.50000000000000000 ) ) ;
#28477 = CARTESIAN_POINT ( 'NONE',  ( 31.18700685317242716, 26.11823559933198879, -1.500000000000000000 ) ) ;
#28478 = ADVANCED_FACE ( 'NONE', ( #30707 ), #14494, .F. ) ;
#28479 = CARTESIAN_POINT ( 'NONE',  ( 28.79137815760242702, -9.331429872129930914, -1.500000000000000000 ) ) ;
#28481 = CARTESIAN_POINT ( 'NONE',  ( -34.70577939416727276, 10.49309206033987785, 34.49999999999999289 ) ) ;
#28480 = VECTOR ( 'NONE', #8568, 1000.000000000000000 ) ;
#28482 = VERTEX_POINT ( 'NONE', #2642 ) ;
#28483 = CARTESIAN_POINT ( 'NONE',  ( 0.000000000000000000, 0.000000000000000000, 0.000000000000000000 ) ) ;
#28484 = CARTESIAN_POINT ( 'NONE',  ( -17.20435420003449423, -1.463329469628170898, 1.500000000000000000 ) ) ;
#28485 = CARTESIAN_POINT ( 'NONE',  ( 5.517068924551614906, 19.24285362756905471, 5.670038381137163519 ) ) ;
#28486 = EDGE_CURVE ( 'NONE', #15211, #2038, #29807, .T. ) ;
#28487 = ORIENTED_EDGE ( 'NONE', *, *, #27489, .T. ) ;
#28488 = FACE_OUTER_BOUND ( 'NONE', #14396, .T. ) ;
#28489 = ADVANCED_FACE ( 'NONE', ( #16525, #28391 ), #2327, .F. ) ;
#28490 = DIRECTION ( 'NONE',  ( 1.000000000000000000, 0.000000000000000000, 0.000000000000000000 ) ) ;
#28491 = VECTOR ( 'NONE', #29103, 1000.000000000000000 ) ;
#28492 = CARTESIAN_POINT ( 'NONE',  ( 9.749114229549594057, -0.1262659238204522361, 1.500000000000001332 ) ) ;
#28493 = CARTESIAN_POINT ( 'NONE',  ( -21.00291486166312183, 35.92820678882968366, 34.50839795287551937 ) ) ;
#28494 = ORIENTED_EDGE ( 'NONE', *, *, #10806, .F. ) ;
#28495 = DIRECTION ( 'NONE',  ( 0.000000000000000000, -0.000000000000000000, -1.000000000000000000 ) ) ;
#28496 = CYLINDRICAL_SURFACE ( 'NONE', #16517, 15.00000000000003375 ) ;
#28497 = CARTESIAN_POINT ( 'NONE',  ( -2.552544030762004645, -42.50000000000000000, -1.500000000000000000 ) ) ;
#28498 = EDGE_LOOP ( 'NONE', ( #1423, #20592, #22044, #19176 ) ) ;
#28499 = DIRECTION ( 'NONE',  ( -0.000000000000000000, -0.000000000000000000, 1.000000000000000000 ) ) ;
#28500 = LINE ( 'NONE', #21308, #16280 ) ;
#28501 = CARTESIAN_POINT ( 'NONE',  ( -0.2808233399669959884, -20.01605574108312524, 5.862424720655265098 ) ) ;
#28502 = CARTESIAN_POINT ( 'NONE',  ( 24.57973596967192265, -7.302173446879558938, 49.35895363830199045 ) ) ;
#28503 = CARTESIAN_POINT ( 'NONE',  ( 2.703030265324084080, -12.75514121382991384, 1.500000000000001332 ) ) ;
#28504 = CARTESIAN_POINT ( 'NONE',  ( 43.34097750826427387, 11.89502811014146033, -1.500000000000000000 ) ) ;
#28505 = DIRECTION ( 'NONE',  ( 0.000000000000000000, -1.132880637372608986E-16, 1.000000000000000000 ) ) ;
#28506 = ORIENTED_EDGE ( 'NONE', *, *, #25413, .F. ) ;
#28507 = CARTESIAN_POINT ( 'NONE',  ( -42.49999999999998579, 50.00000000000000000, 62.49999999999999289 ) ) ;
#28508 = AXIS2_PLACEMENT_3D ( 'NONE', #5359, #17521, #8168 ) ;
#28509 = LINE ( 'NONE', #9633, #16549 ) ;
#28510 = ORIENTED_EDGE ( 'NONE', *, *, #17391, .T. ) ;
#28511 = ORIENTED_EDGE ( 'NONE', *, *, #19304, .F. ) ;
#28512 = CARTESIAN_POINT ( 'NONE',  ( -15.95879822657219194, 12.05485308878816397, 6.919864475265776527 ) ) ;
#28513 = EDGE_CURVE ( 'NONE', #10973, #24160, #16275, .T. ) ;
#28514 = DIRECTION ( 'NONE',  ( 0.000000000000000000, 0.000000000000000000, 1.000000000000000000 ) ) ;
#28515 = EDGE_LOOP ( 'NONE', ( #25893, #7352, #19503, #19347 ) ) ;
#28516 = ADVANCED_FACE ( 'NONE', ( #6865 ), #6258, .F. ) ;
#28517 = PLANE ( 'NONE',  #5203 ) ;
#28518 = AXIS2_PLACEMENT_3D ( 'NONE', #4611, #28783, #14436 ) ;
#28519 = CARTESIAN_POINT ( 'NONE',  ( 0.000000000000000000, 0.000000000000000000, 1.500000000000000000 ) ) ;
#28520 = ORIENTED_EDGE ( 'NONE', *, *, #28852, .T. ) ;
#28521 = AXIS2_PLACEMENT_3D ( 'NONE', #19298, #16802, #18998 ) ;
#28522 = CARTESIAN_POINT ( 'NONE',  ( 18.68320837179354044, -7.186693706611503529, 18.82680253904184298 ) ) ;
#28523 = CARTESIAN_POINT ( 'NONE',  ( 16.56823697822719055, 4.133291823432034384, 19.69140814234746273 ) ) ;
#28524 = CARTESIAN_POINT ( 'NONE',  ( -25.41307773079511634, 6.523700759042264430, 48.76310947883596469 ) ) ;
#28525 = ORIENTED_EDGE ( 'NONE', *, *, #19110, .T. ) ;
#28526 = CARTESIAN_POINT ( 'NONE',  ( 15.47699552840392734, -7.094814489915346911, 18.72771030977187223 ) ) ;
#28527 = ORIENTED_EDGE ( 'NONE', *, *, #17061, .F. ) ;
#28528 = VERTEX_POINT ( 'NONE', #6570 ) ;
#28529 = LINE ( 'NONE', #28684, #16568 ) ;
#28530 = CARTESIAN_POINT ( 'NONE',  ( 3.863105514190048694E-15, -8.014718854569434114, -4.118099735505531100 ) ) ;
#28531 = CARTESIAN_POINT ( 'NONE',  ( 1.745046693156363071, -16.98705356654486209, 6.341840715582230281 ) ) ;
#28532 = CARTESIAN_POINT ( 'NONE',  ( -17.27847337688485396, -38.19802013284401454, 29.22704955593633613 ) ) ;
#28533 = CIRCLE ( 'NONE', #13619, 17.00000000000000000 ) ;
#28534 = CARTESIAN_POINT ( 'NONE',  ( -7.538175180318458679, -5.069257791428355198, 13.22130136205108819 ) ) ;
#28535 = FACE_BOUND ( 'NONE', #8576, .T. ) ;
#28536 = ORIENTED_EDGE ( 'NONE', *, *, #9979, .T. ) ;
#28537 = AXIS2_PLACEMENT_3D ( 'NONE', #15499, #20638, #27205 ) ;
#28538 = CARTESIAN_POINT ( 'NONE',  ( -16.95096719779282068, 1.761153487549138585, 18.35377592296120497 ) ) ;
#28539 = CARTESIAN_POINT ( 'NONE',  ( 18.35307960222155899, -7.992235168165439774, 5.652196082367003882 ) ) ;
#28540 = B_SPLINE_CURVE_WITH_KNOTS ( 'NONE', 3,
 ( #8817, #27544, #18343, #1795, #16142, #6172, #4277, #23308, #20950, #10855, #9117, #18639, #15524, #20365 ),
 .UNSPECIFIED., .F., .F.,
 ( 4, 2, 2, 2, 2, 2, 4 ),
 ( 2.108697328626194806E-07, 0.0004867403590529698022, 0.0009732698483730769980, 0.001459799337693184085, 0.001946328827013291390, 0.002919387805653492120, 0.003892446784293693285 ),
 .UNSPECIFIED. ) ;
#28541 = CARTESIAN_POINT ( 'NONE',  ( 20.47140833542507821, 26.57182937991349903, -16.50000000000000000 ) ) ;
#28542 = ORIENTED_EDGE ( 'NONE', *, *, #5062, .F. ) ;
#28543 = EDGE_LOOP ( 'NONE', ( #12776, #29017, #28188, #5190 ) ) ;
#28544 = CARTESIAN_POINT ( 'NONE',  ( 39.52380524533145945, -7.028748154382047808, -6.500000000000000888 ) ) ;
#28545 = CARTESIAN_POINT ( 'NONE',  ( -5.105024945673440229, 42.22604126506271882, -1.500000000000009992 ) ) ;
#28546 = B_SPLINE_CURVE_WITH_KNOTS ( 'NONE', 3,
 ( #7639, #17302, #15109, #27134 ),
 .UNSPECIFIED., .F., .F.,
 ( 4, 4 ),
 ( 2.143643656964904170E-07, 0.003421830178490233715 ),
 .UNSPECIFIED. ) ;
#28547 = DIRECTION ( 'NONE',  ( 0.000000000000000000, 0.000000000000000000, 1.000000000000000000 ) ) ;
#28548 = DIRECTION ( 'NONE',  ( -1.000000000000000000, 0.000000000000000000, 0.000000000000000000 ) ) ;
#28549 = DIRECTION ( 'NONE',  ( -1.000000000000000000, 0.000000000000000000, 0.000000000000000000 ) ) ;
#28550 = CARTESIAN_POINT ( 'NONE',  ( -33.04966240345561346, 15.66936333904344814, 27.50000000000001421 ) ) ;
#28551 = DIRECTION ( 'NONE',  ( -0.000000000000000000, 1.132880637372608986E-16, -1.000000000000000000 ) ) ;
#28552 = ORIENTED_EDGE ( 'NONE', *, *, #5034, .T. ) ;
#28553 = CARTESIAN_POINT ( 'NONE',  ( -11.01465109972504486, -37.62049097135311371, 34.49999999999999289 ) ) ;
#28554 = FACE_OUTER_BOUND ( 'NONE', #14083, .T. ) ;
#28555 = CARTESIAN_POINT ( 'NONE',  ( -24.03057240117690441, -26.57182937991348481, -1.500000000000001332 ) ) ;
#28556 = ORIENTED_EDGE ( 'NONE', *, *, #24195, .T. ) ;
#28557 = CARTESIAN_POINT ( 'NONE',  ( -4.937793815610304726, 6.974883619896852238, -1.500000000000000888 ) ) ;
#28558 = CIRCLE ( 'NONE', #26079, 20.00000000000000000 ) ;
#28559 = VERTEX_POINT ( 'NONE', #16382 ) ;
#28560 = CARTESIAN_POINT ( 'NONE',  ( -37.99999999999999289, 90.00000000000001421, -28.49999999999998934 ) ) ;
#28561 = AXIS2_PLACEMENT_3D ( 'NONE', #23858, #17148, #24323 ) ;
#28562 = UNCERTAINTY_MEASURE_WITH_UNIT (LENGTH_MEASURE( 1.000000000000000082E-05 ), #18067, 'distance_accuracy_value', 'NONE');
#28563 = CARTESIAN_POINT ( 'NONE',  ( -6.254902194515756797, 43.56090013333164279, -16.50000000000000000 ) ) ;
#28564 = ORIENTED_EDGE ( 'NONE', *, *, #23044, .T. ) ;
#28565 = CARTESIAN_POINT ( 'NONE',  ( 4.958664261655640892, 39.14709335570276494, 27.50000000000001066 ) ) ;
#28566 = CARTESIAN_POINT ( 'NONE',  ( 7.483314773547865784, 75.00000000000001421, 50.49999999999998579 ) ) ;
#28567 = CARTESIAN_POINT ( 'NONE',  ( 10.58714538945784867, -13.39479915613590499, 19.85459532544248162 ) ) ;
#28568 = CARTESIAN_POINT ( 'NONE',  ( 39.99999999999998579, 90.00000000000001421, 57.49999999999998579 ) ) ;
#28569 = LINE ( 'NONE', #4705, #3861 ) ;
#28570 = DIRECTION ( 'NONE',  ( -1.000000000000000000, 0.000000000000000000, 0.000000000000000000 ) ) ;
#28571 = VERTEX_POINT ( 'NONE', #8751 ) ;
#28572 = CARTESIAN_POINT ( 'NONE',  ( 15.40878509683846431, -7.233835689978969974, 6.973843882838225205 ) ) ;
#28573 = CIRCLE ( 'NONE', #24580, 9.482273699623480212 ) ;
#28574 = CARTESIAN_POINT ( 'NONE',  ( 34.07766914598172292, -21.40380666527112652, -1.500000000000000000 ) ) ;
#28575 = DIRECTION ( 'NONE',  ( -0.000000000000000000, 1.132880637372608986E-16, -1.000000000000000000 ) ) ;
#28576 = EDGE_CURVE ( 'NONE', #4502, #26722, #1038, .T. ) ;
#28577 = ORIENTED_EDGE ( 'NONE', *, *, #2777, .F. ) ;
#28578 = DIRECTION ( 'NONE',  ( -0.000000000000000000, -0.000000000000000000, 1.000000000000000000 ) ) ;
#28579 = VECTOR ( 'NONE', #17112, 1000.000000000000000 ) ;
#28580 = CARTESIAN_POINT ( 'NONE',  ( 7.974144905643786529, 5.130938270761634890, 13.00000000000000178 ) ) ;
#28581 = CARTESIAN_POINT ( 'NONE',  ( 20.47140833542507821, 26.57182937991349903, -6.500000000000000888 ) ) ;
#28582 = CIRCLE ( 'NONE', #7162, 9.084132297865673777 ) ;
#28583 = CARTESIAN_POINT ( 'NONE',  ( 4.989870534578006556, 16.27408959345230954, 6.385774490351134425 ) ) ;
#28584 = CARTESIAN_POINT ( 'NONE',  ( -33.48612972047447300, 10.91418318924902131, 35.53782825235610687 ) ) ;
#28585 = ORIENTED_EDGE ( 'NONE', *, *, #11116, .T. ) ;
#28586 = CARTESIAN_POINT ( 'NONE',  ( 0.2238118478526132105, -19.99918941848005005, 18.34726407865098707 ) ) ;
#28587 = FACE_OUTER_BOUND ( 'NONE', #25433, .T. ) ;
#28588 = CARTESIAN_POINT ( 'NONE',  ( 35.80460862680673273, 16.89914958172166237, 31.37043939660702563 ) ) ;
#28589 = ADVANCED_FACE ( 'NONE', ( #7177 ), #19179, .F. ) ;
#28590 = DIRECTION ( 'NONE',  ( 1.000000000000000000, 0.000000000000000000, 0.000000000000000000 ) ) ;
#28591 = VERTEX_POINT ( 'NONE', #24000 ) ;
#28592 = FACE_OUTER_BOUND ( 'NONE', #12006, .T. ) ;
#28593 = EDGE_LOOP ( 'NONE', ( #11729, #5145, #24340, #12132 ) ) ;
#28594 = CARTESIAN_POINT ( 'NONE',  ( 12.35522425158188931, 11.74279415389956327, 18.34798005863078885 ) ) ;
#28595 = CARTESIAN_POINT ( 'NONE',  ( -43.34097750826426676, 11.89502811014148698, 1.500000000000000444 ) ) ;
#28596 = ORIENTED_EDGE ( 'NONE', *, *, #13563, .T. ) ;
#28597 = ORIENTED_EDGE ( 'NONE', *, *, #16630, .F. ) ;
#28598 = CARTESIAN_POINT ( 'NONE',  ( 8.499586724479435418, 2.959227181723830036, 1.500000000000001332 ) ) ;
#28599 = VERTEX_POINT ( 'NONE', #2649 ) ;
#28600 = PRODUCT_DEFINITION_SHAPE ( 'NONE', 'NONE',  #3621 ) ;
#28601 = ORIENTED_EDGE ( 'NONE', *, *, #28801, .F. ) ;
#28602 = EDGE_LOOP ( 'NONE', ( #2255, #30692, #26126, #7071 ) ) ;
#28603 = CARTESIAN_POINT ( 'NONE',  ( -0.2861250491275360575, -20.01582202454545367, 20.12545155307891065 ) ) ;
#28604 = ADVANCED_FACE ( 'NONE', ( #11863 ), #21362, .F. ) ;
#28605 = CIRCLE ( 'NONE', #7182, 0.7500000000000006661 ) ;
#28606 = DIRECTION ( 'NONE',  ( 0.000000000000000000, 0.000000000000000000, 1.000000000000000000 ) ) ;
#28607 = DIRECTION ( 'NONE',  ( 0.000000000000000000, 1.132880637372608986E-16, -1.000000000000000000 ) ) ;
#28608 = CARTESIAN_POINT ( 'NONE',  ( -5.278755796068720585, -7.392982946727063798, 21.50000000000000000 ) ) ;
#28609 = ORIENTED_EDGE ( 'NONE', *, *, #19661, .F. ) ;
#28610 = CARTESIAN_POINT ( 'NONE',  ( 2.168404344971008868E-16, 42.50000000000000711, -1.500000000000000000 ) ) ;
#28611 = CARTESIAN_POINT ( 'NONE',  ( 22.94541271837968566, 35.03073867843525591, -6.499999999999999112 ) ) ;
#28612 = CARTESIAN_POINT ( 'NONE',  ( 14.19710122452049106, 14.11195047426184601, 19.25672174529527325 ) ) ;
#28613 = CARTESIAN_POINT ( 'NONE',  ( -10.47960520055065636, -7.757439966934454034, 1.500000000000001332 ) ) ;
#28614 = ORIENTED_EDGE ( 'NONE', *, *, #25767, .F. ) ;
#28615 = B_SPLINE_CURVE_WITH_KNOTS ( 'NONE', 3,
 ( #3646, #8639, #27659, #8948, #1911, #1759, #22965, #22819, #18464, #13160, #11275 ),
 .UNSPECIFIED., .F., .F.,
 ( 4, 1, 1, 1, 1, 1, 1, 1, 4 ),
 ( 0.000000000000000000, 0.3926990816987241395, 0.7853981633974482790, 1.178097245096172418, 1.570796326794896558, 1.963495408493620475, 2.356194490192344837, 2.748893571891068976, 3.141592653589793116 ),
 .UNSPECIFIED. ) ;
#28616 = DIRECTION ( 'NONE',  ( 0.000000000000000000, 1.000000000000000000, 0.000000000000000000 ) ) ;
#28617 = DIRECTION ( 'NONE',  ( -0.000000000000000000, -0.000000000000000000, -1.000000000000000000 ) ) ;
#28618 = LINE ( 'NONE', #7241, #20784 ) ;
#28619 = CARTESIAN_POINT ( 'NONE',  ( -19.92837724392305532, 1.693712106646815929, 7.272192800924334399 ) ) ;
#28620 = CARTESIAN_POINT ( 'NONE',  ( 19.76423196911359881, 3.064691114365036828, 7.652108011868850923 ) ) ;
#28621 = ADVANCED_FACE ( 'NONE', ( #1 ), #16690, .F. ) ;
#28622 = EDGE_CURVE ( 'NONE', #3110, #28626, #21666, .T. ) ;
#28623 = PLANE ( 'NONE',  #21883 ) ;
#28624 = DIRECTION ( 'NONE',  ( 1.000000000000000000, 0.000000000000000000, 0.000000000000000000 ) ) ;
#28625 = VERTEX_POINT ( 'NONE', #7022 ) ;
#28626 = VERTEX_POINT ( 'NONE', #23855 ) ;
#28627 = CARTESIAN_POINT ( 'NONE',  ( -10.47960520055065636, -7.757439966934454034, 24.50000000000000000 ) ) ;
#28628 = CARTESIAN_POINT ( 'NONE',  ( -10.11202017158466759, 41.14070756921185534, -1.500000000000000000 ) ) ;
#28629 = CARTESIAN_POINT ( 'NONE',  ( -14.72004833196315765, 13.56602982695842030, 6.974106381145714018 ) ) ;
#28630 = ADVANCED_FACE ( 'NONE', ( #12016 ), #7338, .F. ) ;
#28631 = CARTESIAN_POINT ( 'NONE',  ( 11.91798344328409875, -16.06126763266894386, 19.08830981656265280 ) ) ;
#28632 = ORIENTED_EDGE ( 'NONE', *, *, #18143, .F. ) ;
#28633 = PRODUCT_CONTEXT ( 'NONE', #28111, 'mechanical' ) ;
#28634 = CARTESIAN_POINT ( 'NONE',  ( 17.96497429814991875, -8.830595420483337676, 19.77662771831109367 ) ) ;
#28635 = CARTESIAN_POINT ( 'NONE',  ( 4.731053074881898191, 16.35701261131972473, 5.940635272151477686 ) ) ;
#28636 = EDGE_CURVE ( 'NONE', #20389, #17339, #10875, .T. ) ;
#28637 = ORIENTED_EDGE ( 'NONE', *, *, #6228, .T. ) ;
#28638 = CARTESIAN_POINT ( 'NONE',  ( 14.84769773172387630, 13.42619037096054413, 7.652108011868850035 ) ) ;
#28639 = ADVANCED_FACE ( 'NONE', ( #21190 ), #28354, .F. ) ;
#28640 = PLANE ( 'NONE',  #18818 ) ;
#28641 = CARTESIAN_POINT ( 'NONE',  ( -38.33685850190697408, 7.830772188364141684, 32.02836762638165169 ) ) ;
#28642 = ORIENTED_EDGE ( 'NONE', *, *, #20439, .T. ) ;
#28643 = CARTESIAN_POINT ( 'NONE',  ( -0.9307681286967859347, 9.436481611552762772, 13.00000000000000178 ) ) ;
#28644 = ADVANCED_FACE ( 'NONE', ( #11802 ), #20692, .F. ) ;
#28645 = CARTESIAN_POINT ( 'NONE',  ( 33.48319591361583036, 9.771272583783430221, 35.87764403311519601 ) ) ;
#28646 = CARTESIAN_POINT ( 'NONE',  ( 10.54213442295891667, 42.56985972894294434, -16.50000000000000711 ) ) ;
#28647 = ORIENTED_EDGE ( 'NONE', *, *, #28622, .F. ) ;
#28648 = CARTESIAN_POINT ( 'NONE',  ( -18.32390295431234861, -8.059524160852179264, 5.862424720655265098 ) ) ;
#28649 = AXIS2_PLACEMENT_3D ( 'NONE', #23906, #20796, #8965 ) ;
#28650 = DIRECTION ( 'NONE',  ( -0.000000000000000000, -0.000000000000000000, 1.000000000000000000 ) ) ;
#28651 = CARTESIAN_POINT ( 'NONE',  ( 14.79453494486352483, 13.45878767717418789, 7.652108011868850035 ) ) ;
#28652 = CARTESIAN_POINT ( 'NONE',  ( 0.2430132208050684306, -17.02994525543105908, 5.796888747622817029 ) ) ;
#28653 = FACE_OUTER_BOUND ( 'NONE', #6066, .T. ) ;
#28654 = CARTESIAN_POINT ( 'NONE',  ( -6.962021646281576714, -6.437683520590145037, 1.500000000000001332 ) ) ;
#28655 = CARTESIAN_POINT ( 'NONE',  ( 43.34097750826426676, -11.89502811014149941, -1.500000000000000000 ) ) ;
#28656 = CARTESIAN_POINT ( 'NONE',  ( 0.000000000000000000, 0.000000000000000000, -16.50000000000000000 ) ) ;
#28657 = EDGE_LOOP ( 'NONE', ( #23133, #23478, #726, #21819 ) ) ;
#28658 = EDGE_CURVE ( 'NONE', #26358, #12583, #30218, .T. ) ;
#28659 = ADVANCED_FACE ( 'NONE', ( #16177 ), #4168, .F. ) ;
#28660 = CARTESIAN_POINT ( 'NONE',  ( 11.55802067824463464, -16.34381896053850625, 20.19593175699879595 ) ) ;
#28661 = CYLINDRICAL_SURFACE ( 'NONE', #28521, 0.7500000000000006661 ) ;
#28662 = ORIENTED_EDGE ( 'NONE', *, *, #21943, .T. ) ;
#28663 = EDGE_CURVE ( 'NONE', #4676, #7304, #25691, .T. ) ;
#28664 = ORIENTED_EDGE ( 'NONE', *, *, #3506, .F. ) ;
#28665 = CARTESIAN_POINT ( 'NONE',  ( 69.99999999999998579, 50.00000000000000000, -92.50000000000000000 ) ) ;
#28666 = CARTESIAN_POINT ( 'NONE',  ( -10.94934520787159826, 48.78767624520369139, -65.26408404810210584 ) ) ;
#28667 = ADVANCED_FACE ( 'NONE', ( #8863 ), #4632, .F. ) ;
#28668 = CARTESIAN_POINT ( 'NONE',  ( 49.99999999999998579, -50.00000000000000000, 97.07879600563551037 ) ) ;
#28669 = VERTEX_POINT ( 'NONE', #4319 ) ;
#28670 = CARTESIAN_POINT ( 'NONE',  ( -4.163336342344337027E-14, -1.387778780781445676E-14, 1.500000000000000000 ) ) ;
#28671 = AXIS2_PLACEMENT_3D ( 'NONE', #15947, #25462, #21054 ) ;
#28672 = DIRECTION ( 'NONE',  ( -0.000000000000000000, -0.000000000000000000, -1.000000000000000000 ) ) ;
#28673 = EDGE_CURVE ( 'NONE', #6009, #7019, #25943, .T. ) ;
#28674 = VERTEX_POINT ( 'NONE', #11510 ) ;
#28675 = FACE_OUTER_BOUND ( 'NONE', #8760, .T. ) ;
#28676 = CARTESIAN_POINT ( 'NONE',  ( -15.66344362052393002, 12.43669181132025514, 20.22386025856689784 ) ) ;
#28677 = CARTESIAN_POINT ( 'NONE',  ( 25.10445388623454477, -25.60065097860747585, 1.500000000000000000 ) ) ;
#28678 = ORIENTED_EDGE ( 'NONE', *, *, #1232, .T. ) ;
#28679 = CARTESIAN_POINT ( 'NONE',  ( 15.76152542338162377, -6.481515897793713066, 18.34727598691068096 ) ) ;
#28680 = ORIENTED_EDGE ( 'NONE', *, *, #27657, .F. ) ;
#28681 = CIRCLE ( 'NONE', #1785, 9.000000000000000000 ) ;
#28682 = ORIENTED_EDGE ( 'NONE', *, *, #1036, .T. ) ;
#28683 = EDGE_CURVE ( 'NONE', #19990, #6231, #16832, .T. ) ;
#28684 = CARTESIAN_POINT ( 'NONE',  ( 69.99999999999998579, -70.00000000000000000, 12.49999999999999112 ) ) ;
#28685 = EDGE_CURVE ( 'NONE', #24319, #21410, #25544, .T. ) ;
#28686 = CARTESIAN_POINT ( 'NONE',  ( -26.36764545593177900, 31.31467416275353344, -1.500000000000000000 ) ) ;
#28687 = AXIS2_PLACEMENT_3D ( 'NONE', #38, #2538, #9408 ) ;
#28688 = FACE_OUTER_BOUND ( 'NONE', #28366, .T. ) ;
#28689 = FACE_OUTER_BOUND ( 'NONE', #7254, .T. ) ;
#28690 = FACE_BOUND ( 'NONE', #3820, .T. ) ;
#28691 = ORIENTED_EDGE ( 'NONE', *, *, #17924, .F. ) ;
#28692 = CARTESIAN_POINT ( 'NONE',  ( -19.83214989528428163, 2.722369515932096640, 18.36582235739946611 ) ) ;
#28693 = LINE ( 'NONE', #30418, #21702 ) ;
#28694 = VECTOR ( 'NONE', #23073, 1000.000000000000000 ) ;
#28695 = CARTESIAN_POINT ( 'NONE',  ( -13.37849590052435111, 10.56201291103764106, 7.652108011868850035 ) ) ;
#28696 = FACE_OUTER_BOUND ( 'NONE', #14432, .T. ) ;
#28697 = ORIENTED_EDGE ( 'NONE', *, *, #187, .F. ) ;
#28698 = ORIENTED_EDGE ( 'NONE', *, *, #12074, .T. ) ;
#28699 = CARTESIAN_POINT ( 'NONE',  ( 39.87350638640861433, 4.706224724276823146, -6.500000000000000888 ) ) ;
#28700 = CARTESIAN_POINT ( 'NONE',  ( -8.743977807160096205, -3.668292057955974350, 13.00000000000000178 ) ) ;
#28701 = CARTESIAN_POINT ( 'NONE',  ( 3.582389001540554840, -42.36371625716371625, 19.83486202640626672 ) ) ;
#28702 = DIRECTION ( 'NONE',  ( -1.000000000000000000, -0.000000000000000000, 0.000000000000000000 ) ) ;
#28703 = DIRECTION ( 'NONE',  ( -0.6548607339452852116, 0.7557495743542581579, 0.000000000000000000 ) ) ;
#28704 = VECTOR ( 'NONE', #6177, 1000.000000000000000 ) ;
#28705 = DIRECTION ( 'NONE',  ( 0.000000000000000000, 0.000000000000000000, -1.000000000000000000 ) ) ;
#28706 = CARTESIAN_POINT ( 'NONE',  ( -27.75715622479468081, 2.303929616531696922E-16, 1.500000000000001332 ) ) ;
#28707 = ORIENTED_EDGE ( 'NONE', *, *, #29217, .F. ) ;
#28708 = CARTESIAN_POINT ( 'NONE',  ( -34.70577939417217550, -10.49309206032214270, 34.49999999999999289 ) ) ;
#28709 = DIRECTION ( 'NONE',  ( -0.000000000000000000, -0.000000000000000000, -1.000000000000000000 ) ) ;
#28710 = DIRECTION ( 'NONE',  ( 0.000000000000000000, 0.000000000000000000, 1.000000000000000000 ) ) ;
#28711 = EDGE_LOOP ( 'NONE', ( #24376, #3521, #7548, #6861 ) ) ;
#28712 = CIRCLE ( 'NONE', #2294, 0.7499999999999997780 ) ;
#28713 = DIRECTION ( 'NONE',  ( 1.000000000000000000, 0.000000000000000000, 0.000000000000000000 ) ) ;
#28714 = VERTEX_POINT ( 'NONE', #13697 ) ;
#28715 = CARTESIAN_POINT ( 'NONE',  ( 15.81223571690236440, -6.365019318618790223, 7.652108011868850035 ) ) ;
#28716 = AXIS2_PLACEMENT_3D ( 'NONE', #18462, #27656, #27509 ) ;
#28717 = CARTESIAN_POINT ( 'NONE',  ( 49.99999999999998579, 50.00000000000000000, 12.49999999999999112 ) ) ;
#28718 = AXIS2_PLACEMENT_3D ( 'NONE', #17360, #26721, #15160 ) ;
#28719 = CARTESIAN_POINT ( 'NONE',  ( 14.88222593340887023, 13.36111339922579866, 7.652108011868850035 ) ) ;
#28720 = VERTEX_POINT ( 'NONE', #30516 ) ;
#28721 = CARTESIAN_POINT ( 'NONE',  ( 33.25228913575067224, 15.14457679224870823, 27.50000000000000711 ) ) ;
#28722 = CARTESIAN_POINT ( 'NONE',  ( 49.37858786280191481, 69.99072022605612631, 55.98525212243750815 ) ) ;
#28723 = DIRECTION ( 'NONE',  ( 1.000000000000000000, 0.000000000000000000, 0.000000000000000000 ) ) ;
#28724 = CARTESIAN_POINT ( 'NONE',  ( -18.44536497093016791, -7.731176935556637986, 6.386539667786092167 ) ) ;
#28725 = AXIS2_PLACEMENT_3D ( 'NONE', #6288, #30598, #30451 ) ;
#28726 = AXIS2_PLACEMENT_3D ( 'NONE', #27336, #972, #29362 ) ;
#28727 = DIRECTION ( 'NONE',  ( 0.000000000000000000, 0.000000000000000000, -1.000000000000000000 ) ) ;
#28728 = FACE_OUTER_BOUND ( 'NONE', #28447, .T. ) ;
#28729 = LINE ( 'NONE', #6895, #10877 ) ;
#28730 = EDGE_LOOP ( 'NONE', ( #19603, #15500, #21593, #26605 ) ) ;
#28731 = CARTESIAN_POINT ( 'NONE',  ( 7.500000000000000000, 0.000000000000000000, -6.600000000000001421 ) ) ;
#28732 = CIRCLE ( 'NONE', #18297, 1.447898107987198646 ) ;
#28733 = CARTESIAN_POINT ( 'NONE',  ( 2.552544030762014415, -42.50000000000000000, -1.500000000000000000 ) ) ;
#28734 = DIRECTION ( 'NONE',  ( 0.000000000000000000, 0.000000000000000000, 1.000000000000000000 ) ) ;
#28735 = EDGE_LOOP ( 'NONE', ( #22846, #21205, #28556, #27757 ) ) ;
#28736 = DIRECTION ( 'NONE',  ( -0.000000000000000000, -0.000000000000000000, -1.000000000000000000 ) ) ;
#28737 = LINE ( 'NONE', #28895, #26741 ) ;
#28738 = LINE ( 'NONE', #5027, #20197 ) ;
#28739 = AXIS2_PLACEMENT_3D ( 'NONE', #5411, #19742, #1037 ) ;
#28740 = CIRCLE ( 'NONE', #20282, 37.99999999999933920 ) ;
#28741 = CARTESIAN_POINT ( 'NONE',  ( -37.98493438988128901, 11.12428508575241004, -1.500000000000000000 ) ) ;
#28742 = EDGE_LOOP ( 'NONE', ( #22953, #29740, #23513, #15600 ) ) ;
#28743 = CARTESIAN_POINT ( 'NONE',  ( -4.163336342344337027E-14, -1.387778780781445676E-14, -1.500000000000000000 ) ) ;
#28744 = CARTESIAN_POINT ( 'NONE',  ( 28.40824562282756816, 24.48677906707029095, 37.49999999999575095 ) ) ;
#28745 = CARTESIAN_POINT ( 'NONE',  ( 7.500000000000000000, -5.196152422706639129, -9.000000000000000000 ) ) ;
#28746 = ORIENTED_EDGE ( 'NONE', *, *, #23070, .T. ) ;
#28747 = DIRECTION ( 'NONE',  ( -0.000000000000000000, 0.000000000000000000, 1.000000000000000000 ) ) ;
#28748 = ORIENTED_EDGE ( 'NONE', *, *, #9021, .F. ) ;
#28749 = VECTOR ( 'NONE', #25892, 1000.000000000000000 ) ;
#28750 = CARTESIAN_POINT ( 'NONE',  ( -23.72453467988983178, -12.99099554674205947, 43.70890687484121173 ) ) ;
#28751 = CARTESIAN_POINT ( 'NONE',  ( 0.000000000000000000, 0.000000000000000000, 1.500000000000001332 ) ) ;
#28752 = ORIENTED_EDGE ( 'NONE', *, *, #15458, .F. ) ;
#28753 = VERTEX_POINT ( 'NONE', #2131 ) ;
#28754 = LINE ( 'NONE', #19690, #13781 ) ;
#28755 = VECTOR ( 'NONE', #6544, 1000.000000000000000 ) ;
#28756 = EDGE_LOOP ( 'NONE', ( #8280, #5521, #12539, #21758 ) ) ;
#28757 = VERTEX_POINT ( 'NONE', #1835 ) ;
#28758 = CARTESIAN_POINT ( 'NONE',  ( 0.1433833641520081137, -17.02852539342428884, 20.12545155307891065 ) ) ;
#28759 = DIRECTION ( 'NONE',  ( 0.000000000000000000, 0.000000000000000000, 1.000000000000000000 ) ) ;
#28760 = CARTESIAN_POINT ( 'NONE',  ( 1.583371619456036994, -16.99707458536919802, 18.73743063545763121 ) ) ;
#28761 = EDGE_LOOP ( 'NONE', ( #16127, #6537, #9035, #24471 ) ) ;
#28762 = CARTESIAN_POINT ( 'NONE',  ( 31.31394823342230183, 25.51108937476774585, -1.500000000000003997 ) ) ;
#28763 = DIRECTION ( 'NONE',  ( -0.000000000000000000, -0.000000000000000000, 1.000000000000000000 ) ) ;
#28764 = CARTESIAN_POINT ( 'NONE',  ( 14.53258460577763067, 13.76634464516646972, 20.19593175699879595 ) ) ;
#28765 = PLANE ( 'NONE',  #27587 ) ;
#28766 = ORIENTED_EDGE ( 'NONE', *, *, #23604, .T. ) ;
#28767 = VECTOR ( 'NONE', #28117, 1000.000000000000000 ) ;
#28768 = AXIS2_PLACEMENT_3D ( 'NONE', #6486, #8679, #27861 ) ;
#28769 = PLANE ( 'NONE',  #937 ) ;
#28770 = CARTESIAN_POINT ( 'NONE',  ( -17.59999711780629283, -9.536506973003668008, 6.782048567692550378 ) ) ;
#28771 = CARTESIAN_POINT ( 'NONE',  ( -4.776122516674677878E-15, -42.50000000000000000, 27.50000000000000355 ) ) ;
#28772 = CARTESIAN_POINT ( 'NONE',  ( 5.881244434206234217, 6.812559277181991391, 21.50000000000000000 ) ) ;
#28773 = CARTESIAN_POINT ( 'NONE',  ( -70.00000000000000000, 50.00000000000000000, 12.49999999999999112 ) ) ;
#28774 = CARTESIAN_POINT ( 'NONE',  ( -15.17962487735951527, -7.751670534285732828, 18.34777357837151968 ) ) ;
#28775 = CARTESIAN_POINT ( 'NONE',  ( -32.19782014694307293, -14.25394737442115733, 35.54550565580014876 ) ) ;
#28776 = AXIS2_PLACEMENT_3D ( 'NONE', #7268, #26617, #16780 ) ;
#28777 = ORIENTED_EDGE ( 'NONE', *, *, #29642, .T. ) ;
#28778 = EDGE_LOOP ( 'NONE', ( #23552, #2081, #1415, #12480 ) ) ;
#28779 = AXIS2_PLACEMENT_3D ( 'NONE', #9469, #2913, #408 ) ;
#28780 = DIRECTION ( 'NONE',  ( 0.000000000000000000, 0.000000000000000000, 1.000000000000000000 ) ) ;
#28781 = DIRECTION ( 'NONE',  ( 0.000000000000000000, 0.000000000000000000, 1.000000000000000000 ) ) ;
#28782 = CARTESIAN_POINT ( 'NONE',  ( -12.72741959552008773, 11.30275801665550617, 6.864725433338323413 ) ) ;
#28783 = DIRECTION ( 'NONE',  ( -0.000000000000000000, -0.000000000000000000, -1.000000000000000000 ) ) ;
#28784 = ORIENTED_EDGE ( 'NONE', *, *, #26582, .F. ) ;
#28785 = CARTESIAN_POINT ( 'NONE',  ( 16.18505772754830119, -5.447928388648084486, 19.61324152429827095 ) ) ;
#28786 = DIRECTION ( 'NONE',  ( 0.000000000000000000, 0.000000000000000000, -1.000000000000000000 ) ) ;
#28787 = ORIENTED_EDGE ( 'NONE', *, *, #16224, .F. ) ;
#28788 = CARTESIAN_POINT ( 'NONE',  ( 4.270667257859590116, 16.49544336893744045, 20.32842677360128292 ) ) ;
#28789 = AXIS2_PLACEMENT_3D ( 'NONE', #7592, #14607, #2603 ) ;
#28790 = CARTESIAN_POINT ( 'NONE',  ( 11.99367014178017321, 12.13468339478709979, 7.500147780736496017 ) ) ;
#28791 = AXIS2_PLACEMENT_3D ( 'NONE', #16071, #27471, #20445 ) ;
#28792 = CARTESIAN_POINT ( 'NONE',  ( 19.54426622602687402, -37.07991288358297055, -1.499999999999999778 ) ) ;
#28793 = CARTESIAN_POINT ( 'NONE',  ( -29.63644584941609139, 27.66395999911765458, 34.56506848433971868 ) ) ;
#28794 = ORIENTED_EDGE ( 'NONE', *, *, #8848, .F. ) ;
#28795 = DIRECTION ( 'NONE',  ( 1.000000000000000000, 0.000000000000000000, 0.000000000000000000 ) ) ;
#28796 = EDGE_CURVE ( 'NONE', #8561, #19541, #18167, .T. ) ;
#28797 = EDGE_CURVE ( 'NONE', #25178, #5791, #6976, .T. ) ;
#28798 = DIRECTION ( 'NONE',  ( 1.000000000000000000, 0.000000000000000000, -0.000000000000000000 ) ) ;
#28799 = DIRECTION ( 'NONE',  ( 1.000000000000000000, 0.000000000000000000, 0.000000000000000000 ) ) ;
#28800 = VECTOR ( 'NONE', #29679, 1000.000000000000000 ) ;
#28801 = EDGE_CURVE ( 'NONE', #25490, #18893, #558, .T. ) ;
#28802 = ORIENTED_EDGE ( 'NONE', *, *, #19112, .F. ) ;
#28803 = AXIS2_PLACEMENT_3D ( 'NONE', #26584, #363, #7552 ) ;
#28804 = CARTESIAN_POINT ( 'NONE',  ( -18.39183130958318557, -7.903152449895378240, 7.272049892295485485 ) ) ;
#28805 = EDGE_CURVE ( 'NONE', #18778, #28122, #24419, .T. ) ;
#28806 = DIRECTION ( 'NONE',  ( 0.000000000000000000, 0.000000000000000000, -1.000000000000000000 ) ) ;
#28807 = EDGE_CURVE ( 'NONE', #6600, #5146, #7377, .T. ) ;
#28808 = LINE ( 'NONE', #5253, #30697 ) ;
#28809 = DIRECTION ( 'NONE',  ( 0.000000000000000000, 0.000000000000000000, 1.000000000000000000 ) ) ;
#28810 = CYLINDRICAL_SURFACE ( 'NONE', #12319, 50.00000000000000000 ) ;
#28811 = CARTESIAN_POINT ( 'NONE',  ( 36.60626274880365116, -14.67294879964692278, 9.537266162416086601 ) ) ;
#28812 = DIRECTION ( 'NONE',  ( -0.000000000000000000, -0.000000000000000000, 1.000000000000000000 ) ) ;
#28813 = VERTEX_POINT ( 'NONE', #7442 ) ;
#28814 = CIRCLE ( 'NONE', #17848, 3.559164065751841743 ) ;
#28815 = ADVANCED_FACE ( 'NONE', ( #26781, #5409 ), #16789, .F. ) ;
#28816 = AXIS2_PLACEMENT_3D ( 'NONE', #3643, #8497, #677 ) ;
#28817 = CARTESIAN_POINT ( 'NONE',  ( -6.045292009791579879, 15.95527889494839968, 7.545655578832111132 ) ) ;
#28818 = LINE ( 'NONE', #268, #2621 ) ;
#28819 = ADVANCED_FACE ( 'NONE', ( #19282 ), #7131, .T. ) ;
#28820 = AXIS2_PLACEMENT_3D ( 'NONE', #8066, #10552, #1196 ) ;
#28821 = ORIENTED_EDGE ( 'NONE', *, *, #27863, .T. ) ;
#28822 = ORIENTED_EDGE ( 'NONE', *, *, #8469, .T. ) ;
#28823 = ADVANCED_FACE ( 'NONE', ( #12586 ), #10078, .T. ) ;
#28824 = LINE ( 'NONE', #27098, #3180 ) ;
#28825 = CARTESIAN_POINT ( 'NONE',  ( 28.34828976096172681, 29.18752572968383419, 1.500000000000000000 ) ) ;
#28826 = ORIENTED_EDGE ( 'NONE', *, *, #14035, .T. ) ;
#28827 = DIRECTION ( 'NONE',  ( -0.000000000000000000, 0.000000000000000000, 1.000000000000000000 ) ) ;
#28828 = CYLINDRICAL_SURFACE ( 'NONE', #993, 12.66227964008302287 ) ;
#28829 = EDGE_LOOP ( 'NONE', ( #27823, #29251, #17540, #486 ) ) ;
#28830 = CARTESIAN_POINT ( 'NONE',  ( 18.62671295915898639, -7.331958482175751968, 20.06253562465620632 ) ) ;
#28831 = CARTESIAN_POINT ( 'NONE',  ( -15.89566665641789456, 12.13797781250046626, 19.85730954408919047 ) ) ;
#28832 = DIRECTION ( 'NONE',  ( 0.000000000000000000, 1.000000000000000000, 0.000000000000000000 ) ) ;
#28833 = ORIENTED_EDGE ( 'NONE', *, *, #2266, .F. ) ;
#28834 = DIRECTION ( 'NONE',  ( 0.000000000000000000, 0.000000000000000000, 1.000000000000000000 ) ) ;
#28835 = ADVANCED_FACE ( 'NONE', ( #2760 ), #19591, .F. ) ;
#28836 = VERTEX_POINT ( 'NONE', #22077 ) ;
#28837 = DIRECTION ( 'NONE',  ( -0.000000000000000000, -1.000000000000000000, 0.000000000000000000 ) ) ;
#28838 = ADVANCED_FACE ( 'NONE', ( #26144 ), #21620, .F. ) ;
#28839 = EDGE_CURVE ( 'NONE', #28714, #11459, #6899, .T. ) ;
#28840 = VECTOR ( 'NONE', #5957, 1000.000000000000114 ) ;
#28841 = EDGE_LOOP ( 'NONE', ( #11588, #2910, #5882, #8453, #961, #20933 ) ) ;
#28842 = EDGE_CURVE ( 'NONE', #19044, #2106, #15355, .T. ) ;
#28843 = CARTESIAN_POINT ( 'NONE',  ( 28.97452988725117962, 28.45570922648237300, 30.21020218777692889 ) ) ;
#28844 = CARTESIAN_POINT ( 'NONE',  ( 49.99999999999998579, -70.00000000000000000, 12.49999999999999112 ) ) ;
#28845 = CIRCLE ( 'NONE', #1921, 2.898871837527149609 ) ;
#28846 = CARTESIAN_POINT ( 'NONE',  ( -7.796062812047480861, -15.18940472835274669, 18.82680253904184298 ) ) ;
#28847 = ADVANCED_FACE ( 'NONE', ( #26623 ), #17096, .F. ) ;
#28848 = CYLINDRICAL_SURFACE ( 'NONE', #16512, 9.482273699623480212 ) ;
#28849 = LINE ( 'NONE', #3414, #18012 ) ;
#28850 = DIRECTION ( 'NONE',  ( 1.000000000000000000, 0.000000000000000000, -0.000000000000000000 ) ) ;
#28851 = EDGE_LOOP ( 'NONE', ( #5108, #10376 ) ) ;
#28852 = EDGE_CURVE ( 'NONE', #12760, #10675, #17771, .T. ) ;
#28853 = FACE_OUTER_BOUND ( 'NONE', #24735, .T. ) ;
#28854 = CARTESIAN_POINT ( 'NONE',  ( -28.00567590795085238, 29.57774132268513512, 12.52310953214416323 ) ) ;
#28855 = DIRECTION ( 'NONE',  ( -0.000000000000000000, -0.000000000000000000, 1.000000000000000000 ) ) ;
#28856 = CARTESIAN_POINT ( 'NONE',  ( 57.49999999999998579, 50.00000000000000000, 12.49999999999999112 ) ) ;
#28857 = EDGE_LOOP ( 'NONE', ( #30680, #28428, #11881, #27147, #30110, #665, #21946, #8797, #20546 ) ) ;
#28858 = VERTEX_POINT ( 'NONE', #19740 ) ;
#28859 = B_SPLINE_CURVE_WITH_KNOTS ( 'NONE', 3,
 ( #18283, #21053, #1738, #27804, #6430, #15946, #4086, #13614, #18589, #20909, #9072, #23094, #18732, #28100, #13901, #16696, #17313, #10136 ),
 .UNSPECIFIED., .F., .F.,
 ( 4, 2, 2, 2, 2, 2, 2, 2, 4 ),
 ( 0.000000000000000000, 0.0003967869494442877220, 0.0007935738988885754439, 0.001190360848332863274, 0.001587147797777150888, 0.001983934747221438501, 0.002380721696665726549, 0.002777508646110014162, 0.003174295595554301776 ),
 .UNSPECIFIED. ) ;
#28860 = CARTESIAN_POINT ( 'NONE',  ( -39.87808514257974224, -7.028748160228998287, -14.83333104093387611 ) ) ;
#28861 = DIRECTION ( 'NONE',  ( -0.000000000000000000, -0.000000000000000000, 1.000000000000000000 ) ) ;
#28862 = PRODUCT_DEFINITION_SHAPE ( 'NONE', 'NONE',  #7631 ) ;
#28863 = CARTESIAN_POINT ( 'NONE',  ( -5.450136891332532763, 19.26184010647175882, 7.500898271101006820 ) ) ;
#28864 = CARTESIAN_POINT ( 'NONE',  ( -15.57492749417239253, -6.866608492817582565, 6.782064869129510676 ) ) ;
#28865 = CARTESIAN_POINT ( 'NONE',  ( -3.395021109945006721, -30.50000000000000711, 24.50000000000000000 ) ) ;
#28866 = EDGE_CURVE ( 'NONE', #21892, #26251, #10396, .T. ) ;
#28867 = ORIENTED_EDGE ( 'NONE', *, *, #13732, .F. ) ;
#28868 = EDGE_CURVE ( 'NONE', #14320, #3020, #3914, .T. ) ;
#28869 = ORIENTED_EDGE ( 'NONE', *, *, #29811, .F. ) ;
#28870 = CARTESIAN_POINT ( 'NONE',  ( 0.000000000000000000, 9.084132297865670225, 27.94260272410217638 ) ) ;
#28871 = CIRCLE ( 'NONE', #12423, 0.7500000000000006661 ) ;
#28872 = CARTESIAN_POINT ( 'NONE',  ( -17.76782356872499946, -9.182228809334535669, 20.15039051365864253 ) ) ;
#28873 = DIRECTION ( 'NONE',  ( 0.000000000000000000, 0.000000000000000000, 1.000000000000000000 ) ) ;
#28874 = ORIENTED_EDGE ( 'NONE', *, *, #14434, .F. ) ;
#28875 = CARTESIAN_POINT ( 'NONE',  ( 12.35846532919128826, 11.73919094318043577, 7.652108011868850035 ) ) ;
#28876 = ORIENTED_EDGE ( 'NONE', *, *, #12606, .T. ) ;
#28877 = CARTESIAN_POINT ( 'NONE',  ( 18.52307105101189677, -7.590397700845933571, 7.559636331181775581 ) ) ;
#28878 = CYLINDRICAL_SURFACE ( 'NONE', #11378, 1.999999999999998224 ) ;
#28879 = AXIS2_PLACEMENT_3D ( 'NONE', #15592, #27151, #24955 ) ;
#28880 = CYLINDRICAL_SURFACE ( 'NONE', #27992, 0.7500000000000002220 ) ;
#28881 = EDGE_CURVE ( 'NONE', #4157, #29398, #23809, .T. ) ;
#28882 = ORIENTED_EDGE ( 'NONE', *, *, #6403, .T. ) ;
#28883 = CARTESIAN_POINT ( 'NONE',  ( 3.826954525806324448, 16.61697297626112046, 5.678370764302467677 ) ) ;
#28884 = DIRECTION ( 'NONE',  ( 0.000000000000000000, 0.000000000000000000, -1.000000000000000000 ) ) ;
#28885 = LINE ( 'NONE', #8286, #1376 ) ;
#28886 = CARTESIAN_POINT ( 'NONE',  ( -18.15420570657826360, -8.392844156286336954, 5.676722608126685721 ) ) ;
#28887 = DIRECTION ( 'NONE',  ( 1.000000000000000000, 0.000000000000000000, 0.000000000000000000 ) ) ;
#28888 = CARTESIAN_POINT ( 'NONE',  ( 29.61203839202722676, 15.40012917324034092, 41.62281023987512185 ) ) ;
#28889 = EDGE_LOOP ( 'NONE', ( #17539, #13453, #29555, #12391 ) ) ;
#28890 = CARTESIAN_POINT ( 'NONE',  ( 19.54426622602689179, 37.07991288358296345, 1.499999999999999778 ) ) ;
#28891 = AXIS2_PLACEMENT_3D ( 'NONE', #9109, #27985, #23587 ) ;
#28892 = CARTESIAN_POINT ( 'NONE',  ( 10.64374042650304020, -42.96126232887725394, -19.50000000000000355 ) ) ;
#28893 = DIRECTION ( 'NONE',  ( -0.000000000000000000, 0.000000000000000000, -1.000000000000000000 ) ) ;
#28894 = ORIENTED_EDGE ( 'NONE', *, *, #20284, .F. ) ;
#28895 = CARTESIAN_POINT ( 'NONE',  ( -12.72536390617885260, -2.839914339433650348, 24.50000000000000000 ) ) ;
#28896 = DIRECTION ( 'NONE',  ( -1.000000000000000000, 0.000000000000000000, 0.000000000000000000 ) ) ;
#28897 = DIRECTION ( 'NONE',  ( -0.000000000000000000, -0.000000000000000000, 1.000000000000000000 ) ) ;
#28898 = CIRCLE ( 'NONE', #7479, 9.084132297865673777 ) ;
#28899 = CARTESIAN_POINT ( 'NONE',  ( -25.19442432475474902, -35.44676296258422354, -19.50000000000000355 ) ) ;
#28900 = CYLINDRICAL_SURFACE ( 'NONE', #5931, 0.7500000000000002220 ) ;
#28901 = CARTESIAN_POINT ( 'NONE',  ( 33.58313301488747271, 16.73358698008457424, 37.50000000006255618 ) ) ;
#28902 = EDGE_CURVE ( 'NONE', #29503, #12213, #17709, .T. ) ;
#28903 = CARTESIAN_POINT ( 'NONE',  ( 0.000000000000000000, 1.699320956058915452E-16, -1.500000000000001776 ) ) ;
#28904 = VERTEX_POINT ( 'NONE', #29723 ) ;
#28905 = CARTESIAN_POINT ( 'NONE',  ( 32.93066664481101924, -23.11087910253144528, -3.166603179814984959 ) ) ;
#28906 = ORIENTED_EDGE ( 'NONE', *, *, #20517, .F. ) ;
#28907 = DIRECTION ( 'NONE',  ( 1.000000000000000000, 0.000000000000000000, 0.000000000000000000 ) ) ;
#28908 = DIRECTION ( 'NONE',  ( -0.000000000000000000, -0.000000000000000000, 1.000000000000000000 ) ) ;
#28909 = ORIENTED_EDGE ( 'NONE', *, *, #3282, .F. ) ;
#28910 = ORIENTED_EDGE ( 'NONE', *, *, #5949, .T. ) ;
#28911 = CARTESIAN_POINT ( 'NONE',  ( -9.636724589035630117, -17.52522580332708202, 6.788986777570690023 ) ) ;
#28912 = ORIENTED_EDGE ( 'NONE', *, *, #15478, .T. ) ;
#28913 = AXIS2_PLACEMENT_3D ( 'NONE', #18734, #13616, #23097 ) ;
#28914 = EDGE_LOOP ( 'NONE', ( #14047, #3550 ) ) ;
#28915 = ORIENTED_EDGE ( 'NONE', *, *, #7895, .T. ) ;
#28916 = CARTESIAN_POINT ( 'NONE',  ( -0.2229293267576271109, -17.01997447887395509, 19.22654678686458141 ) ) ;
#28917 = CARTESIAN_POINT ( 'NONE',  ( -25.23650299772496197, 28.24517122938463842, 34.50000000000000000 ) ) ;
#28918 = CARTESIAN_POINT ( 'NONE',  ( -9.702532784345955008, -17.50903092980014009, 6.995624166085161910 ) ) ;
#28919 = CARTESIAN_POINT ( 'NONE',  ( 4.172444469959711633, 16.52351170757476950, 18.34727598691068096 ) ) ;
#28920 = CARTESIAN_POINT ( 'NONE',  ( 0.9820204223201484117, -19.99380624802880035, 20.13759033520874908 ) ) ;
#28921 = ORIENTED_EDGE ( 'NONE', *, *, #28945, .F. ) ;
#28922 = FACE_OUTER_BOUND ( 'NONE', #10072, .T. ) ;
#28923 = CARTESIAN_POINT ( 'NONE',  ( 19.82873939126788443, -38.47025822325555566, -16.50000000000000355 ) ) ;
#28924 = CARTESIAN_POINT ( 'NONE',  ( 0.3518703668723784928, -19.99690444156084723, 20.34789198813115263 ) ) ;
#28925 = DIRECTION ( 'NONE',  ( 1.000000000000000000, 0.000000000000000000, 0.000000000000000000 ) ) ;
#28926 = ORIENTED_EDGE ( 'NONE', *, *, #18064, .T. ) ;
#28927 = CARTESIAN_POINT ( 'NONE',  ( -8.840471615930058036, 1.687027447297517080, -3.621320343559650379 ) ) ;
#28928 = CARTESIAN_POINT ( 'NONE',  ( -17.62281152098609027, -9.494300025206930727, 6.341840715582230281 ) ) ;
#28929 = CARTESIAN_POINT ( 'NONE',  ( -6.294089901980526314, 15.86740633010675516, 7.280727868105637768 ) ) ;
#28930 = CARTESIAN_POINT ( 'NONE',  ( -19.94291556179615910, 1.510882595598290079, 6.392525840300333329 ) ) ;
#28931 = CARTESIAN_POINT ( 'NONE',  ( 0.3593302862868671399, 3.504574740656557275, 9.000000000000003553 ) ) ;
#28932 = AXIS2_PLACEMENT_3D ( 'NONE', #28058, #30094, #30403 ) ;
#28933 = CARTESIAN_POINT ( 'NONE',  ( -6.974883619896829146, -5.687793815610328707, -3.621320343559650379 ) ) ;
#28934 = B_SPLINE_CURVE_WITH_KNOTS ( 'NONE', 3,
 ( #28610, #9888, #30624, #11935, #18953, #26427, #21259, #26260, #28762, #16592 ),
 .UNSPECIFIED., .F., .F.,
 ( 4, 2, 2, 2, 4 ),
 ( 0.1275862231236772337, 0.1353932202260588469, 0.1432002173284404600, 0.1588142115332036863, 0.1673618661614010295 ),
 .UNSPECIFIED. ) ;
#28935 = VERTEX_POINT ( 'NONE', #20198 ) ;
#28936 = ORIENTED_EDGE ( 'NONE', *, *, #30198, .T. ) ;
#28937 = DIRECTION ( 'NONE',  ( -0.8910248307962436165, -0.4539545692076746852, 0.000000000000000000 ) ) ;
#28938 = VECTOR ( 'NONE', #22340, 1000.000000000000000 ) ;
#28939 = CARTESIAN_POINT ( 'NONE',  ( 10.64374042650142904, 42.96126232887663576, -19.50000000000000355 ) ) ;
#28940 = DIRECTION ( 'NONE',  ( -1.000000000000000000, 0.000000000000000000, 0.000000000000000000 ) ) ;
#28941 = CARTESIAN_POINT ( 'NONE',  ( 0.5152247662762403646, -17.03071091119059233, 7.626437579292365321 ) ) ;
#28942 = VERTEX_POINT ( 'NONE', #6018 ) ;
#28943 = APPLICATION_PROTOCOL_DEFINITION ( 'draft international standard', 'automotive_design', 1998, #13759 ) ;
#28944 = CARTESIAN_POINT ( 'NONE',  ( 5.881244434206234217, 6.812559277181991391, 21.50000000000000000 ) ) ;
#28945 = EDGE_CURVE ( 'NONE', #18617, #12232, #10384, .T. ) ;
#28946 = CARTESIAN_POINT ( 'NONE',  ( -8.072557715923444732, 14.41080185948837311, -0.6213203435596476032 ) ) ;
#28947 = ORIENTED_EDGE ( 'NONE', *, *, #8876, .F. ) ;
#28948 = CYLINDRICAL_SURFACE ( 'NONE', #28173, 7.500000000000000000 ) ;
#28949 = DIRECTION ( 'NONE',  ( 1.000000000000000000, 0.000000000000000000, 0.000000000000000000 ) ) ;
#28950 = CARTESIAN_POINT ( 'NONE',  ( -35.18685215751978745, -13.22180849084768006, 37.49999999986729193 ) ) ;
#28951 = ORIENTED_EDGE ( 'NONE', *, *, #22693, .F. ) ;
#28952 = CARTESIAN_POINT ( 'NONE',  ( -6.630478080506957639, -6.778663211761441154, 13.00000000000000178 ) ) ;
#28953 = DIRECTION ( 'NONE',  ( -0.000000000000000000, -0.000000000000000000, -1.000000000000000000 ) ) ;
#28954 = CARTESIAN_POINT ( 'NONE',  ( -10.11202017158235833, -41.14070756921188377, -1.500000000000000000 ) ) ;
#28955 = ORIENTED_EDGE ( 'NONE', *, *, #27404, .F. ) ;
#28956 = CARTESIAN_POINT ( 'NONE',  ( -18.43827498451961944, -7.794211480880298915, 7.080843742048788414 ) ) ;
#28957 = DIRECTION ( 'NONE',  ( 1.000000000000000000, 0.000000000000000000, 0.000000000000000000 ) ) ;
#28958 = DIRECTION ( 'NONE',  ( -0.000000000000000000, -0.000000000000000000, -1.000000000000000000 ) ) ;
#28959 = CARTESIAN_POINT ( 'NONE',  ( -0.2229293267576251125, -17.01997447887395509, 6.530762810602277924 ) ) ;
#28960 = DIRECTION ( 'NONE',  ( -0.000000000000000000, -1.000000000000000000, -0.000000000000000000 ) ) ;
#28961 = DIRECTION ( 'NONE',  ( 1.000000000000000000, 0.000000000000000000, 0.000000000000000000 ) ) ;
#28962 = CARTESIAN_POINT ( 'NONE',  ( 37.98476534559758733, -9.634081485176503534, 12.75486969068182397 ) ) ;
#28963 = DIRECTION ( 'NONE',  ( -1.000000000000000000, 0.000000000000000000, 0.000000000000000000 ) ) ;
#28964 = EDGE_LOOP ( 'NONE', ( #13305, #12505 ) ) ;
#28965 = AXIS2_PLACEMENT_3D ( 'NONE', #26311, #9477, #12125 ) ;
#28966 = DIRECTION ( 'NONE',  ( -1.000000000000000000, 0.000000000000000000, 0.000000000000000000 ) ) ;
#28967 = CARTESIAN_POINT ( 'NONE',  ( -70.00000000000000000, -65.00000000000000000, 57.49999999999999289 ) ) ;
#28968 = ORIENTED_EDGE ( 'NONE', *, *, #2144, .F. ) ;
#28969 = EDGE_LOOP ( 'NONE', ( #4707, #10645, #11223 ) ) ;
#28970 = EDGE_CURVE ( 'NONE', #26160, #16362, #13309, .T. ) ;
#28971 = CARTESIAN_POINT ( 'NONE',  ( 3.637110358602582583, 19.99473753024312117, 1.500000000000000000 ) ) ;
#28973 = CARTESIAN_POINT ( 'NONE',  ( -11.91668235487185257, 48.56246597984248581, -45.83682539780265586 ) ) ;
#28972 = PRODUCT_RELATED_PRODUCT_CATEGORY ( 'part', '', ( #21363 ) ) ;
#28974 = VERTEX_POINT ( 'NONE', #8675 ) ;
#28975 = CARTESIAN_POINT ( 'NONE',  ( 15.25015041412931183, 12.96756205105604920, 18.49267272388512140 ) ) ;
#28976 = CARTESIAN_POINT ( 'NONE',  ( -10.97902775627723493, -16.73874854128740353, 5.796888747622817029 ) ) ;
#28977 = ORIENTED_EDGE ( 'NONE', *, *, #30202, .T. ) ;
#28978 = EDGE_CURVE ( 'NONE', #3062, #19423, #1913, .T. ) ;
#28979 = CARTESIAN_POINT ( 'NONE',  ( 31.92585768969536630, 26.59981599185444878, -13.16665969302820471 ) ) ;
#28980 = CARTESIAN_POINT ( 'NONE',  ( 19.73572331631237731, 3.349230485916621980, 18.35718225375110180 ) ) ;
#28981 = CARTESIAN_POINT ( 'NONE',  ( 37.99999999999999289, 209.2686044187655909, -81.50000000000001421 ) ) ;
#28982 = ORIENTED_EDGE ( 'NONE', *, *, #27181, .F. ) ;
#28983 = CARTESIAN_POINT ( 'NONE',  ( 15.60593903839447982, -6.823719261784396473, 18.47056384035244037 ) ) ;
#28984 = ORIENTED_EDGE ( 'NONE', *, *, #11138, .T. ) ;
#28985 = CIRCLE ( 'NONE', #9063, 0.7441270634456955690 ) ;
#28986 = ORIENTED_EDGE ( 'NONE', *, *, #8452, .F. ) ;
#28987 = EDGE_CURVE ( 'NONE', #25828, #7554, #18493, .T. ) ;
#28988 = CARTESIAN_POINT ( 'NONE',  ( -6.670428619809866788, 18.87372120578244150, 18.64703902303423178 ) ) ;
#28989 = DIRECTION ( 'NONE',  ( -0.000000000000000000, 0.000000000000000000, 1.000000000000000000 ) ) ;
#28990 = AXIS2_PLACEMENT_3D ( 'NONE', #7983, #7811, #5477 ) ;
#28991 = CARTESIAN_POINT ( 'NONE',  ( -7.685008110482988819, -15.25093183970989763, 19.14333282897057842 ) ) ;
#28992 = DIRECTION ( 'NONE',  ( -0.3598999890241648680, -0.9329908884337543284, 0.000000000000000000 ) ) ;
#28993 = LINE ( 'NONE', #9976, #5529 ) ;
#28994 = CARTESIAN_POINT ( 'NONE',  ( 6.900000000000000355, -1.502314598737158242E-15, -9.000000000000001776 ) ) ;
#28995 = ORIENTED_EDGE ( 'NONE', *, *, #23501, .F. ) ;
#28996 = CARTESIAN_POINT ( 'NONE',  ( 9.014152831625311890, -14.43863835250231809, 6.530762810602277924 ) ) ;
#28997 = CARTESIAN_POINT ( 'NONE',  ( -27.98912715346896007, 29.59629564344513142, 12.74957844391862949 ) ) ;
#28998 = CARTESIAN_POINT ( 'NONE',  ( 9.343263424913798687, -14.23786665604193047, 5.848946451764561516 ) ) ;
#28999 = ORIENTED_EDGE ( 'NONE', *, *, #26738, .T. ) ;
#29000 = ORIENTED_EDGE ( 'NONE', *, *, #19357, .T. ) ;
#29001 = CARTESIAN_POINT ( 'NONE',  ( -7.483314773547907528, 80.00000000000000000, 50.49999999999998579 ) ) ;
#29002 = EDGE_CURVE ( 'NONE', #14300, #15112, #22821, .T. ) ;
#29003 = CARTESIAN_POINT ( 'NONE',  ( -2.081668171172168513E-14, 75.00000000000001421, 52.49999999999999289 ) ) ;
#29004 = EDGE_CURVE ( 'NONE', #23685, #24152, #28314, .T. ) ;
#29005 = VECTOR ( 'NONE', #17684, 1000.000000000000000 ) ;
#29006 = CARTESIAN_POINT ( 'NONE',  ( 18.44003002641402134, -7.744679585886133033, 20.32200205377524682 ) ) ;
#29007 = CARTESIAN_POINT ( 'NONE',  ( -15.55757656137109457, -6.908027829072596937, 6.973843882838224317 ) ) ;
#29008 = CARTESIAN_POINT ( 'NONE',  ( -13.83213539500865785, 7.758783772730382111, -0.6213203435596476032 ) ) ;
#29009 = EDGE_LOOP ( 'NONE', ( #9075, #10849, #10037, #26166 ) ) ;
#29010 = ADVANCED_FACE ( 'NONE', ( #27695 ), #4135, .F. ) ;
#29011 = CARTESIAN_POINT ( 'NONE',  ( -17.83717022821180009, -34.31216324508217497, 34.50000000000000000 ) ) ;
#29012 = DIRECTION ( 'NONE',  ( -0.000000000000000000, -0.000000000000000000, 1.000000000000000000 ) ) ;
#29013 = DIRECTION ( 'NONE',  ( 1.000000000000000000, 0.000000000000000000, 0.000000000000000000 ) ) ;
#29014 = EDGE_CURVE ( 'NONE', #23725, #6974, #20951, .T. ) ;
#29015 = EDGE_LOOP ( 'NONE', ( #11811, #4035, #30691, #15226 ) ) ;
#29016 = LINE ( 'NONE', #314, #26785 ) ;
#29017 = ORIENTED_EDGE ( 'NONE', *, *, #16635, .F. ) ;
#29018 = EDGE_CURVE ( 'NONE', #18473, #29885, #23713, .T. ) ;
#29019 = CARTESIAN_POINT ( 'NONE',  ( -8.430595340551226613, 4.340342926365046594, 1.500000000000001332 ) ) ;
#29020 = CARTESIAN_POINT ( 'NONE',  ( 16.56617216130194237, 4.143135851892797206, 19.02573955821369012 ) ) ;
#29021 = CARTESIAN_POINT ( 'NONE',  ( -8.884323311075783991, -1.438332125858144295, -1.500000000000001776 ) ) ;
#29022 = ORIENTED_EDGE ( 'NONE', *, *, #26799, .T. ) ;
#29023 = EDGE_CURVE ( 'NONE', #23911, #22510, #21834, .T. ) ;
#29024 = CIRCLE ( 'NONE', #27483, 11.46182693247429718 ) ;
#29025 = AXIS2_PLACEMENT_3D ( 'NONE', #21342, #25584, #16369 ) ;
#29026 = FACE_OUTER_BOUND ( 'NONE', #1457, .T. ) ;
#29027 = AXIS2_PLACEMENT_3D ( 'NONE', #4496, #23811, #5106 ) ;
#29028 = DIRECTION ( 'NONE',  ( 0.000000000000000000, -1.000000000000000000, -0.000000000000000000 ) ) ;
#29029 = DIRECTION ( 'NONE',  ( 0.000000000000000000, 0.000000000000000000, -1.000000000000000000 ) ) ;
#29030 = CARTESIAN_POINT ( 'NONE',  ( 9.824744466605370263, -8.513189541288715745, 1.500000000000001332 ) ) ;
#29031 = DIRECTION ( 'NONE',  ( -0.000000000000000000, -0.000000000000000000, -1.000000000000000000 ) ) ;
#29032 = CARTESIAN_POINT ( 'NONE',  ( 11.21147646446735102, -30.29926891764210595, 1.500000000000000000 ) ) ;
#29033 = CARTESIAN_POINT ( 'NONE',  ( 31.46019086465472014, 15.19107625323260891, 40.06435153370524915 ) ) ;
#29034 = VERTEX_POINT ( 'NONE', #25354 ) ;
#29035 = DIRECTION ( 'NONE',  ( 0.000000000000000000, -0.000000000000000000, 1.000000000000000000 ) ) ;
#29036 = CARTESIAN_POINT ( 'NONE',  ( 40.89187623478217404, -5.790488632116400858, -19.50000000000000355 ) ) ;
#29037 = CARTESIAN_POINT ( 'NONE',  ( 0.000000000000000000, 0.000000000000000000, -11.49999999999999645 ) ) ;
#29038 = ORIENTED_EDGE ( 'NONE', *, *, #1521, .T. ) ;
#29039 = CARTESIAN_POINT ( 'NONE',  ( 29.19058584261892619, -28.18502476532347600, 16.25721844935590710 ) ) ;
#29040 = EDGE_CURVE ( 'NONE', #27397, #5492, #6481, .T. ) ;
#29041 = DIRECTION ( 'NONE',  ( -0.000000000000000000, -0.000000000000000000, 1.000000000000000000 ) ) ;
#29042 = EDGE_CURVE ( 'NONE', #7938, #28720, #6628, .T. ) ;
#29043 = DIRECTION ( 'NONE',  ( -1.000000000000000000, 0.000000000000000000, 0.000000000000000000 ) ) ;
#29044 = FILL_AREA_STYLE ('',( #14542 ) ) ;
#29045 = CARTESIAN_POINT ( 'NONE',  ( -20.65888525914364493, -38.75220717792906555, -19.50000000000000355 ) ) ;
#29046 = EDGE_CURVE ( 'NONE', #8392, #16888, #25659, .T. ) ;
#29047 = CARTESIAN_POINT ( 'NONE',  ( -4.375757216953428294E-15, -39.50000000000000000, 37.50000000000000000 ) ) ;
#29048 = VECTOR ( 'NONE', #15640, 1000.000000000000114 ) ;
#29049 = CARTESIAN_POINT ( 'NONE',  ( 38.97222564111406484, -2.062036942600702805, 32.22331656435463287 ) ) ;
#29051 = AXIS2_PLACEMENT_3D ( 'NONE', #18160, #6461, #10831 ) ;
#29050 = LINE ( 'NONE', #7693, #11046 ) ;
#29052 = ORIENTED_EDGE ( 'NONE', *, *, #16253, .F. ) ;
#29053 = DIRECTION ( 'NONE',  ( 1.000000000000000000, 0.000000000000000000, 0.000000000000000000 ) ) ;
#29054 = ORIENTED_EDGE ( 'NONE', *, *, #21985, .F. ) ;
#29055 = FACE_OUTER_BOUND ( 'NONE', #116, .T. ) ;
#29056 = DIRECTION ( 'NONE',  ( 1.000000000000000000, 0.000000000000000000, 0.000000000000000000 ) ) ;
#29057 = VERTEX_POINT ( 'NONE', #6772 ) ;
#29058 = ORIENTED_EDGE ( 'NONE', *, *, #30854, .F. ) ;
#29059 = CARTESIAN_POINT ( 'NONE',  ( -10.28466407052217413, -17.15343732189305115, 5.679672709359373073 ) ) ;
#29060 = ORIENTED_EDGE ( 'NONE', *, *, #9192, .T. ) ;
#29061 = EDGE_LOOP ( 'NONE', ( #20568, #8517 ) ) ;
#29062 = ORIENTED_EDGE ( 'NONE', *, *, #26046, .T. ) ;
#29063 = DIRECTION ( 'NONE',  ( -0.7416830501633135952, -0.6707505147970024284, 0.000000000000000000 ) ) ;
#29064 = CARTESIAN_POINT ( 'NONE',  ( -2.025933774932175968, 39.50000000000001421, 34.50000000000000000 ) ) ;
#29065 = CARTESIAN_POINT ( 'NONE',  ( -3.662523238938586001, -12.47340865698848056, 24.50000000000000000 ) ) ;
#29066 = VECTOR ( 'NONE', #24764, 1000.000000000000114 ) ;
#29067 = CARTESIAN_POINT ( 'NONE',  ( 4.533306948338440279, 16.41820958405265785, 18.47056384035244037 ) ) ;
#29068 = CARTESIAN_POINT ( 'NONE',  ( 42.49999999999998579, 50.00000000000000000, 12.49999999999999112 ) ) ;
#29069 = ORIENTED_EDGE ( 'NONE', *, *, #11867, .F. ) ;
#29070 = CIRCLE ( 'NONE', #16624, 20.00000000000000000 ) ;
#29071 = CARTESIAN_POINT ( 'NONE',  ( 8.728722367416583694, -2.516121109503213216, 21.50000000000000000 ) ) ;
#29072 = CARTESIAN_POINT ( 'NONE',  ( 0.000000000000000000, 0.000000000000000000, 21.50000000000000000 ) ) ;
#29073 = CARTESIAN_POINT ( 'NONE',  ( 14.25941570111288037, 14.04905143479254725, 18.92976555901915603 ) ) ;
#29074 = DIRECTION ( 'NONE',  ( 1.000000000000000000, 0.000000000000000000, 0.000000000000000000 ) ) ;
#29075 = VERTEX_POINT ( 'NONE', #25963 ) ;
#29076 = ADVANCED_FACE ( 'NONE', ( #4590 ), #20512, .T. ) ;
#29077 = AXIS2_PLACEMENT_3D ( 'NONE', #21982, #3121, #12641 ) ;
#29078 = EDGE_CURVE ( 'NONE', #23147, #21713, #26734, .T. ) ;
#29079 = CARTESIAN_POINT ( 'NONE',  ( -8.647361814388506929, -14.68561526379590809, 20.34789198813115263 ) ) ;
#29080 = CARTESIAN_POINT ( 'NONE',  ( -5.729465025513086419E-13, 44.07656359094158915, -16.50000000000000000 ) ) ;
#29081 = CARTESIAN_POINT ( 'NONE',  ( -5.549074438232170614, 16.11683645458454706, 5.652196082364320695 ) ) ;
#29082 = CARTESIAN_POINT ( 'NONE',  ( -4.163336342344337027E-14, 1.387778780781445676E-14, 24.50000000000000000 ) ) ;
#29083 = CARTESIAN_POINT ( 'NONE',  ( -18.35575104603287500, -7.986347210076461423, 18.63641924841378028 ) ) ;
#29084 = CARTESIAN_POINT ( 'NONE',  ( 6.974883619896790954, 5.687793815610376669, 1.500000000000001332 ) ) ;
#29085 = VERTEX_POINT ( 'NONE', #14091 ) ;
#29086 = EDGE_LOOP ( 'NONE', ( #20402, #2672, #11148, #1276 ) ) ;
#29087 = CYLINDRICAL_SURFACE ( 'NONE', #20006, 23.20393738267408779 ) ;
#29088 = CARTESIAN_POINT ( 'NONE',  ( 5.374868878255610660, 44.10336124695606230, -19.50000000000000355 ) ) ;
#29089 = CARTESIAN_POINT ( 'NONE',  ( -14.82920317518825470, 13.44671003463071735, 7.272049892295485485 ) ) ;
#29090 = CARTESIAN_POINT ( 'NONE',  ( 0.6517800498974439805, -17.02970683165111154, 5.651492010659112886 ) ) ;
#29091 = VERTEX_POINT ( 'NONE', #17211 ) ;
#29092 = APPLICATION_PROTOCOL_DEFINITION ( 'draft international standard', 'automotive_design', 1998, #10574 ) ;
#29093 = CARTESIAN_POINT ( 'NONE',  ( 16.17629920998172821, -5.470921186992126373, 19.02573955821369722 ) ) ;
#29094 = LINE ( 'NONE', #24250, #21648 ) ;
#29095 = VECTOR ( 'NONE', #6955, 1000.000000000000000 ) ;
#29096 = VERTEX_POINT ( 'NONE', #2568 ) ;
#29097 = CARTESIAN_POINT ( 'NONE',  ( 4.263339901971998636, 16.49757000336417789, 18.36582235739946611 ) ) ;
#29098 = DIRECTION ( 'NONE',  ( -1.000000000000000000, 0.000000000000000000, 0.000000000000000000 ) ) ;
#29099 = CARTESIAN_POINT ( 'NONE',  ( -7.677470532982090035, -15.25505107808950278, 19.21769074125272780 ) ) ;
#29100 = CARTESIAN_POINT ( 'NONE',  ( -37.05526867389234980, -13.52123220197743336, 34.89587700162063300 ) ) ;
#29101 = ORIENTED_EDGE ( 'NONE', *, *, #18735, .F. ) ;
#29102 = CARTESIAN_POINT ( 'NONE',  ( -9.301547456646385825, 8.591538895647085283, -1.500000000000000000 ) ) ;
#29103 = DIRECTION ( 'NONE',  ( -0.000000000000000000, -0.000000000000000000, -1.000000000000000000 ) ) ;
#29104 = DIRECTION ( 'NONE',  ( -0.000000000000000000, -0.000000000000000000, 1.000000000000000000 ) ) ;
#29105 = LINE ( 'NONE', #7746, #860 ) ;
#29106 = ORIENTED_EDGE ( 'NONE', *, *, #9757, .F. ) ;
#29107 = LINE ( 'NONE', #710, #15794 ) ;
#29108 = CARTESIAN_POINT ( 'NONE',  ( 3.118309183252346628, 17.14266753270391774, -1.500000000000000000 ) ) ;
#29109 = CARTESIAN_POINT ( 'NONE',  ( 14.79007711409979819, 13.46370387462956586, 5.652912763329819512 ) ) ;
#29110 = CARTESIAN_POINT ( 'NONE',  ( -0.6660349346848389862, -20.00682905350634755, 6.641371103590088865 ) ) ;
#29111 = EDGE_CURVE ( 'NONE', #13000, #13876, #9596, .T. ) ;
#29112 = CARTESIAN_POINT ( 'NONE',  ( 49.99999999999998579, 70.00000000000000000, -92.50000000000000000 ) ) ;
#29113 = ADVANCED_FACE ( 'NONE', ( #368 ), #26588, .F. ) ;
#29115 = ADVANCED_FACE ( 'NONE', ( #9583 ), #14419, .F. ) ;
#29114 = CARTESIAN_POINT ( 'NONE',  ( -10.47960520055065636, -7.757439966934454034, 1.500000000000001332 ) ) ;
#29116 = CIRCLE ( 'NONE', #27632, 7.500000000000000000 ) ;
#29117 = DIRECTION ( 'NONE',  ( 1.000000000000000000, 0.000000000000000000, 0.000000000000000000 ) ) ;
#29118 = CARTESIAN_POINT ( 'NONE',  ( 0.000000000000000000, 42.50000000000000000, 32.33822642395377045 ) ) ;
#29119 = ORIENTED_EDGE ( 'NONE', *, *, #8454, .T. ) ;
#29120 = DIRECTION ( 'NONE',  ( -0.000000000000000000, -0.000000000000000000, 1.000000000000000000 ) ) ;
#29121 = CARTESIAN_POINT ( 'NONE',  ( 0.000000000000000000, 90.00000000000001421, -40.00000000000000711 ) ) ;
#29122 = B_SPLINE_CURVE_WITH_KNOTS ( 'NONE', 3,
 ( #11395, #9195, #21175, #2483, #16674, #12000, #30699, #8902, #18425, #9049, #25884, #18707, #4515, #5127, #14640, #23984, #2957, #24611 ),
 .UNSPECIFIED., .F., .F.,
 ( 4, 2, 2, 2, 2, 2, 2, 2, 4 ),
 ( 0.000000000000000000, 0.0003967869494442914082, 0.0007935738988885828165, 0.001190360848332874116, 0.001587147797777165633, 0.001983934747221457150, 0.002380721696665748233, 0.002777508646110039749, 0.003174295595554331266 ),
 .UNSPECIFIED. ) ;
#29123 = ORIENTED_EDGE ( 'NONE', *, *, #431, .F. ) ;
#29124 = ORIENTED_EDGE ( 'NONE', *, *, #15253, .F. ) ;
#29125 = B_SPLINE_CURVE_WITH_KNOTS ( 'NONE', 3,
 ( #3658, #15811, #3345, #22213, #15345, #1481 ),
 .UNSPECIFIED., .F., .F.,
 ( 4, 2, 4 ),
 ( 2.380730970505090229E-07, 0.002629065763328460210, 0.005257893453559869812 ),
 .UNSPECIFIED. ) ;
#29126 = CARTESIAN_POINT ( 'NONE',  ( 8.616279238414451314, -7.781333699927420966, -1.500000000000000000 ) ) ;
#29127 = FACE_OUTER_BOUND ( 'NONE', #29458, .T. ) ;
#29128 = ORIENTED_EDGE ( 'NONE', *, *, #13613, .F. ) ;
#29129 = CARTESIAN_POINT ( 'NONE',  ( 15.31102578509455903, 12.89549683364648835, 18.55820869691756769 ) ) ;
#29130 = CARTESIAN_POINT ( 'NONE',  ( -10.81179434590808697, -16.84691785479785864, 7.595116371587256054 ) ) ;
#29131 = ORIENTED_EDGE ( 'NONE', *, *, #20617, .F. ) ;
#29132 = B_SPLINE_CURVE_WITH_KNOTS ( 'NONE', 3,
 ( #30241, #25565, #20424, #8886, #29946, #8582, #23368, #27760, #10755, #18410, #15735, #20266, #4188, #25254, #3901, #23200, #6390, #22906, #1557, #11066 ),
 .UNSPECIFIED., .F., .F.,
 ( 4, 2, 2, 2, 2, 2, 2, 2, 2, 4 ),
 ( 0.000000000000000000, 0.06250000000000030531, 0.1250000000000006106, 0.1875000000000009159, 0.2187500000000009714, 0.2500000000000010547, 0.3125000000000007772, 0.3750000000000005551, 0.4375000000000002776, 0.5000000000000000000 ),
 .UNSPECIFIED. ) ;
#29133 = CARTESIAN_POINT ( 'NONE',  ( -16.86183147812084115, 2.368508504629202260, 7.359006845440219102 ) ) ;
#29134 = B_SPLINE_CURVE_WITH_KNOTS ( 'NONE', 3,
 ( #18223, #6056, #1388, #8567, #17605, #3566, #29615, #6372, #10905, #20406, #22579, #18071, #25400, #27588, #12770, #22272 ),
 .UNSPECIFIED., .F., .F.,
 ( 4, 2, 2, 2, 2, 2, 2, 4 ),
 ( 0.4999999999999997224, 0.6249999999999997780, 0.6874999999999997780, 0.7187499999999997780, 0.7499999999999997780, 0.8124999999999997780, 0.8749999999999997780, 1.000000000000000000 ),
 .UNSPECIFIED. ) ;
#29135 = DIRECTION ( 'NONE',  ( 1.000000000000000000, 0.000000000000000000, 0.000000000000000000 ) ) ;
#29136 = DIRECTION ( 'NONE',  ( 0.000000000000000000, -0.000000000000000000, 1.000000000000000000 ) ) ;
#29137 = EDGE_LOOP ( 'NONE', ( #7733, #5378, #8549, #9526 ) ) ;
#29138 = FACE_OUTER_BOUND ( 'NONE', #29009, .T. ) ;
#29139 = CIRCLE ( 'NONE', #24652, 0.7499999999999997780 ) ;
#29140 = ORIENTED_EDGE ( 'NONE', *, *, #3490, .T. ) ;
#29141 = EDGE_LOOP ( 'NONE', ( #28198, #28380, #6878, #16003, #21226, #27390, #14658, #27559 ) ) ;
#29142 = CARTESIAN_POINT ( 'NONE',  ( -6.737371319102178902, 18.84978071134531419, 18.73743063545763121 ) ) ;
#29143 = CARTESIAN_POINT ( 'NONE',  ( 3.474270935886293987, -15.38174572367601911, -0.6213203435596476032 ) ) ;
#29144 = AXIS2_PLACEMENT_3D ( 'NONE', #23904, #26713, #16895 ) ;
#29145 = DIRECTION ( 'NONE',  ( -3.469446951953611033E-15, 1.000000000000000000, 0.000000000000000000 ) ) ;
#29146 = CARTESIAN_POINT ( 'NONE',  ( -21.56949286799591903, -35.43467754613438814, 29.49548763488747483 ) ) ;
#29147 = DIRECTION ( 'NONE',  ( 0.000000000000000000, -0.000000000000000000, -1.000000000000000000 ) ) ;
#29148 = DIRECTION ( 'NONE',  ( -0.1423148382732853101, 0.9898214418809327952, 0.000000000000000000 ) ) ;
#29149 = ORIENTED_EDGE ( 'NONE', *, *, #28074, .T. ) ;
#29150 = EDGE_CURVE ( 'NONE', #22434, #11709, #26822, .T. ) ;
#29151 = CARTESIAN_POINT ( 'NONE',  ( 10.38931136226422325, -17.11076273665786118, 7.176035686813569292 ) ) ;
#29152 = CARTESIAN_POINT ( 'NONE',  ( 8.099999999999999645, 0.000000000000000000, -6.600000000000001421 ) ) ;
#29153 = VERTEX_POINT ( 'NONE', #19095 ) ;
#29154 = VERTEX_POINT ( 'NONE', #29071 ) ;
#29155 = CIRCLE ( 'NONE', #6733, 20.00000000000000355 ) ;
#29156 = DIRECTION ( 'NONE',  ( 0.7557495743542582689, -0.6548607339452849896, 0.000000000000000000 ) ) ;
#29157 = CARTESIAN_POINT ( 'NONE',  ( -8.840471615930058036, 1.687027447297517080, 21.50000000000000000 ) ) ;
#29158 = DIRECTION ( 'NONE',  ( -1.000000000000000000, 0.000000000000000000, 0.000000000000000000 ) ) ;
#29159 = CARTESIAN_POINT ( 'NONE',  ( -15.16517293421789070, -7.781889191988407894, 7.652108011868850923 ) ) ;
#29160 = PLANE ( 'NONE',  #11677 ) ;
#29161 = CARTESIAN_POINT ( 'NONE',  ( -70.00000000000000000, 50.00000000000000000, 12.49999999999999112 ) ) ;
#29162 = VERTEX_POINT ( 'NONE', #9437 ) ;
#29163 = FACE_OUTER_BOUND ( 'NONE', #6006, .T. ) ;
#29164 = VECTOR ( 'NONE', #29925, 1000.000000000000000 ) ;
#29165 = CARTESIAN_POINT ( 'NONE',  ( -17.64439154790314390, -9.416908767371243272, 19.85730954408918691 ) ) ;
#29166 = CARTESIAN_POINT ( 'NONE',  ( 16.86235748570416249, 2.342382300094909553, 7.176035686813569292 ) ) ;
#29167 = ORIENTED_EDGE ( 'NONE', *, *, #20624, .F. ) ;
#29168 = CARTESIAN_POINT ( 'NONE',  ( 15.51850634784529959, 12.64495090725178983, 6.310736198168394928 ) ) ;
#29169 = ORIENTED_EDGE ( 'NONE', *, *, #5934, .T. ) ;
#29170 = CARTESIAN_POINT ( 'NONE',  ( 16.13887868878510190, -5.569097860077081741, 7.196036389296800451 ) ) ;
#29171 = DIRECTION ( 'NONE',  ( 1.000000000000000000, 0.000000000000000000, 0.000000000000000000 ) ) ;
#29172 = CARTESIAN_POINT ( 'NONE',  ( -24.57973596967191554, 7.302173446879558050, 45.11631295118280605 ) ) ;
#29173 = ORIENTED_EDGE ( 'NONE', *, *, #15315, .F. ) ;
#29174 = AXIS2_PLACEMENT_3D ( 'NONE', #4476, #26134, #7429 ) ;
#29175 = EDGE_CURVE ( 'NONE', #3976, #11851, #7089, .T. ) ;
#29176 = CARTESIAN_POINT ( 'NONE',  ( 48.71078001599239826, 69.96156514568451712, 57.45356112030430751 ) ) ;
#29177 = EDGE_CURVE ( 'NONE', #14731, #11716, #14777, .T. ) ;
#29178 = LINE ( 'NONE', #17327, #6114 ) ;
#29179 = CARTESIAN_POINT ( 'NONE',  ( -39.00000000000000000, -46.58316968839002925, 16.34922658321931976 ) ) ;
#29180 = DIRECTION ( 'NONE',  ( -0.000000000000000000, -0.000000000000000000, -1.000000000000000000 ) ) ;
#29181 = VECTOR ( 'NONE', #3746, 1000.000000000000000 ) ;
#29182 = CARTESIAN_POINT ( 'NONE',  ( -24.03057240117691862, 26.57182937991349903, 1.500000000000000000 ) ) ;
#29183 = CARTESIAN_POINT ( 'NONE',  ( 9.766261594859264150, -13.96654203752514256, 20.34789198813115263 ) ) ;
#29184 = DIRECTION ( 'NONE',  ( -1.000000000000000000, 0.000000000000000000, 0.000000000000000000 ) ) ;
#29185 = ORIENTED_EDGE ( 'NONE', *, *, #30731, .T. ) ;
#29186 = EDGE_CURVE ( 'NONE', #18557, #13268, #16365, .T. ) ;
#29187 = CARTESIAN_POINT ( 'NONE',  ( 37.99999999999999289, 90.00000000000001421, -75.50000000000001421 ) ) ;
#29188 = CARTESIAN_POINT ( 'NONE',  ( -5.105024945673440229, 42.22604126506271172, -1.500000000000000000 ) ) ;
#29189 = DIRECTION ( 'NONE',  ( 0.000000000000000000, 0.000000000000000000, 1.000000000000000000 ) ) ;
#29190 = ORIENTED_EDGE ( 'NONE', *, *, #7636, .T. ) ;
#29191 = CARTESIAN_POINT ( 'NONE',  ( 28.00422547688649644, -29.57936985937913477, 13.46106986886504941 ) ) ;
#29193 = ADVANCED_FACE ( 'NONE', ( #9889 ), #16594, .F. ) ;
#29192 = CARTESIAN_POINT ( 'NONE',  ( 46.99999999999998579, 90.00000000000001421, 22.49999999999999289 ) ) ;
#29194 = DIRECTION ( 'NONE',  ( 0.5503133621338236470, -0.8349582046168341209, 0.000000000000000000 ) ) ;
#29195 = CYLINDRICAL_SURFACE ( 'NONE', #8300, 34.99999999999933920 ) ;
#29196 = CARTESIAN_POINT ( 'NONE',  ( 5.105024945673418912, -42.22604126506271882, -1.500000000000000000 ) ) ;
#29197 = EDGE_CURVE ( 'NONE', #1784, #30101, #21062, .T. ) ;
#29198 = PRESENTATION_STYLE_ASSIGNMENT (( #186 ) ) ;
#29199 = EDGE_CURVE ( 'NONE', #25178, #10235, #19839, .T. ) ;
#29200 = CARTESIAN_POINT ( 'NONE',  ( 4.963855673496207821, 42.15448181593355059, 34.60401223484481648 ) ) ;
#29201 = CARTESIAN_POINT ( 'NONE',  ( -2.352830851074180440, -9.185733585337901630, 21.50000000000000000 ) ) ;
#29202 = ORIENTED_EDGE ( 'NONE', *, *, #2678, .T. ) ;
#29203 = AXIS2_PLACEMENT_3D ( 'NONE', #3829, #27690, #11468 ) ;
#29204 = CIRCLE ( 'NONE', #7786, 0.7500000000000006661 ) ;
#29205 = DIRECTION ( 'NONE',  ( 0.000000000000000000, 0.000000000000000000, 1.000000000000000000 ) ) ;
#29206 = ORIENTED_EDGE ( 'NONE', *, *, #21956, .F. ) ;
#29207 = DIRECTION ( 'NONE',  ( 1.000000000000000000, 0.000000000000000000, 0.000000000000000000 ) ) ;
#29208 = DIRECTION ( 'NONE',  ( -0.000000000000000000, -0.000000000000000000, 1.000000000000000000 ) ) ;
#29209 = ORIENTED_EDGE ( 'NONE', *, *, #17583, .F. ) ;
#29210 = ORIENTED_EDGE ( 'NONE', *, *, #20067, .F. ) ;
#29211 = FACE_BOUND ( 'NONE', #27187, .T. ) ;
#29212 = ORIENTED_EDGE ( 'NONE', *, *, #12004, .T. ) ;
#29213 = CIRCLE ( 'NONE', #9283, 0.7500000000000004441 ) ;
#29214 = ORIENTED_EDGE ( 'NONE', *, *, #16258, .F. ) ;
#29215 = DIRECTION ( 'NONE',  ( -0.000000000000000000, 0.000000000000000000, 1.000000000000000000 ) ) ;
#29216 = AXIS2_PLACEMENT_3D ( 'NONE', #12832, #5963, #10791 ) ;
#29217 = EDGE_CURVE ( 'NONE', #13626, #20319, #30301, .T. ) ;
#29218 = CARTESIAN_POINT ( 'NONE',  ( -25.23756106473024019, 11.43858098102958287, -11.49999999999999645 ) ) ;
#29219 = ADVANCED_FACE ( 'NONE', ( #28922 ), #29308, .T. ) ;
#29220 = DIRECTION ( 'NONE',  ( -0.000000000000000000, 0.000000000000000000, 1.000000000000000000 ) ) ;
#29221 = CARTESIAN_POINT ( 'NONE',  ( -37.81047817032544600, 10.41981227368125218, 14.33565414798128934 ) ) ;
#29222 = CARTESIAN_POINT ( 'NONE',  ( -4.100931858250869588, 19.90478481566557178, -1.500000000000000000 ) ) ;
#29223 = ORIENTED_EDGE ( 'NONE', *, *, #8693, .F. ) ;
#29224 = EDGE_CURVE ( 'NONE', #2852, #7465, #9373, .T. ) ;
#29225 = CIRCLE ( 'NONE', #18278, 9.482273699623480212 ) ;
#29226 = CARTESIAN_POINT ( 'NONE',  ( 0.000000000000000000, 1.699320956058915452E-16, -1.500000000000001776 ) ) ;
#29227 = CARTESIAN_POINT ( 'NONE',  ( -7.322557715923444732, 14.41080185948837311, -0.6213203435596476032 ) ) ;
#29228 = LINE ( 'NONE', #14716, #3672 ) ;
#29229 = ORIENTED_EDGE ( 'NONE', *, *, #25615, .F. ) ;
#29230 = EDGE_CURVE ( 'NONE', #26490, #24252, #10045, .T. ) ;
#29231 = VECTOR ( 'NONE', #222, 1000.000000000000000 ) ;
#29232 = CARTESIAN_POINT ( 'NONE',  ( -17.22181377296915272, -14.41708049311147555, 1.500000000000000000 ) ) ;
#29233 = DIRECTION ( 'NONE',  ( -0.000000000000000000, -1.000000000000000000, -0.000000000000000000 ) ) ;
#29234 = CARTESIAN_POINT ( 'NONE',  ( 10.23384659304339372, -13.64843352988230230, 5.749491821935610147 ) ) ;
#29235 = EDGE_CURVE ( 'NONE', #17226, #4417, #7897, .T. ) ;
#29236 = CARTESIAN_POINT ( 'NONE',  ( 33.56327786402393798, -10.22184951998668012, 35.67222448829685533 ) ) ;
#29237 = VECTOR ( 'NONE', #20927, 1000.000000000000000 ) ;
#29238 = EDGE_LOOP ( 'NONE', ( #21513, #12993, #20087, #16435 ) ) ;
#29239 = ORIENTED_EDGE ( 'NONE', *, *, #11905, .T. ) ;
#29240 =( NAMED_UNIT ( * ) PLANE_ANGLE_UNIT ( ) SI_UNIT ( $, .RADIAN. ) );
#29241 = LINE ( 'NONE', #14889, #3201 ) ;
#29242 = CARTESIAN_POINT ( 'NONE',  ( -15.30875331599080091, 12.89789204219718854, 5.653912893140659257 ) ) ;
#29243 = CARTESIAN_POINT ( 'NONE',  ( -50.00000000000000000, -50.00000000000000000, -92.50000000000000000 ) ) ;
#29244 = ORIENTED_EDGE ( 'NONE', *, *, #4768, .F. ) ;
#29245 = APPLICATION_PROTOCOL_DEFINITION ( 'draft international standard', 'automotive_design', 1998, #28111 ) ;
#29246 = CARTESIAN_POINT ( 'NONE',  ( 16.19239463133111911, -5.428304825925631683, 19.21769074125273491 ) ) ;
#29247 = CIRCLE ( 'NONE', #10314, 0.7499999999999997780 ) ;
#29248 = LINE ( 'NONE', #19577, #6229 ) ;
#29249 = VECTOR ( 'NONE', #10226, 1000.000000000000000 ) ;
#29250 = ADVANCED_FACE ( 'NONE', ( #10818 ), #22499, .T. ) ;
#29251 = ORIENTED_EDGE ( 'NONE', *, *, #9991, .T. ) ;
#29252 = CARTESIAN_POINT ( 'NONE',  ( -49.99999999999955236, -4.926614671774132148E-13, 79.49999999999998579 ) ) ;
#29253 = DIRECTION ( 'NONE',  ( 1.000000000000000000, 0.000000000000000000, 0.000000000000000000 ) ) ;
#29254 = EDGE_CURVE ( 'NONE', #4883, #8580, #22196, .T. ) ;
#29255 = AXIS2_PLACEMENT_3D ( 'NONE', #27446, #8577, #10748 ) ;
#29256 = PLANE ( 'NONE',  #22795 ) ;
#29257 = CARTESIAN_POINT ( 'NONE',  ( -31.96377083499153571, -24.36009066984772531, 30.63716218392069024 ) ) ;
#29258 = ORIENTED_EDGE ( 'NONE', *, *, #28658, .F. ) ;
#29259 = DIRECTION ( 'NONE',  ( -1.000000000000000000, 0.000000000000000000, -0.000000000000000000 ) ) ;
#29260 = VECTOR ( 'NONE', #2209, 1000.000000000000000 ) ;
#29261 = CARTESIAN_POINT ( 'NONE',  ( 39.99999999999998579, 80.00000000000001421, 22.49999999999999289 ) ) ;
#29262 = VECTOR ( 'NONE', #11727, 1000.000000000000000 ) ;
#29263 = DIRECTION ( 'NONE',  ( 0.000000000000000000, 0.000000000000000000, 1.000000000000000000 ) ) ;
#29264 = DIRECTION ( 'NONE',  ( -0.000000000000000000, 0.000000000000000000, -1.000000000000000000 ) ) ;
#29265 = CIRCLE ( 'NONE', #13331, 28.20443790117963800 ) ;
#29266 = ORIENTED_EDGE ( 'NONE', *, *, #20, .F. ) ;
#29267 = CYLINDRICAL_SURFACE ( 'NONE', #15295, 20.00000000000000355 ) ;
#29268 = CARTESIAN_POINT ( 'NONE',  ( 16.01802636632491428, -5.877265577664587681, 5.759928666072748449 ) ) ;
#29269 = VECTOR ( 'NONE', #30254, 1000.000000000000000 ) ;
#29270 = DIRECTION ( 'NONE',  ( -0.000000000000000000, -0.000000000000000000, -1.000000000000000000 ) ) ;
#29271 = VECTOR ( 'NONE', #30545, 1000.000000000000000 ) ;
#29272 = DIRECTION ( 'NONE',  ( -8.962737959213495958E-15, 1.000000000000000000, 0.000000000000000000 ) ) ;
#29273 = AXIS2_PLACEMENT_3D ( 'NONE', #554, #12430, #28799 ) ;
#29274 = DIRECTION ( 'NONE',  ( 0.000000000000000000, 0.4961389383568337030, -0.8682431421244592995 ) ) ;
#29275 = DIRECTION ( 'NONE',  ( -0.000000000000000000, -0.000000000000000000, -1.000000000000000000 ) ) ;
#29276 = CYLINDRICAL_SURFACE ( 'NONE', #9400, 9.482273699623480212 ) ;
#29277 = ORIENTED_EDGE ( 'NONE', *, *, #1549, .T. ) ;
#29278 = LINE ( 'NONE', #26792, #25706 ) ;
#29279 = VECTOR ( 'NONE', #8565, 1000.000000000000000 ) ;
#29280 = CARTESIAN_POINT ( 'NONE',  ( -9.675133109038686285, -8.168544852422948921, -1.500000000000000000 ) ) ;
#29281 = ORIENTED_EDGE ( 'NONE', *, *, #26299, .T. ) ;
#29282 = VERTEX_POINT ( 'NONE', #24534 ) ;
#29283 = CARTESIAN_POINT ( 'NONE',  ( -16.80735851984694662, 38.39305298849780002, 23.11497516139116826 ) ) ;
#29284 = CIRCLE ( 'NONE', #18337, 15.00000000000000000 ) ;
#29285 = CARTESIAN_POINT ( 'NONE',  ( -4.843246358613172653, 49.76713946421946133, -40.79481846074538254 ) ) ;
#29286 = AXIS2_PLACEMENT_3D ( 'NONE', #1593, #28087, #11244 ) ;
#29287 = VERTEX_POINT ( 'NONE', #22650 ) ;
#29288 = CARTESIAN_POINT ( 'NONE',  ( -27.60655220535237575, -25.35568602214586065, 27.50000000000000355 ) ) ;
#29289 = CARTESIAN_POINT ( 'NONE',  ( 15.41319392345653938, 12.77323265862689183, 18.71435384576123440 ) ) ;
#29290 = B_SPLINE_CURVE_WITH_KNOTS ( 'NONE', 3,
 ( #3135, #1103, #22151, #8128 ),
 .UNSPECIFIED., .F., .F.,
 ( 4, 4 ),
 ( 2.143643656964903641E-07, 0.003421830178490235450 ),
 .UNSPECIFIED. ) ;
#29291 = CARTESIAN_POINT ( 'NONE',  ( 15.89967663190787839, -6.161197767010743398, 20.32367522806703874 ) ) ;
#29292 = DIRECTION ( 'NONE',  ( -1.000000000000000000, 0.000000000000000000, 0.000000000000000000 ) ) ;
#29293 = AXIS2_PLACEMENT_3D ( 'NONE', #706, #10537, #1329 ) ;
#29294 = CARTESIAN_POINT ( 'NONE',  ( -30.75232512042845556, -9.966982604840850968, 1.500000000000000000 ) ) ;
#29295 = VERTEX_POINT ( 'NONE', #29534 ) ;
#29296 = AXIS2_PLACEMENT_3D ( 'NONE', #6279, #15636, #3794 ) ;
#29297 = EDGE_CURVE ( 'NONE', #544, #13676, #19868, .T. ) ;
#29298 = CARTESIAN_POINT ( 'NONE',  ( -17.20435420003449423, -1.463329469628170898, 24.50000000000000000 ) ) ;
#29299 = ORIENTED_EDGE ( 'NONE', *, *, #1002, .T. ) ;
#29300 = DIRECTION ( 'NONE',  ( 0.000000000000000000, 1.132880637372608986E-16, -1.000000000000000000 ) ) ;
#29301 = EDGE_LOOP ( 'NONE', ( #23772, #14273, #2832, #22403 ) ) ;
#29302 = CARTESIAN_POINT ( 'NONE',  ( -6.908049759614255159, 18.76916546752685733, 19.61564845152807379 ) ) ;
#29303 = AXIS2_PLACEMENT_3D ( 'NONE', #6386, #4038, #13564 ) ;
#29304 = CARTESIAN_POINT ( 'NONE',  ( 26.40719054689828837, 31.30341782987545329, 29.91384141721222889 ) ) ;
#29305 = B_SPLINE_SURFACE_WITH_KNOTS ( 'NONE', 3, 1, ( 
 ( #23061, #14280 ),
 ( #4773, #2451 ),
 ( #30825, #19439 ),
 ( #2280, #21139 ),
 ( #21619, #19281 ),
 ( #9472, #2758 ),
 ( #255, #21462 ),
 ( #410, #28349 ),
 ( #28804, #26002 ),
 ( #26622, #18833 ),
 ( #28956, #7441 ),
 ( #12271, #26464 ),
 ( #4631, #18988 ),
 ( #23799, #1711 ),
 ( #21773, #7130 ),
 ( #11800, #6975 ),
 ( #14129, #9622 ),
 ( #21306, #9928 ),
 ( #17095, #23635 ),
 ( #16641, #5249 ),
 ( #104, #11970 ),
 ( #11226, #19132 ),
 ( #28648, #7274 ),
 ( #4940, #24269 ),
 ( #19739, #2916 ),
 ( #3367, #12736 ),
 ( #7748, #17561 ),
 ( #26780, #27080 ),
 ( #5704, #17253 ),
 ( #29573, #17707 ),
 ( #10691, #24418 ) ),
 .UNSPECIFIED., .F., .F., .F.,
 ( 4, 3, 3, 3, 3, 3, 3, 3, 3, 3, 4 ),
 ( 2, 2 ),
 ( 0.000000000000000000, 0.05425176834609633791, 0.1085332949128352958, 0.1623767749169382768, 0.2157504826133063158, 0.2688657508888171455, 0.3218907763505476360, 0.3749548578363336993, 0.4282048033836242107, 0.4818374082110501444, 0.4999999999131651274 ),
 ( 0.000000000000000000, 1.000000000000000000 ),
 .UNSPECIFIED. ) ;
#29306 = CARTESIAN_POINT ( 'NONE',  ( 19.61965483366450158, 3.971857776421113595, 7.280727868105637768 ) ) ;
#29307 = CARTESIAN_POINT ( 'NONE',  ( -14.70245401545668962, 13.58508552794529400, 19.11611934778430921 ) ) ;
#29308 = CONICAL_SURFACE ( 'NONE', #1444, 9.000000000000000000, 1.047197551196600296 ) ;
#29309 = CARTESIAN_POINT ( 'NONE',  ( -8.481700458822087896, -14.78796854237962322, 18.34838970509067479 ) ) ;
#29310 = CARTESIAN_POINT ( 'NONE',  ( -23.69684009293500893, 33.86367947567046599, 29.65129610998314647 ) ) ;
#29311 = CARTESIAN_POINT ( 'NONE',  ( -28.34828976096172681, 29.18752572968383419, -1.500000000000000000 ) ) ;
#29312 = FACE_OUTER_BOUND ( 'NONE', #5192, .T. ) ;
#29313 = VERTEX_POINT ( 'NONE', #14872 ) ;
#29314 = CARTESIAN_POINT ( 'NONE',  ( 10.34995923732865286, -17.13460031806512873, 6.211014596808754007 ) ) ;
#29315 = CARTESIAN_POINT ( 'NONE',  ( 27.19231046524321371, -25.90237096470084310, 34.50000000000000711 ) ) ;
#29316 = CIRCLE ( 'NONE', #10883, 21.71568325578132530 ) ;
#29317 = DIRECTION ( 'NONE',  ( 0.000000000000000000, 0.000000000000000000, 1.000000000000000000 ) ) ;
#29318 = CARTESIAN_POINT ( 'NONE',  ( 19.86493687747363168, 2.320961355260795944, 7.156831654632821227 ) ) ;
#29319 = VERTEX_POINT ( 'NONE', #29386 ) ;
#29320 = ORIENTED_EDGE ( 'NONE', *, *, #25034, .T. ) ;
#29321 = DIRECTION ( 'NONE',  ( -1.000000000000000000, 0.000000000000000000, 0.000000000000000000 ) ) ;
#29322 = CARTESIAN_POINT ( 'NONE',  ( 18.70859934877967135, -7.070433808158456124, 19.61564845152809511 ) ) ;
#29323 = ORIENTED_EDGE ( 'NONE', *, *, #8243, .T. ) ;
#29324 = CARTESIAN_POINT ( 'NONE',  ( 5.881244434206234217, 6.812559277181991391, -1.500000000000000888 ) ) ;
#29325 = B_SPLINE_CURVE_WITH_KNOTS ( 'NONE', 3,
 ( #12079, #24068, #367, #21577, #14238, #26107, #28145, #6938, #16448, #6770, #4737, #21105, #16295, #25813, #23755, #23920, #2409, #21427 ),
 .UNSPECIFIED., .F., .F.,
 ( 4, 2, 2, 2, 2, 2, 2, 2, 4 ),
 ( 0.000000000000000000, 0.0003967869494442890772, 0.0007935738988885781544, 0.001190360848332867177, 0.001587147797777156309, 0.001983934747221445440, 0.002380721696665734355, 0.002777508646110023703, 0.003174295595554312618 ),
 .UNSPECIFIED. ) ;
#29326 = CARTESIAN_POINT ( 'NONE',  ( -4.163336342344337027E-14, 1.387778780781445676E-14, 67.49999999999997158 ) ) ;
#29327 = DIRECTION ( 'NONE',  ( 1.000000000000000000, 0.000000000000000000, 0.000000000000000000 ) ) ;
#29328 = AXIS2_PLACEMENT_3D ( 'NONE', #18513, #21287, #4467 ) ;
#29329 = ORIENTED_EDGE ( 'NONE', *, *, #23445, .T. ) ;
#29330 = AXIS2_PLACEMENT_3D ( 'NONE', #9895, #9732, #3033 ) ;
#29331 = CARTESIAN_POINT ( 'NONE',  ( -9.982956658368040692, -17.33059308371926122, 20.15039051365864253 ) ) ;
#29332 = CARTESIAN_POINT ( 'NONE',  ( 14.25941570111287682, 14.04905143479254548, 6.233981582756856987 ) ) ;
#29333 = CARTESIAN_POINT ( 'NONE',  ( 19.89797503522100541, 2.188012981718273853, 6.641371103590088865 ) ) ;
#29334 = ORIENTED_EDGE ( 'NONE', *, *, #16097, .F. ) ;
#29335 = LINE ( 'NONE', #8125, #18807 ) ;
#29336 = ORIENTED_EDGE ( 'NONE', *, *, #19914, .F. ) ;
#29337 = CARTESIAN_POINT ( 'NONE',  ( -13.71169828459619389, 10.15410312392310033, 20.24143955528809613 ) ) ;
#29338 = CARTESIAN_POINT ( 'NONE',  ( 20.71335220384823117, 27.86167394782616213, -16.50000000000000000 ) ) ;
#29339 = CONICAL_SURFACE ( 'NONE', #7430, 35.37867965644036872, 0.7853981633974500554 ) ;
#29340 = CARTESIAN_POINT ( 'NONE',  ( -10.51513057463695411, -17.01270198993486460, 20.34789198813115263 ) ) ;
#29341 = ORIENTED_EDGE ( 'NONE', *, *, #17756, .F. ) ;
#29342 = DIRECTION ( 'NONE',  ( -0.000000000000000000, -0.000000000000000000, -1.000000000000000000 ) ) ;
#29343 = CYLINDRICAL_SURFACE ( 'NONE', #5182, 32.50000000000000000 ) ;
#29344 = DIRECTION ( 'NONE',  ( 1.000000000000000000, 0.000000000000000000, 0.000000000000000000 ) ) ;
#29345 = PRESENTATION_LAYER_ASSIGNMENT (  '', '', ( #19881 ) ) ;
#29346 = CARTESIAN_POINT ( 'NONE',  ( 31.10910608030087943, 19.98124338977578773, 34.49999999999999289 ) ) ;
#29347 = CARTESIAN_POINT ( 'NONE',  ( -11.52197458429825083, 37.50933785548062360, 34.80090346875805096 ) ) ;
#29348 = CARTESIAN_POINT ( 'NONE',  ( -7.075845757273814415E-16, 80.00000000000000000, 15.49999999999998757 ) ) ;
#29349 = CARTESIAN_POINT ( 'NONE',  ( 0.01899995639453812973, 7.352259170992722304, -5.265513565426382492 ) ) ;
#29350 = CARTESIAN_POINT ( 'NONE',  ( -11.39115782160862977, -40.65273190043797058, 29.00210455454194047 ) ) ;
#29351 = ORIENTED_EDGE ( 'NONE', *, *, #11073, .T. ) ;
#29352 = CARTESIAN_POINT ( 'NONE',  ( -24.75988009833579184, -7.043597625963917253, 49.25816067347040672 ) ) ;
#29353 = DIRECTION ( 'NONE',  ( 1.000000000000000000, 0.000000000000000000, 0.000000000000000000 ) ) ;
#29354 = CIRCLE ( 'NONE', #9934, 1.447898107987198646 ) ;
#29355 = CARTESIAN_POINT ( 'NONE',  ( -15.81542570303655637, 12.27127866024201985, 18.64703902303423178 ) ) ;
#29356 = AXIS2_PLACEMENT_3D ( 'NONE', #21753, #22219, #854 ) ;
#29357 = DIRECTION ( 'NONE',  ( 1.000000000000000000, 0.000000000000000000, 0.000000000000000000 ) ) ;
#29358 = VERTEX_POINT ( 'NONE', #3181 ) ;
#29359 = CARTESIAN_POINT ( 'NONE',  ( 28.10944024216546211, -29.46071976086648192, 11.88312378939523306 ) ) ;
#29360 = CARTESIAN_POINT ( 'NONE',  ( -40.00000000000000000, 63.74772708486752038, 62.49999999999999289 ) ) ;
#29361 = CARTESIAN_POINT ( 'NONE',  ( -6.187077094091591789, 11.47693674426096955, 1.500000000000001332 ) ) ;
#29362 = DIRECTION ( 'NONE',  ( 1.000000000000000000, 0.000000000000000000, 0.000000000000000000 ) ) ;
#29363 = CARTESIAN_POINT ( 'NONE',  ( -12.56641067637617759, -40.32935944494947478, -1.500000000000000000 ) ) ;
#29364 = VECTOR ( 'NONE', #11707, 1000.000000000000000 ) ;
#29365 = FACE_BOUND ( 'NONE', #13447, .T. ) ;
#29366 = CARTESIAN_POINT ( 'NONE',  ( 16.56282882398535250, 33.64935822775603924, 37.49999999998171063 ) ) ;
#29367 = CARTESIAN_POINT ( 'NONE',  ( 19.56075217167572688, 4.168887357664727844, 6.392525840300342210 ) ) ;
#29368 = ORIENTED_EDGE ( 'NONE', *, *, #26350, .F. ) ;
#29369 = DIRECTION ( 'NONE',  ( 0.000000000000000000, 0.000000000000000000, 1.000000000000000000 ) ) ;
#29370 = CARTESIAN_POINT ( 'NONE',  ( -24.02316098943739675, -13.21662147465773707, 43.33855891335688426 ) ) ;
#29371 = DIRECTION ( 'NONE',  ( 0.000000000000000000, 0.000000000000000000, 1.000000000000000000 ) ) ;
#29372 = VERTEX_POINT ( 'NONE', #3328 ) ;
#29373 = ORIENTED_EDGE ( 'NONE', *, *, #1783, .F. ) ;
#29374 = DIRECTION ( 'NONE',  ( 0.9096319953545183301, 0.4154150130018865461, 0.000000000000000000 ) ) ;
#29375 = ADVANCED_FACE ( 'NONE', ( #12549 ), #29857, .F. ) ;
#29376 = ORIENTED_EDGE ( 'NONE', *, *, #16255, .T. ) ;
#29377 = DIRECTION ( 'NONE',  ( -0.000000000000000000, -0.000000000000000000, -1.000000000000000000 ) ) ;
#29378 = CARTESIAN_POINT ( 'NONE',  ( -34.70577939416727276, 10.49309206033987785, 34.49999999999999289 ) ) ;
#29379 = CARTESIAN_POINT ( 'NONE',  ( 3.395021109945009385, -30.50000000000000711, 1.500000000000000222 ) ) ;
#29380 = CARTESIAN_POINT ( 'NONE',  ( -36.41962120944751291, 15.21524643282687350, 9.352698495745318752 ) ) ;
#29381 = VECTOR ( 'NONE', #1782, 1000.000000000000000 ) ;
#29382 = EDGE_CURVE ( 'NONE', #11001, #20003, #11873, .T. ) ;
#29383 = DIRECTION ( 'NONE',  ( -0.000000000000000000, 1.000000000000000000, -0.000000000000000000 ) ) ;
#29384 = ORIENTED_EDGE ( 'NONE', *, *, #24439, .T. ) ;
#29385 = EDGE_CURVE ( 'NONE', #10771, #24660, #15168, .T. ) ;
#29386 = CARTESIAN_POINT ( 'NONE',  ( 3.896869771148438577, -16.82098518409776489, 24.50000000000000000 ) ) ;
#29387 = DIRECTION ( 'NONE',  ( -1.369518533665900065E-16, 0.000000000000000000, -1.000000000000000000 ) ) ;
#29388 = DIRECTION ( 'NONE',  ( -0.000000000000000000, -0.000000000000000000, 1.000000000000000000 ) ) ;
#29389 = FACE_OUTER_BOUND ( 'NONE', #352, .T. ) ;
#29390 = ORIENTED_EDGE ( 'NONE', *, *, #11644, .T. ) ;
#29391 = AXIS2_PLACEMENT_3D ( 'NONE', #536, #7883, #26601 ) ;
#29392 = CARTESIAN_POINT ( 'NONE',  ( -11.35279153858833290, -16.48728705952963480, 19.56050940960062690 ) ) ;
#29393 = CARTESIAN_POINT ( 'NONE',  ( -17.96415918337694251, -8.831719996762307900, 7.627891251804737927 ) ) ;
#29394 = CARTESIAN_POINT ( 'NONE',  ( -6.587417658830999834, 18.90298706665743822, 5.872146474157316831 ) ) ;
#29395 = CARTESIAN_POINT ( 'NONE',  ( -3.515970705488605130, 17.06554576617236307, 1.500000000000000000 ) ) ;
#29396 = CARTESIAN_POINT ( 'NONE',  ( 1.000000000000008438, 15.73749217771910125, 1.500000000000001332 ) ) ;
#29397 = DIRECTION ( 'NONE',  ( 0.6548607339452782172, -0.7557495743542642641, 0.000000000000000000 ) ) ;
#29398 = VERTEX_POINT ( 'NONE', #17525 ) ;
#29399 = ORIENTED_EDGE ( 'NONE', *, *, #21972, .F. ) ;
#29400 = DIRECTION ( 'NONE',  ( -0.000000000000000000, 1.132880637372608986E-16, -1.000000000000000000 ) ) ;
#29401 = CARTESIAN_POINT ( 'NONE',  ( -5.196396160405778453, 19.31337320890706266, 19.96302680909623462 ) ) ;
#29402 = EDGE_CURVE ( 'NONE', #20812, #3530, #5904, .T. ) ;
#29403 = CARTESIAN_POINT ( 'NONE',  ( 15.41296542101254552, 5.939519782021115191, -0.6213203435596476032 ) ) ;
#29404 = EDGE_CURVE ( 'NONE', #28377, #7591, #24857, .T. ) ;
#29405 = CARTESIAN_POINT ( 'NONE',  ( 0.1595703638607181285, -17.02896808597062162, 7.453286057244485008 ) ) ;
#29406 = EDGE_LOOP ( 'NONE', ( #13427, #10558, #20851, #6163 ) ) ;
#29407 = CONTEXT_DEPENDENT_SHAPE_REPRESENTATION ( #18377, #16902 ) ;
#29408 = AXIS2_PLACEMENT_3D ( 'NONE', #8011, #24674, #14044 ) ;
#29409 = CARTESIAN_POINT ( 'NONE',  ( -11.40980092660686829, 6.310027164379044429, 1.500000000000001332 ) ) ;
#29410 = EDGE_CURVE ( 'NONE', #12825, #30078, #2433, .T. ) ;
#29411 = CARTESIAN_POINT ( 'NONE',  ( -20.71335220384823117, -27.86167394782616213, -6.500000000000000888 ) ) ;
#29412 = ORIENTED_EDGE ( 'NONE', *, *, #16087, .T. ) ;
#29413 = CARTESIAN_POINT ( 'NONE',  ( 5.298970182598334411, 19.30368537022594211, 18.34798005862930026 ) ) ;
#29414 = EDGE_CURVE ( 'NONE', #23905, #28303, #11344, .T. ) ;
#29415 = CARTESIAN_POINT ( 'NONE',  ( 29.99999999999925038, 1.387778780781445676E-14, 67.49999999999997158 ) ) ;
#29416 = CARTESIAN_POINT ( 'NONE',  ( -32.07676738547140616, -24.18760485068483135, 34.63128111633764661 ) ) ;
#29417 = CIRCLE ( 'NONE', #2512, 12.18947652193948272 ) ;
#29418 = ORIENTED_EDGE ( 'NONE', *, *, #19819, .F. ) ;
#29419 = EDGE_CURVE ( 'NONE', #10573, #357, #12139, .T. ) ;
#29420 = DIRECTION ( 'NONE',  ( 0.000000000000000000, 0.000000000000000000, -1.000000000000000000 ) ) ;
#29421 = ADVANCED_FACE ( 'NONE', ( #21855 ), #21219, .F. ) ;
#29422 = CARTESIAN_POINT ( 'NONE',  ( 49.99999999999998579, 70.00000000000000000, -92.50000000000000000 ) ) ;
#29423 = DIRECTION ( 'NONE',  ( -0.000000000000000000, -0.000000000000000000, 1.000000000000000000 ) ) ;
#29424 = ORIENTED_EDGE ( 'NONE', *, *, #13176, .F. ) ;
#29425 = LINE ( 'NONE', #27229, #1862 ) ;
#29426 = CARTESIAN_POINT ( 'NONE',  ( 12.53355205340454681, 11.54212474482388195, 20.32222155561919408 ) ) ;
#29427 = CARTESIAN_POINT ( 'NONE',  ( -7.663215745754974328, 3.196529495465474380, 21.50000000000000000 ) ) ;
#29428 = CARTESIAN_POINT ( 'NONE',  ( -57.50000000000001421, 50.00000000000000000, 12.49999999999999112 ) ) ;
#29429 = AXIS2_PLACEMENT_3D ( 'NONE', #9647, #16820, #14476 ) ;
#29430 = CARTESIAN_POINT ( 'NONE',  ( -37.99999999999999289, 70.00000000000000000, -87.50000000000000000 ) ) ;
#29431 = DIRECTION ( 'NONE',  ( 0.000000000000000000, -0.8682431421244592995, -0.4961389383568337030 ) ) ;
#29432 = CARTESIAN_POINT ( 'NONE',  ( 37.38490933374808378, -12.10749625520922024, 10.61420996327511723 ) ) ;
#29433 = CARTESIAN_POINT ( 'NONE',  ( 0.000000000000000000, 90.00000000000001421, -55.00000000000000711 ) ) ;
#29434 = ORIENTED_EDGE ( 'NONE', *, *, #12994, .F. ) ;
#29435 = ADVANCED_FACE ( 'NONE', ( #9690, #2366 ), #7520, .T. ) ;
#29436 = DIRECTION ( 'NONE',  ( -0.000000000000000000, -0.000000000000000000, -1.000000000000000000 ) ) ;
#29437 = CARTESIAN_POINT ( 'NONE',  ( 4.434078574240013282, 19.50234843602376955, 6.149077423860704883 ) ) ;
#29438 = VERTEX_POINT ( 'NONE', #19366 ) ;
#29439 = ORIENTED_EDGE ( 'NONE', *, *, #8805, .F. ) ;
#29440 = CARTESIAN_POINT ( 'NONE',  ( 1.073881485057758711, -0.9711784013061475207, 1.500000000000000000 ) ) ;
#29441 = ADVANCED_FACE ( 'NONE', ( #26540 ), #17018, .F. ) ;
#29442 = CARTESIAN_POINT ( 'NONE',  ( 0.000000000000000000, 7.794228634059939154, 4.500000000000010658 ) ) ;
#29443 = EDGE_CURVE ( 'NONE', #23362, #5775, #26340, .T. ) ;
#29444 = CARTESIAN_POINT ( 'NONE',  ( -35.99780421875948377, -2.509863319654308089, 27.50000000000000000 ) ) ;
#29445 = CARTESIAN_POINT ( 'NONE',  ( 12.38084545251366642, 11.71426794001388316, 18.34777357837152323 ) ) ;
#29446 = ORIENTED_EDGE ( 'NONE', *, *, #14922, .F. ) ;
#29447 = ORIENTED_EDGE ( 'NONE', *, *, #26444, .T. ) ;
#29448 = DIRECTION ( 'NONE',  ( 1.000000000000000000, 0.000000000000000000, 0.000000000000000000 ) ) ;
#29449 = AXIS2_PLACEMENT_3D ( 'NONE', #12545, #22036, #10041 ) ;
#29450 = CARTESIAN_POINT ( 'NONE',  ( 18.33793066653144521, -7.982499537706466697, 5.652196082369965069 ) ) ;
#29451 = AXIS2_PLACEMENT_3D ( 'NONE', #19779, #29147, #29466 ) ;
#29452 = CARTESIAN_POINT ( 'NONE',  ( 40.48994520213110349, 2.927201920381877542, -16.49999999999999645 ) ) ;
#29453 =( BOUNDED_CURVE ( )  B_SPLINE_CURVE ( 3, ( #5866, #13197, #13050, #3369 ),
 .UNSPECIFIED., .F., .T. ) 
 B_SPLINE_CURVE_WITH_KNOTS ( ( 4, 4 ),
 ( 5.540737561276206868, 5.872433067142492469 ),
 .UNSPECIFIED. ) 
 CURVE ( )  GEOMETRIC_REPRESENTATION_ITEM ( )  RATIONAL_B_SPLINE_CURVE ( ( 1.000000000000000000, 0.9908525036704132205, 0.9908525036704132205, 1.000000000000000000 ) ) 
 REPRESENTATION_ITEM ( '' )  );
#29454 = EDGE_LOOP ( 'NONE', ( #27264, #18173, #15970, #1962 ) ) ;
#29455 = DIRECTION ( 'NONE',  ( -0.000000000000000000, -0.000000000000000000, 1.000000000000000000 ) ) ;
#29456 = ORIENTED_EDGE ( 'NONE', *, *, #22521, .F. ) ;
#29457 = DIRECTION ( 'NONE',  ( -0.000000000000000000, -0.000000000000000000, 1.000000000000000000 ) ) ;
#29458 = EDGE_LOOP ( 'NONE', ( #20017, #20185, #21488, #30674 ) ) ;
#29459 = B_SPLINE_CURVE_WITH_KNOTS ( 'NONE', 3,
 ( #1169, #20645, #1321, #10676 ),
 .UNSPECIFIED., .F., .F.,
 ( 4, 4 ),
 ( 3.018024802580205417E-07, 0.007932103453629116285 ),
 .UNSPECIFIED. ) ;
#29460 =( NAMED_UNIT ( * ) SI_UNIT ( $, .STERADIAN. ) SOLID_ANGLE_UNIT ( ) );
#29461 = CARTESIAN_POINT ( 'NONE',  ( 29.78057599403043909, 27.44970389380054243, 30.31536403417277015 ) ) ;
#29462 = CARTESIAN_POINT ( 'NONE',  ( 19.60578376704636483, 4.040313317649105507, 7.196036389296800451 ) ) ;
#29463 = CARTESIAN_POINT ( 'NONE',  ( -15.28428954155913289, 12.92682542062231121, 18.35377592296120497 ) ) ;
#29464 = DIRECTION ( 'NONE',  ( -1.000000000000000000, 0.000000000000000000, 0.000000000000000000 ) ) ;
#29465 = CARTESIAN_POINT ( 'NONE',  ( -35.59958042135278333, -17.54967582489527445, 31.31518679243729864 ) ) ;
#29466 = DIRECTION ( 'NONE',  ( 1.000000000000000000, 0.000000000000000000, 0.000000000000000000 ) ) ;
#29467 = CARTESIAN_POINT ( 'NONE',  ( -29.61203839202723032, -15.40012917324033381, 41.62281023987518580 ) ) ;
#29468 = ORIENTED_EDGE ( 'NONE', *, *, #29627, .T. ) ;
#29469 = EDGE_CURVE ( 'NONE', #17832, #14781, #4550, .T. ) ;
#29470 = CARTESIAN_POINT ( 'NONE',  ( 9.186411229153641500, -14.33460949872162260, 7.272049892295485485 ) ) ;
#29471 = EDGE_CURVE ( 'NONE', #11152, #21957, #11726, .T. ) ;
#29472 = DIRECTION ( 'NONE',  ( 1.000000000000000000, 0.000000000000000000, 0.000000000000000000 ) ) ;
#29473 = VECTOR ( 'NONE', #1461, 1000.000000000000000 ) ;
#29474 = DIRECTION ( 'NONE',  ( 0.2817325568414296710, -0.9594929736144973687, 0.000000000000000000 ) ) ;
#29475 = ORIENTED_EDGE ( 'NONE', *, *, #16409, .F. ) ;
#29476 = ORIENTED_EDGE ( 'NONE', *, *, #9431, .T. ) ;
#29477 = CARTESIAN_POINT ( 'NONE',  ( 18.28362707703099233, -8.107168301167737567, 20.34789198813115618 ) ) ;
#29478 = CARTESIAN_POINT ( 'NONE',  ( 7.500000000000000000, 1.102182119232617714E-15, -9.000000000000000000 ) ) ;
#29479 = LINE ( 'NONE', #19341, #8384 ) ;
#29480 = ORIENTED_EDGE ( 'NONE', *, *, #29543, .T. ) ;
#29481 = FACE_OUTER_BOUND ( 'NONE', #11815, .T. ) ;
#29482 = DIRECTION ( 'NONE',  ( -0.000000000000000000, 0.000000000000000000, 1.000000000000000000 ) ) ;
#29483 = DIRECTION ( 'NONE',  ( -0.000000000000000000, -0.000000000000000000, -1.000000000000000000 ) ) ;
#29484 = EDGE_LOOP ( 'NONE', ( #4789, #7368 ) ) ;
#29485 = AXIS2_PLACEMENT_3D ( 'NONE', #30701, #14484, #26351 ) ;
#29486 = CARTESIAN_POINT ( 'NONE',  ( -8.999114229549592281, 0.1262659238205133538, -1.500000000000001776 ) ) ;
#29487 = CARTESIAN_POINT ( 'NONE',  ( 14.59199839715917513, 13.70371665158259766, 5.749491821935610147 ) ) ;
#29488 = CARTESIAN_POINT ( 'NONE',  ( 16.84421249428844192, 2.491431357970654403, 5.940635272151477686 ) ) ;
#29489 = ORIENTED_EDGE ( 'NONE', *, *, #3298, .F. ) ;
#29490 = CARTESIAN_POINT ( 'NONE',  ( -16.65122935894506639, -13.93942108199812324, 1.500000000000000000 ) ) ;
#29491 = ORIENTED_EDGE ( 'NONE', *, *, #29469, .F. ) ;
#29492 = CARTESIAN_POINT ( 'NONE',  ( 3.395021109945021376, 30.50000000000000000, 1.500000000000001332 ) ) ;
#29493 = FACE_OUTER_BOUND ( 'NONE', #9490, .T. ) ;
#29494 = CIRCLE ( 'NONE', #6579, 9.482273699623480212 ) ;
#29495 = ORIENTED_EDGE ( 'NONE', *, *, #27404, .T. ) ;
#29496 = CARTESIAN_POINT ( 'NONE',  ( 3.122919890997790215, 16.78802993858288772, 6.995624166085161910 ) ) ;
#29497 = CYLINDRICAL_SURFACE ( 'NONE', #22610, 3.000000000000002665 ) ;
#29498 = DIRECTION ( 'NONE',  ( 1.000000000000000000, 0.000000000000000000, 0.000000000000000000 ) ) ;
#29499 = DIRECTION ( 'NONE',  ( 1.000000000000000000, 0.000000000000000000, 0.000000000000000000 ) ) ;
#29500 = CARTESIAN_POINT ( 'NONE',  ( 0.000000000000000000, 39.50000000000000000, 34.80090346875804386 ) ) ;
#29501 = CARTESIAN_POINT ( 'NONE',  ( 10.25620417238948257, -17.19090129355371488, 19.33715507985239412 ) ) ;
#29502 = CARTESIAN_POINT ( 'NONE',  ( 32.06725342158286907, 14.54034564589948531, 39.79052675593687383 ) ) ;
#29503 = VERTEX_POINT ( 'NONE', #5641 ) ;
#29504 = CIRCLE ( 'NONE', #16051, 0.7500000000000006661 ) ;
#29505 = CARTESIAN_POINT ( 'NONE',  ( 24.75988009833579540, 7.043597625963922582, 49.25816067347034277 ) ) ;
#29506 = CARTESIAN_POINT ( 'NONE',  ( -15.94999985682714971, 12.09556989559485629, 19.69140814234746273 ) ) ;
#29507 = CARTESIAN_POINT ( 'NONE',  ( 33.55235357430897380, 10.58403138555777900, 35.57544210944276841 ) ) ;
#29508 = DIRECTION ( 'NONE',  ( -0.000000000000000000, -0.000000000000000000, -1.000000000000000000 ) ) ;
#29509 = ORIENTED_EDGE ( 'NONE', *, *, #2301, .F. ) ;
#29510 = EDGE_CURVE ( 'NONE', #29358, #1662, #10308, .T. ) ;
#29511 = DIRECTION ( 'NONE',  ( 0.000000000000000000, 0.000000000000000000, 1.000000000000000000 ) ) ;
#29512 = CARTESIAN_POINT ( 'NONE',  ( -46.52886832597424416, 69.65281066659318299, 60.08552421216484873 ) ) ;
#29513 = DIRECTION ( 'NONE',  ( 0.000000000000000000, 0.000000000000000000, 1.000000000000000000 ) ) ;
#29514 = CYLINDRICAL_SURFACE ( 'NONE', #1813, 0.7500000000000003331 ) ;
#29515 = DIRECTION ( 'NONE',  ( 0.000000000000000000, -1.000000000000000000, 0.000000000000000000 ) ) ;
#29516 = B_SPLINE_CURVE_WITH_KNOTS ( 'NONE', 3,
 ( #15181, #12877, #5845, #22376, #6146, #24875, #10671, #20177, #20030, #13172, #22665, #22512, #15652, #25165 ),
 .UNSPECIFIED., .F., .F.,
 ( 4, 2, 2, 2, 2, 2, 4 ),
 ( 2.111077618484504239E-07, 0.0004668847438969953110, 0.0009335583800321421710, 0.001400232016167289248, 0.001866905652302435891, 0.002800252924572717468, 0.003733600196842999479 ),
 .UNSPECIFIED. ) ;
#29517 = CARTESIAN_POINT ( 'NONE',  ( -22.58267429318970443, -26.57182937991348481, -6.499999999999999112 ) ) ;
#29518 = CARTESIAN_POINT ( 'NONE',  ( 14.99999999999995737, 1.387778780781445676E-14, 77.49999999999998579 ) ) ;
#29519 = ORIENTED_EDGE ( 'NONE', *, *, #5159, .F. ) ;
#29520 = CARTESIAN_POINT ( 'NONE',  ( 25.18096005886327760, 6.640581704039639988, 44.71664046397091852 ) ) ;
#29521 = CARTESIAN_POINT ( 'NONE',  ( -19.50000000000000711, 1.387778780781445676E-14, 62.49999999999999289 ) ) ;
#29522 = DIRECTION ( 'NONE',  ( -1.000000000000000000, -0.000000000000000000, 0.000000000000000000 ) ) ;
#29523 = ORIENTED_EDGE ( 'NONE', *, *, #23115, .F. ) ;
#29524 = VECTOR ( 'NONE', #8265, 1000.000000000000000 ) ;
#29525 = VECTOR ( 'NONE', #12186, 1000.000000000000000 ) ;
#29526 = ORIENTED_EDGE ( 'NONE', *, *, #30153, .T. ) ;
#29527 = CARTESIAN_POINT ( 'NONE',  ( -9.471281197126605989, -0.4564504349074081091, 13.00000000000000178 ) ) ;
#29528 = AXIS2_PLACEMENT_3D ( 'NONE', #19787, #29317, #19954 ) ;
#29529 = ORIENTED_EDGE ( 'NONE', *, *, #27520, .T. ) ;
#29530 = CARTESIAN_POINT ( 'NONE',  ( 0.7836603915001300047, -17.02734626464551226, 18.34798005862930381 ) ) ;
#29531 = CARTESIAN_POINT ( 'NONE',  ( -27.82441128074781744, 25.08107326869593479, 34.50000000000000000 ) ) ;
#29532 = CARTESIAN_POINT ( 'NONE',  ( -37.86695649773925965, 10.17204804043823962, 14.12367837669096460 ) ) ;
#29533 = CARTESIAN_POINT ( 'NONE',  ( 12.86767874445214055, -1.850092897552706894, 24.50000000000000000 ) ) ;
#29534 = CARTESIAN_POINT ( 'NONE',  ( -33.42925964089141644, -11.06161099612212695, 39.78814634291941843 ) ) ;
#29535 = LINE ( 'NONE', #8172, #14600 ) ;
#29536 = CARTESIAN_POINT ( 'NONE',  ( 14.67322144252663918, 13.61684651386558542, 20.29915277494337644 ) ) ;
#29537 = CARTESIAN_POINT ( 'NONE',  ( -16.46198811862381817, -1.356593340923033075, -0.6213203435596476032 ) ) ;
#29538 = EDGE_LOOP ( 'NONE', ( #18129, #16956, #22479, #12810 ) ) ;
#29539 = CARTESIAN_POINT ( 'NONE',  ( -11.35443157991641172, -16.48616348260577524, 19.11611934778430921 ) ) ;
#29540 = DIRECTION ( 'NONE',  ( 0.000000000000000000, -1.132880637372608986E-16, 1.000000000000000000 ) ) ;
#29541 = CARTESIAN_POINT ( 'NONE',  ( -6.116198564155505224, 19.06064343544019835, 7.643931100913408550 ) ) ;
#29542 = VECTOR ( 'NONE', #21894, 1000.000000000000000 ) ;
#29543 = EDGE_CURVE ( 'NONE', #17560, #22179, #24345, .T. ) ;
#29544 = CARTESIAN_POINT ( 'NONE',  ( 10.30429258806635495, -13.59853737800767881, 7.500147780736496017 ) ) ;
#29545 = EDGE_CURVE ( 'NONE', #20124, #7938, #7919, .T. ) ;
#29546 = AXIS2_PLACEMENT_3D ( 'NONE', #4290, #9131, #18651 ) ;
#29547 = CARTESIAN_POINT ( 'NONE',  ( 25.19442432474404470, 35.44676296256560022, -19.50000000000000355 ) ) ;
#29548 = CYLINDRICAL_SURFACE ( 'NONE', #2639, 0.7499999999999997780 ) ;
#29549 = ORIENTED_EDGE ( 'NONE', *, *, #187, .T. ) ;
#29550 = VERTEX_POINT ( 'NONE', #2993 ) ;
#29551 = DIRECTION ( 'NONE',  ( 0.000000000000000000, -0.000000000000000000, -1.000000000000000000 ) ) ;
#29552 = CARTESIAN_POINT ( 'NONE',  ( -2.687479363073305372, 44.39187623477332068, -19.50000000000000355 ) ) ;
#29553 = CARTESIAN_POINT ( 'NONE',  ( -12.86036580545043684, 11.15762522838069337, 6.018569869498933578 ) ) ;
#29554 = LINE ( 'NONE', #26604, #1633 ) ;
#29555 = ORIENTED_EDGE ( 'NONE', *, *, #12419, .F. ) ;
#29556 = ITEM_DEFINED_TRANSFORMATION ( 'NONE', 'NONE', #30321,  #7396 ) ;
#29557 = DIRECTION ( 'NONE',  ( 0.000000000000000000, -0.000000000000000000, -1.000000000000000000 ) ) ;
#29558 = ADVANCED_FACE ( 'NONE', ( #5788 ), #12666, .F. ) ;
#29559 = VERTEX_POINT ( 'NONE', #20134 ) ;
#29560 = FACE_BOUND ( 'NONE', #17550, .T. ) ;
#29561 = B_SPLINE_SURFACE_WITH_KNOTS ( 'NONE', 3, 1, ( 
 ( #20094, #10899 ),
 ( #18069, #15563 ),
 ( #15235, #24928 ),
 ( #17920, #1230 ),
 ( #3244, #29612 ),
 ( #3725, #22114 ),
 ( #3409, #29766 ),
 ( #3879, #12768 ),
 ( #22428, #20404 ),
 ( #10732, #22728 ),
 ( #10430, #5902 ),
 ( #8408, #8245 ),
 ( #27585, #26974 ),
 ( #13240, #6211 ),
 ( #24763, #741 ),
 ( #15714, #17751 ),
 ( #20242, #22269 ),
 ( #1385, #10260 ),
 ( #19774, #27271 ),
 ( #913, #5598 ),
 ( #29462, #15093 ),
 ( #29306, #7947 ),
 ( #17452, #15403 ),
 ( #5743, #8096 ),
 ( #1072, #10582 ),
 ( #3564, #27120 ),
 ( #13087, #25399 ),
 ( #20997, #9161 ),
 ( #4170, #8709 ),
 ( #23184, #20549 ),
 ( #9311, #15883 ) ),
 .UNSPECIFIED., .F., .F., .F.,
 ( 4, 3, 3, 3, 3, 3, 3, 3, 3, 3, 4 ),
 ( 2, 2 ),
 ( 0.4999999998345681651, 0.5360336730431942698, 0.5907651151589017324, 0.6456034593241839481, 0.6998270958050443191, 0.7529536536315944995, 0.8052385063053264513, 0.8575343587103996246, 0.9106564858195047574, 0.9648414833209688624, 1.000000006602610014 ),
 ( 0.000000000000000000, 1.000000000000000000 ),
 .UNSPECIFIED. ) ;
#29562 = CIRCLE ( 'NONE', #7159, 1.447898107987170890 ) ;
#29563 = CARTESIAN_POINT ( 'NONE',  ( 8.260402557893151254, 8.184276679720483116, 1.500000000000000000 ) ) ;
#29564 = CARTESIAN_POINT ( 'NONE',  ( -38.03082308345415896, -9.438271779104216108, 31.93948111368219500 ) ) ;
#29565 = VERTEX_POINT ( 'NONE', #5484 ) ;
#29566 = CARTESIAN_POINT ( 'NONE',  ( 11.11118388262826251, -16.62953976291647962, 5.652196082369964181 ) ) ;
#29567 = AXIS2_PLACEMENT_3D ( 'NONE', #24941, #3579, #27909 ) ;
#29568 = CIRCLE ( 'NONE', #8157, 4.999999999999997335 ) ;
#29569 = LINE ( 'NONE', #866, #23985 ) ;
#29570 = DIRECTION ( 'NONE',  ( 1.000000000000000000, 0.000000000000000000, 0.000000000000000000 ) ) ;
#29571 = CYLINDRICAL_SURFACE ( 'NONE', #12855, 20.00000000000000000 ) ;
#29572 = VERTEX_POINT ( 'NONE', #7820 ) ;
#29573 = CARTESIAN_POINT ( 'NONE',  ( -18.07538971572904174, -8.601943808150394943, 5.651989602109218858 ) ) ;
#29574 = CARTESIAN_POINT ( 'NONE',  ( 29.61203839202723032, 15.40012917324034092, 37.38016955275583797 ) ) ;
#29575 = EDGE_CURVE ( 'NONE', #20986, #10442, #7989, .T. ) ;
#29576 = EDGE_CURVE ( 'NONE', #17226, #10643, #5418, .T. ) ;
#29577 = CYLINDRICAL_SURFACE ( 'NONE', #28212, 0.7500000000000006661 ) ;
#29578 = DIRECTION ( 'NONE',  ( 0.000000000000000000, -1.132880637372608986E-16, 1.000000000000000000 ) ) ;
#29579 = FACE_OUTER_BOUND ( 'NONE', #26426, .T. ) ;
#29580 = DIRECTION ( 'NONE',  ( -0.000000000000000000, -0.000000000000000000, 1.000000000000000000 ) ) ;
#29581 = PLANE ( 'NONE',  #20877 ) ;
#29582 = ORIENTED_EDGE ( 'NONE', *, *, #23852, .T. ) ;
#29583 = EDGE_CURVE ( 'NONE', #22741, #10498, #17644, .T. ) ;
#29584 = DIRECTION ( 'NONE',  ( 1.000000000000000000, 0.000000000000000000, 0.000000000000000000 ) ) ;
#29585 = CARTESIAN_POINT ( 'NONE',  ( 4.335955696074043075, 19.52440042691175393, 6.919864475265786297 ) ) ;
#29586 = ORIENTED_EDGE ( 'NONE', *, *, #1601, .F. ) ;
#29587 = EDGE_LOOP ( 'NONE', ( #1700, #18544, #17395, #22930 ) ) ;
#29588 = DIRECTION ( 'NONE',  ( -0.000000000000000000, -0.000000000000000000, -1.000000000000000000 ) ) ;
#29589 = CARTESIAN_POINT ( 'NONE',  ( -25.19442432475474902, -35.44676296258422354, -19.50000000000000355 ) ) ;
#29590 = EDGE_CURVE ( 'NONE', #8115, #20027, #30366, .T. ) ;
#29591 = CARTESIAN_POINT ( 'NONE',  ( -1.967529318552797335, 49.96369992636662971, -69.87862445765860286 ) ) ;
#29592 = CIRCLE ( 'NONE', #16137, 9.482273699623480212 ) ;
#29593 = FACE_OUTER_BOUND ( 'NONE', #18900, .T. ) ;
#29594 = EDGE_CURVE ( 'NONE', #17335, #8993, #3452, .T. ) ;
#29595 = CARTESIAN_POINT ( 'NONE',  ( 15.54774248266353176, 12.60889669900781129, 19.22654678686458141 ) ) ;
#29596 = ADVANCED_FACE ( 'NONE', ( #17170 ), #711, .T. ) ;
#29597 = ORIENTED_EDGE ( 'NONE', *, *, #9045, .T. ) ;
#29598 = VERTEX_POINT ( 'NONE', #20727 ) ;
#29599 = CARTESIAN_POINT ( 'NONE',  ( 15.87141697993282463, -6.228091237695521976, 20.33971507717571114 ) ) ;
#29600 = CARTESIAN_POINT ( 'NONE',  ( 18.23136487193859523, -8.223889151412006271, 5.676722608126685721 ) ) ;
#29601 = DIRECTION ( 'NONE',  ( 0.000000000000000000, 0.000000000000000000, -1.000000000000000000 ) ) ;
#29602 = ORIENTED_EDGE ( 'NONE', *, *, #21615, .T. ) ;
#29603 = CARTESIAN_POINT ( 'NONE',  ( 11.40980092660686118, 6.310027164379057751, 24.50000000000000000 ) ) ;
#29604 = ORIENTED_EDGE ( 'NONE', *, *, #20952, .T. ) ;
#29605 = CARTESIAN_POINT ( 'NONE',  ( 28.34828976096172681, -29.18752572968383419, 1.500000000000000000 ) ) ;
#29606 = ORIENTED_EDGE ( 'NONE', *, *, #19089, .T. ) ;
#29607 = AXIS2_PLACEMENT_3D ( 'NONE', #29326, #21983, #5464 ) ;
#29608 = EDGE_CURVE ( 'NONE', #22425, #4518, #30258, .T. ) ;
#29609 = DIRECTION ( 'NONE',  ( 1.000000000000000000, 0.000000000000000000, 0.000000000000000000 ) ) ;
#29610 = EDGE_CURVE ( 'NONE', #12232, #10944, #15996, .T. ) ;
#29611 = CARTESIAN_POINT ( 'NONE',  ( 8.795879380940563763, 2.270234684139707859, 13.22130136205108819 ) ) ;
#29612 = CARTESIAN_POINT ( 'NONE',  ( 16.68596330270456818, 3.532048315275338357, 5.704143890883081269 ) ) ;
#29613 = FACE_OUTER_BOUND ( 'NONE', #8237, .T. ) ;
#29614 = EDGE_CURVE ( 'NONE', #4424, #191, #22841, .T. ) ;
#29615 = CARTESIAN_POINT ( 'NONE',  ( 1.762690206872143728, -16.98588469933382683, 6.392658652357122051 ) ) ;
#29616 = CARTESIAN_POINT ( 'NONE',  ( -37.99999999999999289, 90.00000000000001421, -87.50000000000000000 ) ) ;
#29617 = DIRECTION ( 'NONE',  ( 0.000000000000000000, 1.132880637372608986E-16, -1.000000000000000000 ) ) ;
#29618 = PLANE ( 'NONE',  #30282 ) ;
#29619 = FACE_OUTER_BOUND ( 'NONE', #23955, .T. ) ;
#29620 = ADVANCED_FACE ( 'NONE', ( #14878 ), #16751, .T. ) ;
#29621 = CARTESIAN_POINT ( 'NONE',  ( 11.39819190923272529, -16.45610177916888262, 18.39992786714538298 ) ) ;
#29622 = LINE ( 'NONE', #17764, #29996 ) ;
#29623 = ORIENTED_EDGE ( 'NONE', *, *, #27112, .F. ) ;
#29624 = VERTEX_POINT ( 'NONE', #10199 ) ;
#29625 = CARTESIAN_POINT ( 'NONE',  ( 17.90972305382299368, -8.901787470106558686, 19.47728749465736797 ) ) ;
#29626 = CARTESIAN_POINT ( 'NONE',  ( -37.16608720827707657, 65.00000000000000000, 97.07879600563551037 ) ) ;
#29627 = EDGE_CURVE ( 'NONE', #22863, #18599, #26268, .T. ) ;
#29628 = CARTESIAN_POINT ( 'NONE',  ( 32.19782014694308003, -14.25394737442115201, 35.54550565580006349 ) ) ;
#29629 = ORIENTED_EDGE ( 'NONE', *, *, #20788, .F. ) ;
#29630 = DIRECTION ( 'NONE',  ( -0.000000000000000000, 0.000000000000000000, 1.000000000000000000 ) ) ;
#29631 =( BOUNDED_SURFACE ( )  B_SPLINE_SURFACE ( 3, 1, ( 
 ( #29118, #26944 ),
 ( #15063, #24577 ),
 ( #5103, #16952 ),
 ( #5415, #24277 ) ),
 .UNSPECIFIED., .F., .F., .T. ) 
 B_SPLINE_SURFACE_WITH_KNOTS ( ( 4, 4 ),
 ( 2, 2 ),
 ( 0.000000000000000000, 1.000000000000000000 ),
 ( 0.000000000000000000, 1.000000000000000000 ),
 .UNSPECIFIED. ) 
 GEOMETRIC_REPRESENTATION_ITEM ( )  RATIONAL_B_SPLINE_SURFACE ( (
 ( 1.000000000000000000, 1.000000000000000000),
 ( 0.3333333333333333703, 0.3333333333333333703),
 ( 0.3333333333333333703, 0.3333333333333333703),
 ( 1.000000000000000000, 1.000000000000000000) ) ) 
 REPRESENTATION_ITEM ( '' )  SURFACE ( )  );
#29632 = CARTESIAN_POINT ( 'NONE',  ( 49.99999999999998579, 50.00000000000000000, -87.50000000000000000 ) ) ;
#29633 = AXIS2_PLACEMENT_3D ( 'NONE', #12533, #2697, #19848 ) ;
#29634 = CARTESIAN_POINT ( 'NONE',  ( 5.888181818956391034, 19.11381997051147152, 5.849008070840538309 ) ) ;
#29635 = ORIENTED_EDGE ( 'NONE', *, *, #4058, .F. ) ;
#29636 = CARTESIAN_POINT ( 'NONE',  ( 26.44644203219471379, 9.801837641955973623, 1.500000000000000000 ) ) ;
#29637 = CARTESIAN_POINT ( 'NONE',  ( 14.20930976959225411, 14.09970620734104330, 6.447548852708279377 ) ) ;
#29638 = DIRECTION ( 'NONE',  ( -0.000000000000000000, -0.000000000000000000, -1.000000000000000000 ) ) ;
#29639 = VERTEX_POINT ( 'NONE', #26432 ) ;
#29640 = CARTESIAN_POINT ( 'NONE',  ( 16.69721919944051791, -13.88429941593332551, 1.500000000000000000 ) ) ;
#29641 = ORIENTED_EDGE ( 'NONE', *, *, #13909, .T. ) ;
#29642 = EDGE_CURVE ( 'NONE', #27365, #26376, #16876, .T. ) ;
#29643 = CARTESIAN_POINT ( 'NONE',  ( 25.48568755041062062, -12.36160011285429583, 1.500000000000001332 ) ) ;
#29644 = EDGE_CURVE ( 'NONE', #23566, #28062, #7093, .T. ) ;
#29645 = CARTESIAN_POINT ( 'NONE',  ( -8.824744466605359605, -8.513189541288717521, 1.500000000000001332 ) ) ;
#29646 = ORIENTED_EDGE ( 'NONE', *, *, #15630, .T. ) ;
#29647 = VERTEX_POINT ( 'NONE', #2877 ) ;
#29648 = FACE_OUTER_BOUND ( 'NONE', #20717, .T. ) ;
#29649 = CARTESIAN_POINT ( 'NONE',  ( 32.60641126234700238, 8.625635766581057240, 41.27204228840735567 ) ) ;
#29650 = CYLINDRICAL_SURFACE ( 'NONE', #7361, 9.482273699623480212 ) ;
#29651 = DIRECTION ( 'NONE',  ( -1.000000000000000000, 0.000000000000000000, 0.000000000000000000 ) ) ;
#29652 = CARTESIAN_POINT ( 'NONE',  ( 11.11463893384431323, -16.64861865631835158, 20.34789198813115263 ) ) ;
#29653 = CARTESIAN_POINT ( 'NONE',  ( 16.85539258114950556, 2.401441585233817566, 19.96783386855779341 ) ) ;
#29654 = ORIENTED_EDGE ( 'NONE', *, *, #8669, .F. ) ;
#29655 = CARTESIAN_POINT ( 'NONE',  ( -4.163336342344337027E-14, -1.387778780781445676E-14, 1.500000000000000000 ) ) ;
#29656 = CARTESIAN_POINT ( 'NONE',  ( 17.93514094173302453, -8.890850898656898593, 6.864725433338323413 ) ) ;
#29657 = CARTESIAN_POINT ( 'NONE',  ( -15.93537878762122872, 12.11488692681953694, 18.92976555901915603 ) ) ;
#29658 = CARTESIAN_POINT ( 'NONE',  ( 24.03057240117691862, 26.57182937991349903, -6.500000000000000888 ) ) ;
#29659 = DIRECTION ( 'NONE',  ( -0.7071067811865487940, -8.659560562354948882E-17, -0.7071067811865463515 ) ) ;
#29660 = ORIENTED_EDGE ( 'NONE', *, *, #836, .F. ) ;
#29661 = CARTESIAN_POINT ( 'NONE',  ( 28.74947044913098892, -28.71817798780287845, 15.65945394955731196 ) ) ;
#29662 = CARTESIAN_POINT ( 'NONE',  ( -44.92384265402849763, 68.80442260972010615, 61.21192266590395548 ) ) ;
#29663 = CARTESIAN_POINT ( 'NONE',  ( -23.59115238065502851, -12.85789229732232464, 48.13252386464831289 ) ) ;
#29664 =( LENGTH_UNIT ( ) NAMED_UNIT ( * ) SI_UNIT ( .MILLI., .METRE. ) );
#29665 = DIRECTION ( 'NONE',  ( -0.000000000000000000, -0.000000000000000000, -1.000000000000000000 ) ) ;
#29666 = VECTOR ( 'NONE', #15401, 1000.000000000000000 ) ;
#29667 = FACE_BOUND ( 'NONE', #20129, .T. ) ;
#29668 = CARTESIAN_POINT ( 'NONE',  ( 7.711002885858497358, 41.77047323054696193, 34.59400228303246649 ) ) ;
#29669 = DIRECTION ( 'NONE',  ( -0.000000000000000000, -0.000000000000000000, -1.000000000000000000 ) ) ;
#29670 = EDGE_LOOP ( 'NONE', ( #25505, #23375, #9200, #7637 ) ) ;
#29671 = DIRECTION ( 'NONE',  ( -1.000000000000000000, 0.000000000000000000, 0.000000000000000000 ) ) ;
#29672 = CARTESIAN_POINT ( 'NONE',  ( 0.000000000000000000, 0.000000000000000000, -6.500000000000000888 ) ) ;
#29673 = VERTEX_POINT ( 'NONE', #14424 ) ;
#29674 = AXIS2_PLACEMENT_3D ( 'NONE', #4562, #5180, #11906 ) ;
#29675 = EDGE_LOOP ( 'NONE', ( #17514, #12613, #444, #5894 ) ) ;
#29676 = DIRECTION ( 'NONE',  ( 0.000000000000000000, 0.000000000000000000, -1.000000000000000000 ) ) ;
#29677 = DIRECTION ( 'NONE',  ( -0.000000000000000000, -0.000000000000000000, -1.000000000000000000 ) ) ;
#29678 = EDGE_LOOP ( 'NONE', ( #22922, #25847, #18966, #14557 ) ) ;
#29679 = DIRECTION ( 'NONE',  ( 0.000000000000000000, -1.132880637372608986E-16, 1.000000000000000000 ) ) ;
#29680 = EDGE_CURVE ( 'NONE', #24939, #23193, #25340, .T. ) ;
#29681 = CARTESIAN_POINT ( 'NONE',  ( 1.962661427741273945, 49.96387296952570267, -69.87920469685937519 ) ) ;
#29682 = LINE ( 'NONE', #18459, #6535 ) ;
#29683 = DIRECTION ( 'NONE',  ( 0.9096319953545185522, -0.4154150130018859910, -0.000000000000000000 ) ) ;
#29684 = CARTESIAN_POINT ( 'NONE',  ( -20.50469103882543109, 27.17502484134975305, -16.50001200000000523 ) ) ;
#29685 = VECTOR ( 'NONE', #27511, 1000.000000000000000 ) ;
#29686 = CARTESIAN_POINT ( 'NONE',  ( -10.94076559809103699, -16.74260033555411553, 5.775318986477953942 ) ) ;
#29687 = CARTESIAN_POINT ( 'NONE',  ( 19.54426622602687402, -37.07991288358297055, 1.499999999999999778 ) ) ;
#29688 = CARTESIAN_POINT ( 'NONE',  ( 0.5064538767941907382, -20.01148730445865098, 5.661398277488801867 ) ) ;
#29689 = DIRECTION ( 'NONE',  ( -0.2972711322815274615, 0.9547931052914336858, 0.000000000000000000 ) ) ;
#29690 = ORIENTED_EDGE ( 'NONE', *, *, #12460, .T. ) ;
#29691 = FACE_OUTER_BOUND ( 'NONE', #16399, .T. ) ;
#29692 = CARTESIAN_POINT ( 'NONE',  ( -4.623640074070403116, 16.38233772743116390, 6.973843882838226094 ) ) ;
#29693 = VECTOR ( 'NONE', #29436, 1000.000000000000000 ) ;
#29694 = PLANE ( 'NONE',  #22739 ) ;
#29695 = CARTESIAN_POINT ( 'NONE',  ( 34.07766914600081520, 21.40380666527109810, -1.500000000000000000 ) ) ;
#29696 = CIRCLE ( 'NONE', #2277, 0.7500000000000006661 ) ;
#29697 = CARTESIAN_POINT ( 'NONE',  ( -23.11204206675364503, 35.56592873118525944, -11.49994521161821481 ) ) ;
#29698 = EDGE_LOOP ( 'NONE', ( #25222, #11131, #28474 ) ) ;
#29699 = ORIENTED_EDGE ( 'NONE', *, *, #7531, .F. ) ;
#29700 = APPLICATION_CONTEXT ( 'automotive_design' ) ;
#29701 = LINE ( 'NONE', #8345, #3450 ) ;
#29702 = CARTESIAN_POINT ( 'NONE',  ( 25.19442432473618254, -35.44676296258426618, -19.50000000000000355 ) ) ;
#29703 = CARTESIAN_POINT ( 'NONE',  ( -4.272706734781662519, -37.25579118953926638, 37.50000000000000000 ) ) ;
#29704 = DIRECTION ( 'NONE',  ( -1.000000000000000000, 0.000000000000000000, 0.000000000000000000 ) ) ;
#29705 = ORIENTED_EDGE ( 'NONE', *, *, #14737, .T. ) ;
#29706 = DIRECTION ( 'NONE',  ( 0.000000000000000000, -1.000000000000000000, 0.000000000000000000 ) ) ;
#29707 = VECTOR ( 'NONE', #1992, 1000.000000000000000 ) ;
#29708 = CARTESIAN_POINT ( 'NONE',  ( 25.19442432473618254, -35.44676296258426618, -19.50000000000000355 ) ) ;
#29709 = VECTOR ( 'NONE', #25292, 1000.000000000000000 ) ;
#29710 = ORIENTED_EDGE ( 'NONE', *, *, #789, .T. ) ;
#29711 = B_SPLINE_CURVE_WITH_KNOTS ( 'NONE', 3,
 ( #11689, #26035, #23675, #2321, #11848, #29350, #2486, #19022, #28532, #2634, #29146, #27124, #12477, #9975, #10113, #24144, #22273, #21968, #14952, #24463, #8249, #19623, #12938, #29465, #7781, #17291, #7951, #26825, #918, #15097, #10264, #17132, #26655, #10585, #24615, #22431, #5449, #457, #3107, #12626, #12311, #7626, #19778, #22117, #24768, #2961, #3247, #5748, #744, #24310, #29310, #12773, #598, #17455, #26978, #5604, #8100, #19479, #17757, #10434, #17606, #19948, #20099, #15239 ),
 .UNSPECIFIED., .F., .F.,
 ( 4, 2, 2, 2, 2, 2, 2, 2, 2, 2, 2, 2, 2, 2, 2, 2, 2, 2, 2, 2, 2, 2, 2, 2, 2, 2, 2, 2, 2, 2, 2, 4 ),
 ( 0.1344761468983755315, 0.1383589492301900981, 0.1403003503960973675, 0.1422417515620046369, 0.1500073562256337700, 0.1538901585574483366, 0.1558315597233556060, 0.1577729608892629032, 0.1655385655528919808, 0.1694213678847065196, 0.1713627690506138168, 0.1733041702165210862, 0.1810697748801501916, 0.1849525772119647304, 0.1888353795437792970, 0.1966009842074084024, 0.1985423853733156718, 0.2004837865392229690, 0.2043665888710375356, 0.2121321935346666410, 0.2160149958664812075, 0.2198977981982957464, 0.2237806005301102852, 0.2257220016960175824, 0.2276634028619248240, 0.2354290075255539016, 0.2393118098573684405, 0.2431946121891829793, 0.2509602168528121124, 0.2529016180187193541, 0.2548430191846266513, 0.2587258215164411901 ),
 .UNSPECIFIED. ) ;
#29712 = FACE_OUTER_BOUND ( 'NONE', #28515, .T. ) ;
#29713 = CARTESIAN_POINT ( 'NONE',  ( 19.65528207207771061, 3.699272045506084350, 18.47531940416305929 ) ) ;
#29714 = EDGE_LOOP ( 'NONE', ( #28697, #2580, #7248, #15179 ) ) ;
#29715 = CARTESIAN_POINT ( 'NONE',  ( 11.93908819109400099, -16.04550321516296663, 6.523620417364445423 ) ) ;
#29716 = AXIS2_PLACEMENT_3D ( 'NONE', #22398, #22237, #8370 ) ;
#29717 = LINE ( 'NONE', #22533, #12054 ) ;
#29718 = VECTOR ( 'NONE', #19763, 1000.000000000000000 ) ;
#29719 = DIRECTION ( 'NONE',  ( -0.000000000000000000, -0.000000000000000000, -1.000000000000000000 ) ) ;
#29720 = DIRECTION ( 'NONE',  ( -0.4154150130018840481, 0.9096319953545194403, 0.000000000000000000 ) ) ;
#29721 = ORIENTED_EDGE ( 'NONE', *, *, #30413, .F. ) ;
#29722 = DIRECTION ( 'NONE',  ( 0.000000000000000000, 0.000000000000000000, -1.000000000000000000 ) ) ;
#29723 = CARTESIAN_POINT ( 'NONE',  ( -2.446529495465445958, -8.413215745754985875, 21.50000000000000000 ) ) ;
#29724 = SURFACE_SIDE_STYLE ('',( #22541 ) ) ;
#29725 = DIRECTION ( 'NONE',  ( 1.000000000000000000, 0.000000000000000000, 0.000000000000000000 ) ) ;
#29726 = CARTESIAN_POINT ( 'NONE',  ( -49.99999999999998579, 90.00000000000001421, -75.50000000000002842 ) ) ;
#29727 = CARTESIAN_POINT ( 'NONE',  ( -22.50000000000000711, 1.387778780781445676E-14, 62.49999999999999289 ) ) ;
#29728 = AXIS2_PLACEMENT_3D ( 'NONE', #9473, #26146, #23801 ) ;
#29729 = DIRECTION ( 'NONE',  ( -0.000000000000000000, -0.000000000000000000, -1.000000000000000000 ) ) ;
#29730 = CARTESIAN_POINT ( 'NONE',  ( 16.52525247487311333, -14.36006998371588317, 1.500000000000000000 ) ) ;
#29731 = CARTESIAN_POINT ( 'NONE',  ( 127.5000000000000000, 0.000000000000000000, 5.035999999999999588 ) ) ;
#29732 = AXIS2_PLACEMENT_3D ( 'NONE', #24712, #8194, #26764 ) ;
#29733 = VERTEX_POINT ( 'NONE', #219 ) ;
#29734 = ORIENTED_EDGE ( 'NONE', *, *, #20259, .T. ) ;
#29735 = VECTOR ( 'NONE', #19237, 1000.000000000000000 ) ;
#29736 = DIRECTION ( 'NONE',  ( 0.000000000000000000, 0.000000000000000000, 1.000000000000000000 ) ) ;
#29737 = LINE ( 'NONE', #17723, #21100 ) ;
#29738 = CARTESIAN_POINT ( 'NONE',  ( 0.000000000000000000, 7.028748154183637631, -16.50000000000000000 ) ) ;
#29739 = AXIS2_PLACEMENT_3D ( 'NONE', #12193, #330, #26394 ) ;
#29740 = ORIENTED_EDGE ( 'NONE', *, *, #12865, .T. ) ;
#29741 =( NAMED_UNIT ( * ) PLANE_ANGLE_UNIT ( ) SI_UNIT ( $, .RADIAN. ) );
#29742 = AXIS2_PLACEMENT_3D ( 'NONE', #17068, #18961, #5374 ) ;
#29743 = CARTESIAN_POINT ( 'NONE',  ( 1.224646799147357201E-15, -10.00000000000003375, -87.50000000000000000 ) ) ;
#29744 = DIRECTION ( 'NONE',  ( -0.000000000000000000, 0.000000000000000000, 1.000000000000000000 ) ) ;
#29745 = ORIENTED_EDGE ( 'NONE', *, *, #11878, .T. ) ;
#29746 = ORIENTED_EDGE ( 'NONE', *, *, #1524, .T. ) ;
#29747 = EDGE_CURVE ( 'NONE', #16446, #16680, #11897, .T. ) ;
#29748 = CARTESIAN_POINT ( 'NONE',  ( 18.35115018089978633, -7.996680568998191241, 20.34789198813115263 ) ) ;
#29749 = DIRECTION ( 'NONE',  ( -0.000000000000000000, -0.000000000000000000, 1.000000000000000000 ) ) ;
#29750 = AXIS2_PLACEMENT_3D ( 'NONE', #22240, #14919, #22081 ) ;
#29751 = CARTESIAN_POINT ( 'NONE',  ( -4.433228896135648966, -43.81350511682552451, -16.50000000000000000 ) ) ;
#29752 = ADVANCED_FACE ( 'NONE', ( #2573 ), #9588, .F. ) ;
#29753 = CARTESIAN_POINT ( 'NONE',  ( -4.704423459274687858, 42.21704346353420334, 28.86412666609725264 ) ) ;
#29754 = EDGE_LOOP ( 'NONE', ( #11955, #99, #4553 ) ) ;
#29755 = CARTESIAN_POINT ( 'NONE',  ( -4.600690885580802636, 16.38836304891080786, 19.08155846658118904 ) ) ;
#29756 = EDGE_CURVE ( 'NONE', #22640, #29034, #682, .T. ) ;
#29757 = EDGE_LOOP ( 'NONE', ( #8880, #28821, #28510, #24517, #21304, #18653, #20650, #21473, #11699, #6343, #22921, #7273, #17430, #7472, #28378, #12070, #15591, #21004, #23978, #1261, #5684, #27278, #25595, #17882, #19578, #8007, #11220, #5809, #14573, #25008, #5726, #22126, #6237, #19108, #26879, #26215, #19229, #22456, #29277, #18643, #1703, #1021, #16433, #10518, #28162, #10281, #29384, #22639, #4899, #21222, #1438, #25374, #18981, #20416, #20749, #24383, #26058, #12907, #12493, #7823, #20207, #3754, #6551, #8316, #14212, #24739, #4751, #8485, #27543, #13690, #13081, #21783, #22052, #20925, #1065, #21072 ) ) ;
#29758 = CIRCLE ( 'NONE', #16620, 15.00000000000000000 ) ;
#29759 = EDGE_CURVE ( 'NONE', #10854, #977, #15884, .T. ) ;
#29760 = CARTESIAN_POINT ( 'NONE',  ( -16.81926493917334042, 2.618766740937769288, 19.60617949693493500 ) ) ;
#29761 = AXIS2_PLACEMENT_3D ( 'NONE', #25908, #27955, #16541 ) ;
#29762 = ORIENTED_EDGE ( 'NONE', *, *, #21763, .F. ) ;
#29763 = CARTESIAN_POINT ( 'NONE',  ( -6.560142022084716196, 18.89374015187015843, 20.15039051365864253 ) ) ;
#29764 = ADVANCED_FACE ( 'NONE', ( #26113 ), #28769, .F. ) ;
#29765 = PLANE ( 'NONE',  #12605 ) ;
#29766 = CARTESIAN_POINT ( 'NONE',  ( 16.64821571380338838, 3.734651121118246042, 5.810767894563978686 ) ) ;
#29767 = CARTESIAN_POINT ( 'NONE',  ( 0.000000000000000000, 0.000000000000000000, -87.50000000000000000 ) ) ;
#29768 = B_SPLINE_CURVE_WITH_KNOTS ( 'NONE', 3,
 ( #451, #12473, #2955, #19473, #22268, #26650, #26493, #23983, #16830, #29304, #21963, #22113, #28843, #29461, #26345, #2630, #14947, #591, #10109, #12152, #7776, #7946, #21651, #9808, #26973, #12767, #24458, #3101, #7477, #17286, #12619, #10259, #17919, #5901, #27583, #27737, #27270, #22427, #23031, #5742, #1680, #20241, #11197, #11047, #10581, #20548, #1071, #25232, #15402, #30069, #24927, #6210, #13551, #3878, #27119, #1384, #17750, #15713, #3563, #8708, #12934, #6053 ),
 .UNSPECIFIED., .F., .F.,
 ( 4, 2, 2, 2, 2, 2, 2, 2, 2, 2, 2, 2, 2, 2, 2, 2, 2, 2, 2, 2, 2, 2, 2, 2, 2, 2, 2, 2, 2, 2, 4 ),
 ( 0.005072925043687738153, 0.01283750835505231488, 0.01671980001073460065, 0.02060209166641688988, 0.02836667497778148916, 0.03224896663346377840, 0.03419011246130493342, 0.03613125828914608151, 0.04389584160051068773, 0.04777813325619299084, 0.05166042491187529395, 0.05942500822323989323, 0.06330729987892219635, 0.06524844570676334443, 0.06718959153460449252, 0.07495417484596912649, 0.07883646650165142267, 0.08077761232949258463, 0.08271875815733373272, 0.09048334146869832506, 0.09242448729653947315, 0.09436563312438060735, 0.09824792478006287577, 0.1021302164357451442, 0.1040713622635862923, 0.1060125080914274404, 0.1137770914027920188, 0.1157182372306331808, 0.1176593830584743428, 0.1215416747141566389, 0.1293062580255212313 ),
 .UNSPECIFIED. ) ;
#29769 = CIRCLE ( 'NONE', #28274, 0.7500000000000006661 ) ;
#29770 = EDGE_CURVE ( 'NONE', #12261, #28625, #19782, .T. ) ;
#29771 = CYLINDRICAL_SURFACE ( 'NONE', #11775, 27.70876437800068359 ) ;
#29772 = EDGE_CURVE ( 'NONE', #8229, #30243, #7720, .T. ) ;
#29773 = CARTESIAN_POINT ( 'NONE',  ( -17.06238204535245018, 0.6919203014575876498, 19.02573955821369012 ) ) ;
#29774 = CARTESIAN_POINT ( 'NONE',  ( -17.03551135121415783, 1.010186107319478888, 18.56793045041961321 ) ) ;
#29775 = LINE ( 'NONE', #27592, #23305 ) ;
#29776 = VERTEX_POINT ( 'NONE', #14574 ) ;
#29777 = VECTOR ( 'NONE', #12363, 1000.000000000000000 ) ;
#29778 = CARTESIAN_POINT ( 'NONE',  ( 39.87808514434166085, -7.028748154387577607, -14.83333104074398356 ) ) ;
#29779 = AXIS2_PLACEMENT_3D ( 'NONE', #10309, #7821, #22463 ) ;
#29780 = CARTESIAN_POINT ( 'NONE',  ( 11.90564931213029531, -16.09225693709295513, 19.03762469184452755 ) ) ;
#29781 = CARTESIAN_POINT ( 'NONE',  ( 31.18890335284658022, 19.89223002944920538, 34.80090346875810070 ) ) ;
#29782 = CIRCLE ( 'NONE', #24778, 12.50000000000000000 ) ;
#29783 = ORIENTED_EDGE ( 'NONE', *, *, #11100, .T. ) ;
#29784 = ORIENTED_EDGE ( 'NONE', *, *, #2360, .F. ) ;
#29785 = CARTESIAN_POINT ( 'NONE',  ( -4.163336342344337027E-14, -1.387778780781445676E-14, 1.500000000000000000 ) ) ;
#29786 = CARTESIAN_POINT ( 'NONE',  ( 0.000000000000000000, 13.00000000000001421, 24.50000000000000000 ) ) ;
#29787 = CARTESIAN_POINT ( 'NONE',  ( -4.619434794156391355, 16.38343285047924880, 6.974106381145714018 ) ) ;
#29788 = EDGE_LOOP ( 'NONE', ( #20875, #15069, #26869 ) ) ;
#29789 = DIRECTION ( 'NONE',  ( 1.000000000000000000, 0.000000000000000000, 0.000000000000000000 ) ) ;
#29790 = CIRCLE ( 'NONE', #21802, 20.00000000000000000 ) ;
#29791 = LINE ( 'NONE', #8432, #17653 ) ;
#29792 = VECTOR ( 'NONE', #4586, 1000.000000000000114 ) ;
#29793 = EDGE_CURVE ( 'NONE', #2233, #16863, #21263, .T. ) ;
#29794 = CARTESIAN_POINT ( 'NONE',  ( -1.000000000000008438, 13.00000000000001421, 24.50000000000000000 ) ) ;
#29795 = ORIENTED_EDGE ( 'NONE', *, *, #23266, .F. ) ;
#29796 = ADVANCED_FACE ( 'NONE', ( #7239 ), #2726, .F. ) ;
#29797 = ADVANCED_FACE ( 'NONE', ( #26592 ), #17419, .T. ) ;
#29798 = DIRECTION ( 'NONE',  ( -0.9329908884337538844, 0.3598999890241658117, 0.000000000000000000 ) ) ;
#29799 = CARTESIAN_POINT ( 'NONE',  ( 12.12755608862869039, 11.99246096336393030, 5.704143890883081269 ) ) ;
#29800 = CARTESIAN_POINT ( 'NONE',  ( 19.81227057857146434, 2.861376016183142745, 7.595116371587256054 ) ) ;
#29801 = EDGE_LOOP ( 'NONE', ( #20827, #10602, #16899, #16316 ) ) ;
#29802 = CARTESIAN_POINT ( 'NONE',  ( 12.71123406193363437, 11.33589958720537005, 5.796888747622817029 ) ) ;
#29803 = ORIENTED_EDGE ( 'NONE', *, *, #20958, .T. ) ;
#29804 = AXIS2_PLACEMENT_3D ( 'NONE', #9516, #19034, #28548 ) ;
#29805 = CARTESIAN_POINT ( 'NONE',  ( 3.395021109945009385, -30.50000000000000711, 24.50000000000000000 ) ) ;
#29806 = EDGE_CURVE ( 'NONE', #8417, #3543, #18310, .T. ) ;
#29807 = CIRCLE ( 'NONE', #10360, 20.00000000000000000 ) ;
#29808 = DIRECTION ( 'NONE',  ( 0.000000000000000000, 0.000000000000000000, 1.000000000000000000 ) ) ;
#29809 = ORIENTED_EDGE ( 'NONE', *, *, #22521, .T. ) ;
#29810 = ORIENTED_EDGE ( 'NONE', *, *, #21390, .T. ) ;
#29811 = EDGE_CURVE ( 'NONE', #19771, #12217, #11818, .T. ) ;
#29812 = EDGE_CURVE ( 'NONE', #12979, #23779, #6556, .T. ) ;
#29813 = CARTESIAN_POINT ( 'NONE',  ( 3.269395338272006235, 16.75466097144276745, 6.041646659195333058 ) ) ;
#29814 = CARTESIAN_POINT ( 'NONE',  ( 33.36692087966583387, 9.471517865689168758, 40.31490688621818208 ) ) ;
#29815 = LINE ( 'NONE', #1714, #29269 ) ;
#29816 = VECTOR ( 'NONE', #20505, 1000.000000000000000 ) ;
#29817 = CARTESIAN_POINT ( 'NONE',  ( -28.55068628633583216, -24.19494186940697134, 34.80090346875804386 ) ) ;
#29818 = DIRECTION ( 'NONE',  ( -0.000000000000000000, -0.000000000000000000, 1.000000000000000000 ) ) ;
#29819 = CARTESIAN_POINT ( 'NONE',  ( 16.87938398529692918, 2.193321724558643382, 19.45164628100866722 ) ) ;
#29820 = ORIENTED_EDGE ( 'NONE', *, *, #23991, .F. ) ;
#29821 = DIRECTION ( 'NONE',  ( -0.000000000000000000, -1.000000000000000000, -0.000000000000000000 ) ) ;
#29822 = CARTESIAN_POINT ( 'NONE',  ( 15.51722275458702960, -7.010743380608710495, 5.940635272151477686 ) ) ;
#29823 = CARTESIAN_POINT ( 'NONE',  ( -15.75339717617904611, 12.35099711776840792, 20.13759033520874908 ) ) ;
#29824 = CARTESIAN_POINT ( 'NONE',  ( -28.37932450449293853, 10.51822134874671022, -1.500000000000000000 ) ) ;
#29825 = ORIENTED_EDGE ( 'NONE', *, *, #6743, .T. ) ;
#29826 = ORIENTED_EDGE ( 'NONE', *, *, #29404, .T. ) ;
#29827 = DIRECTION ( 'NONE',  ( 0.000000000000000000, 0.000000000000000000, 1.000000000000000000 ) ) ;
#29828 = CARTESIAN_POINT ( 'NONE',  ( 1.224038712338732404, -19.98030457043140018, 6.131018562779544823 ) ) ;
#29829 = ADVANCED_FACE ( 'NONE', ( #30058 ), #28019, .F. ) ;
#29830 = B_SPLINE_SURFACE_WITH_KNOTS ( 'NONE', 3, 1, ( 
 ( #7975, #17478 ),
 ( #5772, #27458 ),
 ( #8443, #10291 ),
 ( #29800, #7802 ),
 ( #21990, #20120 ),
 ( #943, #1254 ),
 ( #15266, #24797 ),
 ( #3436, #12957 ),
 ( #26847, #27301 ),
 ( #5932, #29166 ),
 ( #12651, #8272 ),
 ( #10455, #15121 ),
 ( #22450, #15588 ),
 ( #17629, #24638 ),
 ( #29333, #1098 ),
 ( #22299, #22143 ),
 ( #10609, #27000 ),
 ( #19969, #3271 ),
 ( #12800, #3128 ),
 ( #2979, #15429 ),
 ( #17786, #5470 ),
 ( #24951, #29488 ),
 ( #13112, #8123 ),
 ( #27146, #22603 ),
 ( #10761, #14971 ),
 ( #20272, #17948 ),
 ( #6078, #12496 ),
 ( #621, #10138 ),
 ( #19644, #17315 ),
 ( #24484, #20878 ),
 ( #30245, #6234 ) ),
 .UNSPECIFIED., .F., .F., .F.,
 ( 4, 3, 3, 3, 3, 3, 3, 3, 3, 3, 4 ),
 ( 2, 2 ),
 ( 0.000000000000000000, 0.05425176834609633791, 0.1085332949128352958, 0.1623767749169382768, 0.2157504826133063158, 0.2688657508888171455, 0.3218907763505476360, 0.3749548578363336993, 0.4282048033836242107, 0.4818374082110501444, 0.4999999999131654604 ),
 ( 0.000000000000000000, 1.000000000000000000 ),
 .UNSPECIFIED. ) ;
#29831 = CARTESIAN_POINT ( 'NONE',  ( 12.44336852755150424, 11.64466880993055398, 5.651492010659111109 ) ) ;
#29832 = DIRECTION ( 'NONE',  ( -0.000000000000000000, -0.000000000000000000, 1.000000000000000000 ) ) ;
#29833 = VECTOR ( 'NONE', #27997, 1000.000000000000000 ) ;
#29834 = EDGE_CURVE ( 'NONE', #7465, #25448, #16808, .T. ) ;
#29835 = CARTESIAN_POINT ( 'NONE',  ( 0.000000000000000000, 0.000000000000000000, -1.500000000000000000 ) ) ;
#29836 = VECTOR ( 'NONE', #26011, 1000.000000000000000 ) ;
#29837 = FACE_OUTER_BOUND ( 'NONE', #24793, .T. ) ;
#29838 = EDGE_CURVE ( 'NONE', #20491, #28528, #24917, .T. ) ;
#29839 = CARTESIAN_POINT ( 'NONE',  ( 16.85625572096651226, 2.395390699250522726, 7.267659094423557953 ) ) ;
#29840 = ORIENTED_EDGE ( 'NONE', *, *, #6473, .T. ) ;
#29841 = DIRECTION ( 'NONE',  ( 1.000000000000000000, 0.000000000000000000, 0.000000000000000000 ) ) ;
#29842 = AXIS2_PLACEMENT_3D ( 'NONE', #17794, #19974, #29808 ) ;
#29843 = CARTESIAN_POINT ( 'NONE',  ( -33.56615453960540663, 10.45399542313511354, 39.84392849731690234 ) ) ;
#29844 = DIRECTION ( 'NONE',  ( -1.000000000000000000, 0.000000000000000000, 0.000000000000000000 ) ) ;
#29845 = ORIENTED_EDGE ( 'NONE', *, *, #9043, .F. ) ;
#29846 = ORIENTED_EDGE ( 'NONE', *, *, #1036, .F. ) ;
#29847 = CARTESIAN_POINT ( 'NONE',  ( 0.000000000000000000, 0.000000000000000000, 1.500000000000000000 ) ) ;
#29848 = CARTESIAN_POINT ( 'NONE',  ( -19.92877566111874899, 1.688993080932616353, 18.73377938172347612 ) ) ;
#29849 = ORIENTED_EDGE ( 'NONE', *, *, #8671, .T. ) ;
#29850 = DIRECTION ( 'NONE',  ( -0.000000000000000000, -0.000000000000000000, 1.000000000000000000 ) ) ;
#29851 = CARTESIAN_POINT ( 'NONE',  ( 13.47544704454163522, 48.15148052472740403, -48.33895490383400073 ) ) ;
#29852 = DIRECTION ( 'NONE',  ( -0.4154150130018840481, 0.9096319953545194403, 0.000000000000000000 ) ) ;
#29853 = CARTESIAN_POINT ( 'NONE',  ( -37.92875555959543021, 9.893234292455838741, 12.22166928970610478 ) ) ;
#29854 = DIRECTION ( 'NONE',  ( 1.000000000000000000, 0.000000000000000000, 0.000000000000000000 ) ) ;
#29855 = VECTOR ( 'NONE', #29659, 1000.000000000000000 ) ;
#29856 = AXIS2_PLACEMENT_3D ( 'NONE', #9910, #24247, #12416 ) ;
#29857 = CYLINDRICAL_SURFACE ( 'NONE', #11390, 4.999999999999997335 ) ;
#29858 = CARTESIAN_POINT ( 'NONE',  ( -40.00000000000000000, 63.74772708486752038, 62.49999999999999289 ) ) ;
#29859 = LINE ( 'NONE', #8499, #26178 ) ;
#29860 = DIRECTION ( 'NONE',  ( 0.000000000000000000, 0.000000000000000000, 1.000000000000000000 ) ) ;
#29861 = ORIENTED_EDGE ( 'NONE', *, *, #30016, .T. ) ;
#29862 = CIRCLE ( 'NONE', #3469, 0.7441270634457181066 ) ;
#29863 = CARTESIAN_POINT ( 'NONE',  ( -9.213835811784830909, -14.31736145455815290, 18.71435384576123440 ) ) ;
#29864 = CARTESIAN_POINT ( 'NONE',  ( -26.36764545593177544, 31.31467416275353344, -1.500000000000000000 ) ) ;
#29865 = CARTESIAN_POINT ( 'NONE',  ( -24.03448224033878944, -8.660042335149837456, 49.47829057475703252 ) ) ;
#29866 = CARTESIAN_POINT ( 'NONE',  ( 11.18191171624325797, -16.60365183919259380, 5.652605728828375753 ) ) ;
#29867 = EDGE_CURVE ( 'NONE', #21841, #27491, #22278, .T. ) ;
#29868 = CARTESIAN_POINT ( 'NONE',  ( 10.64374042650142904, 42.96126232887663576, -19.50000000000000355 ) ) ;
#29869 = VECTOR ( 'NONE', #29676, 1000.000000000000000 ) ;
#29870 = FACE_OUTER_BOUND ( 'NONE', #25690, .T. ) ;
#29871 = EDGE_LOOP ( 'NONE', ( #29952, #29623, #601, #28947 ) ) ;
#29872 = ORIENTED_EDGE ( 'NONE', *, *, #12436, .T. ) ;
#29873 = CARTESIAN_POINT ( 'NONE',  ( 17.26937953831880534, -14.36006998371588317, 1.500000000000000000 ) ) ;
#29874 = CARTESIAN_POINT ( 'NONE',  ( -39.00000000000000000, 5.563236990218665134, -1.500000000000000000 ) ) ;
#29875 = CARTESIAN_POINT ( 'NONE',  ( -15.00589365688690435, 13.24944937571967429, 5.796888747622817029 ) ) ;
#29876 = LINE ( 'NONE', #8516, #9591 ) ;
#29877 = VERTEX_POINT ( 'NONE', #15552 ) ;
#29878 = CARTESIAN_POINT ( 'NONE',  ( -4.163336342344337027E-14, -1.387778780781445676E-14, 1.500000000000000000 ) ) ;
#29879 = CARTESIAN_POINT ( 'NONE',  ( 40.89187623478217404, 5.790488632116406187, -19.50000000000000355 ) ) ;
#29880 = CARTESIAN_POINT ( 'NONE',  ( -10.62006778255435435, -16.96839658127461803, 5.657991946698900598 ) ) ;
#29881 = ORIENTED_EDGE ( 'NONE', *, *, #10143, .F. ) ;
#29882 = CIRCLE ( 'NONE', #28891, 9.084132297865673777 ) ;
#29883 = DIRECTION ( 'NONE',  ( 0.000000000000000000, 0.000000000000000000, -1.000000000000000000 ) ) ;
#29884 = CARTESIAN_POINT ( 'NONE',  ( -22.32897562208770026, -34.85472879511701194, 34.50814406507193155 ) ) ;
#29885 = VERTEX_POINT ( 'NONE', #20228 ) ;
#29886 = CARTESIAN_POINT ( 'NONE',  ( 0.000000000000000000, 0.000000000000000000, 1.500000000000001332 ) ) ;
#29887 = CARTESIAN_POINT ( 'NONE',  ( -8.416592248870403026, -14.82768166143396726, 5.661398277488802755 ) ) ;
#29888 = VECTOR ( 'NONE', #13372, 1000.000000000000000 ) ;
#29889 = DIRECTION ( 'NONE',  ( -0.000000000000000000, -0.000000000000000000, -1.000000000000000000 ) ) ;
#29890 = ORIENTED_EDGE ( 'NONE', *, *, #30, .F. ) ;
#29891 = DIRECTION ( 'NONE',  ( 0.000000000000000000, 0.000000000000000000, 1.000000000000000000 ) ) ;
#29892 = CARTESIAN_POINT ( 'NONE',  ( 31.79204601741444236, 14.90874471747208219, 35.64345580000760805 ) ) ;
#29893 = CARTESIAN_POINT ( 'NONE',  ( -50.00000000000000000, 50.00000000000000000, 52.07879600563550326 ) ) ;
#29894 = DIRECTION ( 'NONE',  ( 0.000000000000000000, -0.000000000000000000, -1.000000000000000000 ) ) ;
#29895 = CARTESIAN_POINT ( 'NONE',  ( -7.500000000000000000, 0.000000000000000000, -1.500000000000001332 ) ) ;
#29896 = CARTESIAN_POINT ( 'NONE',  ( 35.00000000000000000, 70.00000000000000000, 12.49999999999999112 ) ) ;
#29897 = CARTESIAN_POINT ( 'NONE',  ( -8.478038329015333829, 15.04174200911163517, 1.500000000000000000 ) ) ;
#29898 = CYLINDRICAL_SURFACE ( 'NONE', #14409, 0.7500000000000004441 ) ;
#29899 = CARTESIAN_POINT ( 'NONE',  ( 19.83281414115337782, 2.582324728781452361, 7.454139397117725885 ) ) ;
#29900 = CARTESIAN_POINT ( 'NONE',  ( 35.99999999999969447, -0.8865895960784948571, 34.75735931288063085 ) ) ;
#29901 = CIRCLE ( 'NONE', #24923, 34.99999999999933920 ) ;
#29902 = DIRECTION ( 'NONE',  ( -1.000000000000000000, -0.000000000000000000, -0.000000000000000000 ) ) ;
#29903 = EDGE_CURVE ( 'NONE', #24108, #20004, #11796, .T. ) ;
#29904 = ORIENTED_EDGE ( 'NONE', *, *, #26145, .T. ) ;
#29905 = ORIENTED_EDGE ( 'NONE', *, *, #21348, .T. ) ;
#29906 = CARTESIAN_POINT ( 'NONE',  ( 4.390207617113956573, -7.856594496258208160, 21.50000000000000000 ) ) ;
#29907 = DIRECTION ( 'NONE',  ( 0.000000000000000000, 0.000000000000000000, -1.000000000000000000 ) ) ;
#29908 = CARTESIAN_POINT ( 'NONE',  ( -2.462452140056639038, 49.94168384355573664, -69.80474203353597318 ) ) ;
#29909 = ORIENTED_EDGE ( 'NONE', *, *, #24663, .T. ) ;
#29910 = FACE_OUTER_BOUND ( 'NONE', #4091, .T. ) ;
#29911 = CARTESIAN_POINT ( 'NONE',  ( 9.644751206715060476, -14.04611738690534573, 18.37259980046033903 ) ) ;
#29912 = EDGE_LOOP ( 'NONE', ( #15342, #14314, #2902, #14937 ) ) ;
#29913 = ORIENTED_EDGE ( 'NONE', *, *, #7744, .T. ) ;
#29914 = CARTESIAN_POINT ( 'NONE',  ( -11.25470158702820811, -16.53282404628956925, 19.85261563089511583 ) ) ;
#29915 = CARTESIAN_POINT ( 'NONE',  ( -31.10273980501929003, -15.38400267427140022, 36.05808397467838233 ) ) ;
#29916 = CARTESIAN_POINT ( 'NONE',  ( -8.611567383417474630, -14.70762963579928417, 18.34969686940295830 ) ) ;
#29917 = DIRECTION ( 'NONE',  ( 0.000000000000000000, 0.000000000000000000, 1.000000000000000000 ) ) ;
#29918 = EDGE_LOOP ( 'NONE', ( #7528, #15193 ) ) ;
#29919 = FACE_OUTER_BOUND ( 'NONE', #22248, .T. ) ;
#29920 = ORIENTED_EDGE ( 'NONE', *, *, #16782, .T. ) ;
#29921 = CARTESIAN_POINT ( 'NONE',  ( 52.16608720827707657, 36.86186943028246787, 12.49999999999999112 ) ) ;
#29922 = CIRCLE ( 'NONE', #16460, 9.000000000000000000 ) ;
#29923 = CARTESIAN_POINT ( 'NONE',  ( -16.83567995170645304, 2.524450606588025448, 19.85270094495841775 ) ) ;
#29924 = EDGE_LOOP ( 'NONE', ( #29173, #29586, #13617, #2148 ) ) ;
#29925 = DIRECTION ( 'NONE',  ( -0.8412535328311884220, -0.5406408174555862312, 0.000000000000000000 ) ) ;
#29926 = DIRECTION ( 'NONE',  ( 0.000000000000000000, 0.000000000000000000, -1.000000000000000000 ) ) ;
#29927 = DIRECTION ( 'NONE',  ( -1.000000000000000000, 0.000000000000000000, 0.000000000000000000 ) ) ;
#29928 = CARTESIAN_POINT ( 'NONE',  ( -12.91351154505913179, 11.09846585523631823, 18.63641924841378028 ) ) ;
#29929 = CARTESIAN_POINT ( 'NONE',  ( -9.846411740200890605, -17.42855948811279276, 19.97651184436794125 ) ) ;
#29930 = EDGE_CURVE ( 'NONE', #11382, #14759, #12837, .T. ) ;
#29931 = CARTESIAN_POINT ( 'NONE',  ( -17.06630883447662583, 0.6398751886020307422, 19.28454053338348473 ) ) ;
#29932 = CARTESIAN_POINT ( 'NONE',  ( -16.98411243466783560, 1.496360031252971456, 18.35718225375110180 ) ) ;
#29933 = DIRECTION ( 'NONE',  ( -1.000000000000000000, 0.000000000000000000, 0.000000000000000000 ) ) ;
#29934 = VERTEX_POINT ( 'NONE', #28492 ) ;
#29935 = DIRECTION ( 'NONE',  ( 1.000000000000000000, 0.000000000000000000, 0.000000000000000000 ) ) ;
#29936 = CARTESIAN_POINT ( 'NONE',  ( 10.16054539467770113, 13.96046037420044961, -0.6213203435596476032 ) ) ;
#29937 = ORIENTED_EDGE ( 'NONE', *, *, #15246, .T. ) ;
#29938 = ORIENTED_EDGE ( 'NONE', *, *, #7514, .T. ) ;
#29939 = CARTESIAN_POINT ( 'NONE',  ( -2.185336383880142730, 8.817355867515834333, 21.50000000000000000 ) ) ;
#29940 = ADVANCED_FACE ( 'NONE', ( #16631 ), #9758, .F. ) ;
#29941 = AXIS2_PLACEMENT_3D ( 'NONE', #18338, #11006, #1791 ) ;
#29942 = CARTESIAN_POINT ( 'NONE',  ( -5.557658336892894901, 19.23087281213772570, 5.749228751562096562 ) ) ;
#29943 = ORIENTED_EDGE ( 'NONE', *, *, #26687, .F. ) ;
#29944 = CARTESIAN_POINT ( 'NONE',  ( 5.291489565152560637, 19.28730510418394317, 5.652196082369965069 ) ) ;
#29945 = VECTOR ( 'NONE', #18841, 1000.000000000000000 ) ;
#29946 = CARTESIAN_POINT ( 'NONE',  ( -12.97413174825823390, 11.03100730454233336, 7.453286057244485008 ) ) ;
#29947 = CARTESIAN_POINT ( 'NONE',  ( -27.03074382657074537, 6.449748410230984774, 47.21042702067971675 ) ) ;
#29948 = EDGE_LOOP ( 'NONE', ( #19890, #16657 ) ) ;
#29949 = DIRECTION ( 'NONE',  ( 0.000000000000000000, 0.000000000000000000, 1.000000000000000000 ) ) ;
#29950 = CARTESIAN_POINT ( 'NONE',  ( 11.91933518721470264, 12.21304923692660971, 5.872146474157316831 ) ) ;
#29951 = FACE_BOUND ( 'NONE', #7222, .T. ) ;
#29952 = ORIENTED_EDGE ( 'NONE', *, *, #10269, .F. ) ;
#29953 = EDGE_CURVE ( 'NONE', #15672, #29287, #23482, .T. ) ;
#29954 = CARTESIAN_POINT ( 'NONE',  ( 0.1262659238204208167, 8.999114229549594057, -1.500000000000000888 ) ) ;
#29955 = ORIENTED_EDGE ( 'NONE', *, *, #27313, .F. ) ;
#29956 = CARTESIAN_POINT ( 'NONE',  ( -3.469446951953614189E-15, -30.50000000000000711, 1.500000000000001332 ) ) ;
#29957 = ORIENTED_EDGE ( 'NONE', *, *, #13184, .F. ) ;
#29958 = ORIENTED_EDGE ( 'NONE', *, *, #12043, .T. ) ;
#29959 = DIRECTION ( 'NONE',  ( 0.000000000000000000, 0.000000000000000000, 1.000000000000000000 ) ) ;
#29960 = ORIENTED_EDGE ( 'NONE', *, *, #8434, .F. ) ;
#29961 = CIRCLE ( 'NONE', #8055, 0.7500000000000006661 ) ;
#29962 = CARTESIAN_POINT ( 'NONE',  ( 0.000000000000000000, 0.000000000000000000, 1.500000000000000000 ) ) ;
#29963 = CARTESIAN_POINT ( 'NONE',  ( 19.81227057857146434, 2.861376016183142745, 20.29090034784956131 ) ) ;
#29964 = EDGE_CURVE ( 'NONE', #15180, #4126, #23300, .T. ) ;
#29965 = ORIENTED_EDGE ( 'NONE', *, *, #24280, .T. ) ;
#29966 = ADVANCED_FACE ( 'NONE', ( #2121 ), #21291, .T. ) ;
#29967 = CARTESIAN_POINT ( 'NONE',  ( 0.000000000000000000, -8.043452525345523162E-15, -16.50000000000000000 ) ) ;
#29968 = CARTESIAN_POINT ( 'NONE',  ( 0.3567147238643519902, -19.99681861211371370, 18.34798005863226678 ) ) ;
#29969 = CARTESIAN_POINT ( 'NONE',  ( -15.45532977000708108, 12.72198496171735371, 5.661398277488802755 ) ) ;
#29970 = CARTESIAN_POINT ( 'NONE',  ( 4.606472074292930152, 19.48056636435423528, 20.06253562465620632 ) ) ;
#29971 = ORIENTED_EDGE ( 'NONE', *, *, #21784, .F. ) ;
#29972 = VERTEX_POINT ( 'NONE', #4621 ) ;
#29973 = DIRECTION ( 'NONE',  ( -0.000000000000000000, -0.000000000000000000, -1.000000000000000000 ) ) ;
#29974 = DIRECTION ( 'NONE',  ( -0.000000000000000000, -0.000000000000000000, -1.000000000000000000 ) ) ;
#29975 = EDGE_CURVE ( 'NONE', #20802, #16462, #5880, .T. ) ;
#29976 = AXIS2_PLACEMENT_3D ( 'NONE', #21345, #16371, #23384 ) ;
#29977 = CARTESIAN_POINT ( 'NONE',  ( -5.010690217951877301, 19.38064900392119583, 19.22654678686458141 ) ) ;
#29978 = DIRECTION ( 'NONE',  ( 1.000000000000000000, 0.000000000000000000, 0.000000000000000000 ) ) ;
#29979 = EDGE_CURVE ( 'NONE', #10914, #19423, #28341, .T. ) ;
#29980 = FACE_BOUND ( 'NONE', #5232, .T. ) ;
#29981 = DIRECTION ( 'NONE',  ( 1.000000000000000000, 0.000000000000000000, 0.000000000000000000 ) ) ;
#29982 = EDGE_CURVE ( 'NONE', #16098, #4045, #20804, .T. ) ;
#29983 = EDGE_LOOP ( 'NONE', ( #24990, #13471, #21124, #12026, #15, #29149 ) ) ;
#29984 = CIRCLE ( 'NONE', #20507, 4.999999999999997335 ) ;
#29985 = CARTESIAN_POINT ( 'NONE',  ( -32.68377466358848693, -8.668986135640256663, 36.94359686629218942 ) ) ;
#29986 = DIRECTION ( 'NONE',  ( 1.000000000000000000, 0.000000000000000000, 0.000000000000000000 ) ) ;
#29987 = CARTESIAN_POINT ( 'NONE',  ( -1.000000000000008438, 13.00000000000001421, 1.500000000000001332 ) ) ;
#29988 = ORIENTED_EDGE ( 'NONE', *, *, #4449, .T. ) ;
#29989 = EDGE_CURVE ( 'NONE', #11886, #11902, #26135, .T. ) ;
#29990 = ORIENTED_EDGE ( 'NONE', *, *, #13036, .T. ) ;
#29991 = PLANE ( 'NONE',  #21733 ) ;
#29992 = CARTESIAN_POINT ( 'NONE',  ( 13.88429941593329531, 16.69721919943964039, 1.500000000000000000 ) ) ;
#29993 = EDGE_LOOP ( 'NONE', ( #13657, #13677, #10727, #848 ) ) ;
#29994 = CARTESIAN_POINT ( 'NONE',  ( -9.436481611552759219, -0.9307681286968215728, 13.00000000000000178 ) ) ;
#29995 = LINE ( 'NONE', #13313, #22732 ) ;
#29996 = VECTOR ( 'NONE', #28736, 1000.000000000000000 ) ;
#29997 = CARTESIAN_POINT ( 'NONE',  ( 1.000000000000008438, 13.00000000000001421, 24.50000000000000000 ) ) ;
#29998 = CARTESIAN_POINT ( 'NONE',  ( 6.900000000000000355, 0.000000000000000000, 0.000000000000000000 ) ) ;
#29999 = FACE_OUTER_BOUND ( 'NONE', #7544, .T. ) ;
#30000 = CARTESIAN_POINT ( 'NONE',  ( 0.8870900849372825858, -19.99803318816114484, 7.500147780736496017 ) ) ;
#30001 = CARTESIAN_POINT ( 'NONE',  ( -16.81371235015666699, 2.650171115930315846, 6.714907520933426355 ) ) ;
#30002 = EDGE_CURVE ( 'NONE', #2231, #15872, #2442, .T. ) ;
#30003 = ORIENTED_EDGE ( 'NONE', *, *, #11651, .T. ) ;
#30004 = ADVANCED_FACE ( 'NONE', ( #97 ), #28640, .F. ) ;
#30005 = CARTESIAN_POINT ( 'NONE',  ( 35.76344986165623396, 22.29344514668041199, -19.50000000000000355 ) ) ;
#30006 = CARTESIAN_POINT ( 'NONE',  ( 0.000000000000000000, 1.699320956058915452E-16, -1.500000000000001776 ) ) ;
#30007 = EDGE_CURVE ( 'NONE', #14545, #29153, #18106, .T. ) ;
#30008 = CARTESIAN_POINT ( 'NONE',  ( -5.686690470302443678, 16.07334902597871817, 7.643931100913408550 ) ) ;
#30009 = CARTESIAN_POINT ( 'NONE',  ( 9.984725267469517718, -13.82013960671583241, 7.643931100913408550 ) ) ;
#30010 = CARTESIAN_POINT ( 'NONE',  ( -5.374868878256215510, -44.10336124695545124, -19.50000000000000355 ) ) ;
#30011 = CARTESIAN_POINT ( 'NONE',  ( -26.36764545593177544, 31.31467416275353344, 1.500000000000000000 ) ) ;
#30012 = ORIENTED_EDGE ( 'NONE', *, *, #6123, .T. ) ;
#30013 = CARTESIAN_POINT ( 'NONE',  ( 49.99999999999998579, 87.00000000000001421, 52.49999999999999289 ) ) ;
#30014 = CARTESIAN_POINT ( 'NONE',  ( 23.96732207938043402, -33.98584080152387088, -1.500000000000000000 ) ) ;
#30015 = CARTESIAN_POINT ( 'NONE',  ( 34.55425493108410251, -14.62473873825366688, 37.50000000006821210 ) ) ;
#30016 = EDGE_CURVE ( 'NONE', #22720, #29776, #12889, .T. ) ;
#30018 = VECTOR ( 'NONE', #12096, 1000.000000000000000 ) ;
#30017 = CARTESIAN_POINT ( 'NONE',  ( 9.301547456646380496, 8.591538895647095941, 1.500000000000000000 ) ) ;
#30019 = VERTEX_POINT ( 'NONE', #17086 ) ;
#30020 = CARTESIAN_POINT ( 'NONE',  ( 0.000000000000000000, 1.699320956058915452E-16, -1.500000000000001776 ) ) ;
#30021 = CARTESIAN_POINT ( 'NONE',  ( 0.000000000000000000, 44.39187623478217404, -19.50000000000000355 ) ) ;
#30022 = CARTESIAN_POINT ( 'NONE',  ( -11.24862133554823274, -16.55851774953666222, 7.176035686813569292 ) ) ;
#30023 = ORIENTED_EDGE ( 'NONE', *, *, #27873, .T. ) ;
#30024 = DIRECTION ( 'NONE',  ( 0.000000000000000000, 0.000000000000000000, 1.000000000000000000 ) ) ;
#30025 = CARTESIAN_POINT ( 'NONE',  ( 19.55517958221000185, 4.194633687229719854, 19.21940439362674624 ) ) ;
#30026 = ORIENTED_EDGE ( 'NONE', *, *, #7245, .T. ) ;
#30027 = CARTESIAN_POINT ( 'NONE',  ( -32.19782014694307293, -14.25394737442115733, 39.78814634291943264 ) ) ;
#30028 = ADVANCED_FACE ( 'NONE', ( #26614 ), #29256, .F. ) ;
#30029 = EDGE_CURVE ( 'NONE', #12655, #4949, #12342, .T. ) ;
#30030 = CARTESIAN_POINT ( 'NONE',  ( 31.22647667302025454, -15.32805873036034860, 40.21452297286836597 ) ) ;
#30031 = VERTEX_POINT ( 'NONE', #24258 ) ;
#30032 = CARTESIAN_POINT ( 'NONE',  ( 2.703030265324084080, -12.75514121382991384, 24.50000000000000000 ) ) ;
#30033 = AXIS2_PLACEMENT_3D ( 'NONE', #3029, #22500, #13009 ) ;
#30034 = CARTESIAN_POINT ( 'NONE',  ( 16.70031948179167003, 3.459335817989516393, 5.653604225791663218 ) ) ;
#30035 = CARTESIAN_POINT ( 'NONE',  ( -32.19782014694307293, -14.25394737442115733, 39.78814634291943264 ) ) ;
#30036 = CARTESIAN_POINT ( 'NONE',  ( -45.91542376395022984, 69.58700628869918603, 14.40979685689198675 ) ) ;
#30037 = CARTESIAN_POINT ( 'NONE',  ( -17.05632420042165265, 0.7692048344871257326, 6.147510495896842286 ) ) ;
#30038 = CARTESIAN_POINT ( 'NONE',  ( 35.00000000000000000, 70.00000000000000000, 12.49999999999999112 ) ) ;
#30039 = CARTESIAN_POINT ( 'NONE',  ( -2.959227181723746547, 8.499586724479465616, 21.50000000000000000 ) ) ;
#30040 = DIRECTION ( 'NONE',  ( -0.000000000000000000, 1.132880637372608986E-16, -1.000000000000000000 ) ) ;
#30041 = CARTESIAN_POINT ( 'NONE',  ( 19.87632233081031075, 2.221350112303686952, 6.386539667786102825 ) ) ;
#30042 = CARTESIAN_POINT ( 'NONE',  ( -52.16608720827707657, -51.86186943028246787, 12.49999999999998401 ) ) ;
#30043 = CARTESIAN_POINT ( 'NONE',  ( 8.413215745754998309, -3.196529495465417980, 21.50000000000000000 ) ) ;
#30044 = ORIENTED_EDGE ( 'NONE', *, *, #8031, .F. ) ;
#30045 = ORIENTED_EDGE ( 'NONE', *, *, #23145, .T. ) ;
#30046 = CARTESIAN_POINT ( 'NONE',  ( 0.000000000000000000, 0.000000000000000000, 1.500000000000001332 ) ) ;
#30047 = CARTESIAN_POINT ( 'NONE',  ( 35.76344986163714168, -22.29344514668044752, -19.50000000000000355 ) ) ;
#30048 = DIRECTION ( 'NONE',  ( 0.000000000000000000, 0.000000000000000000, 1.000000000000000000 ) ) ;
#30049 = ORIENTED_EDGE ( 'NONE', *, *, #7497, .T. ) ;
#30050 = CARTESIAN_POINT ( 'NONE',  ( -10.47960520055065636, -7.757439966934454034, 1.500000000000001332 ) ) ;
#30051 = CARTESIAN_POINT ( 'NONE',  ( 11.82521593960875173, 5.400395169024529984, 24.50000000000000000 ) ) ;
#30052 = AXIS2_PLACEMENT_3D ( 'NONE', #10749, #15578, #3739 ) ;
#30053 = VERTEX_POINT ( 'NONE', #547 ) ;
#30054 = ORIENTED_EDGE ( 'NONE', *, *, #11645, .F. ) ;
#30055 = AXIS2_PLACEMENT_3D ( 'NONE', #17772, #27138, #20423 ) ;
#30056 = CARTESIAN_POINT ( 'NONE',  ( -16.81358047026921199, 2.650995224496061731, 6.755862304746362845 ) ) ;
#30057 = DIRECTION ( 'NONE',  ( 0.000000000000000000, 0.000000000000000000, 1.000000000000000000 ) ) ;
#30058 = FACE_OUTER_BOUND ( 'NONE', #21709, .T. ) ;
#30059 = DIRECTION ( 'NONE',  ( -1.000000000000000000, 0.000000000000000000, 0.000000000000000000 ) ) ;
#30060 = ORIENTED_EDGE ( 'NONE', *, *, #7815, .F. ) ;
#30061 = DIRECTION ( 'NONE',  ( 0.7416830501633135952, 0.6707505147970024284, -0.000000000000000000 ) ) ;
#30062 = ORIENTED_EDGE ( 'NONE', *, *, #6175, .T. ) ;
#30063 = CARTESIAN_POINT ( 'NONE',  ( 28.78283879316666471, -7.125616703334846314, 45.34931131770218826 ) ) ;
#30064 = CARTESIAN_POINT ( 'NONE',  ( -16.81371235015666699, 2.650171115930294974, 19.41069149716887310 ) ) ;
#30065 = ADVANCED_FACE ( 'NONE', ( #14904 ), #5398, .F. ) ;
#30066 = ORIENTED_EDGE ( 'NONE', *, *, #27513, .T. ) ;
#30067 = EDGE_CURVE ( 'NONE', #8808, #25145, #6945, .T. ) ;
#30068 = CARTESIAN_POINT ( 'NONE',  ( 11.40980092660686118, 6.310027164379057751, 1.500000000000001332 ) ) ;
#30069 = CARTESIAN_POINT ( 'NONE',  ( 22.62972083932141487, -34.62032468731402446, 29.57672015196555293 ) ) ;
#30070 = LINE ( 'NONE', #1838, #3334 ) ;
#30071 = AXIS2_PLACEMENT_3D ( 'NONE', #27435, #3726, #25081 ) ;
#30072 = CARTESIAN_POINT ( 'NONE',  ( -7.671865949551461838, -15.25812906914210032, 19.36813350477385143 ) ) ;
#30073 = B_SPLINE_CURVE_WITH_KNOTS ( 'NONE', 3,
 ( #6384, #13419, #20417, #6067, #11059, #3578, #20559, #8424, #3894, #13255, #25247, #13099, #3738, #27600, #1548, #15575, #22901, #18233, #15418, #1243, #22743, #30084, #1403, #8719 ),
 .UNSPECIFIED., .F., .F.,
 ( 4, 2, 2, 2, 2, 2, 2, 2, 2, 2, 2, 4 ),
 ( 0.000000000000000000, 0.002009995092672920650, 0.003014992639009388999, 0.004019990185345856913, 0.006029985278018779732, 0.007034982824355240708, 0.008039980370691701683, 0.009044977917028164394, 0.01004997546336462363, 0.01205997055603754732, 0.01406996564871046927, 0.01607996074138339296 ),
 .UNSPECIFIED. ) ;
#30074 = CARTESIAN_POINT ( 'NONE',  ( -5.544451647051929832, 16.11829164193972019, 7.652108011868850923 ) ) ;
#30075 = AXIS2_PLACEMENT_3D ( 'NONE', #11375, #20869, #27601 ) ;
#30076 = CARTESIAN_POINT ( 'NONE',  ( 1.438332125858173605, -8.884323311075778662, 1.500000000000001332 ) ) ;
#30077 = FACE_BOUND ( 'NONE', #28460, .T. ) ;
#30078 = VERTEX_POINT ( 'NONE', #29415 ) ;
#30079 = CIRCLE ( 'NONE', #28024, 0.7500000000000004441 ) ;
#30080 = CARTESIAN_POINT ( 'NONE',  ( 10.39243974596413089, -13.53611166824775935, 18.56793045041961321 ) ) ;
#30081 = CARTESIAN_POINT ( 'NONE',  ( 15.85884089648733131, 35.55173462727347555, 27.50000000000001066 ) ) ;
#30082 = ORIENTED_EDGE ( 'NONE', *, *, #16806, .T. ) ;
#30083 = ORIENTED_EDGE ( 'NONE', *, *, #2026, .T. ) ;
#30084 = CARTESIAN_POINT ( 'NONE',  ( 49.93149649555489589, 70.00033699790037645, 21.15209104779357574 ) ) ;
#30085 = CARTESIAN_POINT ( 'NONE',  ( 13.00999358272542850, -0.8602714556717643291, 1.500000000000001332 ) ) ;
#30086 = CARTESIAN_POINT ( 'NONE',  ( -5.512483845762028878, 16.12829592175436488, 5.651989602109218858 ) ) ;
#30087 = VERTEX_POINT ( 'NONE', #12727 ) ;
#30088 = CARTESIAN_POINT ( 'NONE',  ( -0.8750451464063154772, -9.041888939645135181, -1.500000000000002887 ) ) ;
#30089 = LINE ( 'NONE', #11379, #715 ) ;
#30090 = DIRECTION ( 'NONE',  ( -0.000000000000000000, -0.000000000000000000, -1.000000000000000000 ) ) ;
#30091 = ORIENTED_EDGE ( 'NONE', *, *, #20782, .T. ) ;
#30092 = B_SPLINE_CURVE_WITH_KNOTS ( 'NONE', 3,
 ( #15960, #4100, #13482, #22963 ),
 .UNSPECIFIED., .F., .F.,
 ( 4, 4 ),
 ( 2.143643656948718959E-07, 0.003421830178490221138 ),
 .UNSPECIFIED. ) ;
#30093 = PLANE ( 'NONE',  #10775 ) ;
#30094 = DIRECTION ( 'NONE',  ( 0.000000000000000000, -1.132880637372608986E-16, 1.000000000000000000 ) ) ;
#30095 = ORIENTED_EDGE ( 'NONE', *, *, #16997, .F. ) ;
#30096 = DIRECTION ( 'NONE',  ( 0.000000000000000000, 0.000000000000000000, 1.000000000000000000 ) ) ;
#30097 = AXIS2_PLACEMENT_3D ( 'NONE', #21155, #23653, #26636 ) ;
#30098 = EDGE_LOOP ( 'NONE', ( #29185, #15466 ) ) ;
#30099 = LINE ( 'NONE', #13874, #21874 ) ;
#30100 = PRODUCT_DEFINITION_CONTEXT ( 'detailed design', #5613, 'design' ) ;
#30101 = VERTEX_POINT ( 'NONE', #403 ) ;
#30102 = ORIENTED_EDGE ( 'NONE', *, *, #1798, .F. ) ;
#30103 = CARTESIAN_POINT ( 'NONE',  ( 3.529212228261832340, 16.69261290539734688, 7.500147780736496017 ) ) ;
#30104 = DIRECTION ( 'NONE',  ( 0.000000000000000000, 1.000000000000000000, 0.000000000000000000 ) ) ;
#30105 = CARTESIAN_POINT ( 'NONE',  ( 6.236311564447698075, 19.00292092786887110, 19.08232364404840453 ) ) ;
#30106 = ORIENTED_EDGE ( 'NONE', *, *, #13942, .T. ) ;
#30107 = CARTESIAN_POINT ( 'NONE',  ( -4.677126025380971441, -39.24912351428226742, 34.80090346875804386 ) ) ;
#30108 = CARTESIAN_POINT ( 'NONE',  ( 33.56327786402390245, -10.34181101807379477, 39.87954049117192312 ) ) ;
#30109 = CARTESIAN_POINT ( 'NONE',  ( 16.83479397774491915, 2.565335765644451094, 20.12545155307891065 ) ) ;
#30110 = ORIENTED_EDGE ( 'NONE', *, *, #21160, .F. ) ;
#30111 = ADVANCED_FACE ( 'NONE', ( #19899 ), #2908, .F. ) ;
#30112 = DIRECTION ( 'NONE',  ( 0.000000000000000000, 1.000000000000000000, 0.000000000000000000 ) ) ;
#30113 = CARTESIAN_POINT ( 'NONE',  ( 15.38564065975360506, -7.280544306537537480, 6.755862304746362845 ) ) ;
#30114 = CARTESIAN_POINT ( 'NONE',  ( -15.40675500887359028, 12.78077869785447440, 5.652605728828375753 ) ) ;
#30115 = CARTESIAN_POINT ( 'NONE',  ( 3.064607854149369981, 16.80099270350294915, 19.47783254395485031 ) ) ;
#30116 = ORIENTED_EDGE ( 'NONE', *, *, #18796, .F. ) ;
#30117 = ORIENTED_EDGE ( 'NONE', *, *, #21033, .F. ) ;
#30118 = DIRECTION ( 'NONE',  ( 1.000000000000000000, 0.000000000000000000, 0.000000000000000000 ) ) ;
#30119 = LINE ( 'NONE', #27481, #8155 ) ;
#30120 = CARTESIAN_POINT ( 'NONE',  ( -4.594331223478842929, 16.38995132059639204, 19.11611934778430921 ) ) ;
#30121 = CARTESIAN_POINT ( 'NONE',  ( -6.543385983536390782, -6.301234758012574488, 13.22130136205108819 ) ) ;
#30122 = DIRECTION ( 'NONE',  ( 1.000000000000000000, 0.000000000000000000, 0.000000000000000000 ) ) ;
#30123 = CARTESIAN_POINT ( 'NONE',  ( 35.13669516613780530, 8.778141986578262390, 34.58384122122917148 ) ) ;
#30124 = CONTEXT_DEPENDENT_SHAPE_REPRESENTATION ( #11218, #5461 ) ;
#30125 = CARTESIAN_POINT ( 'NONE',  ( 23.44182307864140569, -12.68276878097691807, 48.34755156432018453 ) ) ;
#30126 = ORIENTED_EDGE ( 'NONE', *, *, #15674, .T. ) ;
#30127 = CARTESIAN_POINT ( 'NONE',  ( -16.96496223448355067, 1.652369715233091396, 7.652108011868850035 ) ) ;
#30128 = DIRECTION ( 'NONE',  ( 0.000000000000000000, 0.000000000000000000, 1.000000000000000000 ) ) ;
#30129 = CARTESIAN_POINT ( 'NONE',  ( 19.85631519639700215, 2.394924755340394285, 19.96302680909623817 ) ) ;
#30130 = ORIENTED_EDGE ( 'NONE', *, *, #20072, .F. ) ;
#30131 = DIRECTION ( 'NONE',  ( 1.000000000000000000, 0.000000000000000000, 0.000000000000000000 ) ) ;
#30132 = EDGE_CURVE ( 'NONE', #30406, #22536, #1024, .T. ) ;
#30133 = ORIENTED_EDGE ( 'NONE', *, *, #16209, .F. ) ;
#30134 = LINE ( 'NONE', #29527, #26213 ) ;
#30135 = CARTESIAN_POINT ( 'NONE',  ( -32.28307784207223108, -8.475829241206282560, 37.38016955275590902 ) ) ;
#30136 = ORIENTED_EDGE ( 'NONE', *, *, #16120, .T. ) ;
#30137 = LINE ( 'NONE', #20474, #1354 ) ;
#30138 = AXIS2_PLACEMENT_3D ( 'NONE', #13685, #18368, #27880 ) ;
#30139 = ADVANCED_FACE ( 'NONE', ( #5242 ), #10219, .F. ) ;
#30140 = CARTESIAN_POINT ( 'NONE',  ( 0.000000000000000000, -8.043452525345523162E-15, -16.50000000000000000 ) ) ;
#30141 = EDGE_CURVE ( 'NONE', #26457, #9428, #6844, .T. ) ;
#30142 = CARTESIAN_POINT ( 'NONE',  ( -4.163336342344337027E-14, -1.387778780781445676E-14, 1.500000000000000000 ) ) ;
#30143 = DIRECTION ( 'NONE',  ( -0.2817325568414296710, 0.9594929736144973687, -0.000000000000000000 ) ) ;
#30144 = CYLINDRICAL_SURFACE ( 'NONE', #9328, 1.447898107987198646 ) ;
#30145 = CARTESIAN_POINT ( 'NONE',  ( 37.16608720827707657, -65.00000000000000000, 12.49999999999999112 ) ) ;
#30146 = CARTESIAN_POINT ( 'NONE',  ( -32.06827542805550024, 14.53851282002520762, 39.79035104390202804 ) ) ;
#30147 = EDGE_CURVE ( 'NONE', #1290, #11660, #15829, .T. ) ;
#30148 = ORIENTED_EDGE ( 'NONE', *, *, #11495, .F. ) ;
#30149 = EDGE_CURVE ( 'NONE', #8380, #17431, #29284, .T. ) ;
#30150 = PLANE ( 'NONE',  #4873 ) ;
#30151 = CARTESIAN_POINT ( 'NONE',  ( 7.538175180318423152, 5.069257791428403159, -1.500000000000001110 ) ) ;
#30152 = CARTESIAN_POINT ( 'NONE',  ( -4.574230723433014845, 16.39514892286268832, 6.519181285484531685 ) ) ;
#30153 = EDGE_CURVE ( 'NONE', #8558, #19615, #1494, .T. ) ;
#30154 = DIRECTION ( 'NONE',  ( 1.000000000000000000, 0.000000000000000000, 0.000000000000000000 ) ) ;
#30155 = CARTESIAN_POINT ( 'NONE',  ( 34.07766914598172292, -21.40380666527112652, -1.500000000000000000 ) ) ;
#30156 = CARTESIAN_POINT ( 'NONE',  ( 32.81350286003733885, 0.000000000000000000, -6.500000000000000888 ) ) ;
#30157 = ORIENTED_EDGE ( 'NONE', *, *, #24828, .T. ) ;
#30158 = CARTESIAN_POINT ( 'NONE',  ( -70.00000000000000000, 50.00000000000000000, -92.50000000000000000 ) ) ;
#30159 = AXIS2_PLACEMENT_3D ( 'NONE', #4535, #23405, #23698 ) ;
#30160 = CARTESIAN_POINT ( 'NONE',  ( 12.56641067637628240, -40.32935944494942504, -1.500000000000000000 ) ) ;
#30161 = CARTESIAN_POINT ( 'NONE',  ( 36.51087454057529413, -15.00302545122030295, 34.85625572976320541 ) ) ;
#30162 = CARTESIAN_POINT ( 'NONE',  ( -4.163336342344337027E-14, 1.387778780781445676E-14, 24.50000000000000000 ) ) ;
#30163 = ORIENTED_EDGE ( 'NONE', *, *, #11319, .F. ) ;
#30164 = CARTESIAN_POINT ( 'NONE',  ( -25.23756106473024374, 11.43858098102958110, -16.50000000000000000 ) ) ;
#30165 = EDGE_LOOP ( 'NONE', ( #23175, #1241 ) ) ;
#30166 = CARTESIAN_POINT ( 'NONE',  ( 0.000000000000000000, 0.000000000000000000, -52.50000000000000000 ) ) ;
#30167 = CARTESIAN_POINT ( 'NONE',  ( 18.58529988941438305, 7.388276390372289448, 1.500000000000001332 ) ) ;
#30168 = EDGE_CURVE ( 'NONE', #13757, #4954, #20357, .T. ) ;
#30169 = ORIENTED_EDGE ( 'NONE', *, *, #6125, .T. ) ;
#30170 = EDGE_CURVE ( 'NONE', #19220, #3711, #20041, .T. ) ;
#30171 = DIRECTION ( 'NONE',  ( 0.000000000000000000, 1.000000000000000000, 6.938893903907227392E-16 ) ) ;
#30172 =( GEOMETRIC_REPRESENTATION_CONTEXT ( 3 ) GLOBAL_UNCERTAINTY_ASSIGNED_CONTEXT ( ( #25143 ) ) GLOBAL_UNIT_ASSIGNED_CONTEXT ( ( #10547, #22078, #3214 ) ) REPRESENTATION_CONTEXT ( 'NONE', 'WORKASPACE' ) );
#30173 = ADVANCED_FACE ( 'NONE', ( #29712 ), #8523, .F. ) ;
#30174 = CARTESIAN_POINT ( 'NONE',  ( 19.72232476070952956, 3.323723214581398633, 20.34789198813115263 ) ) ;
#30175 = EDGE_LOOP ( 'NONE', ( #24656, #1336, #17045, #718 ) ) ;
#30176 = CARTESIAN_POINT ( 'NONE',  ( 11.21631477658333687, -16.55933310271405645, 7.652108011868850923 ) ) ;
#30177 = EDGE_CURVE ( 'NONE', #13645, #23441, #13505, .T. ) ;
#30178 = CARTESIAN_POINT ( 'NONE',  ( -49.99999999999998579, 90.00000000000001421, -75.50000000000002842 ) ) ;
#30179 = EDGE_LOOP ( 'NONE', ( #18730, #2856, #21474 ) ) ;
#30180 = DIRECTION ( 'NONE',  ( 1.000000000000000000, 0.000000000000000000, 0.000000000000000000 ) ) ;
#30181 = VECTOR ( 'NONE', #2377, 1000.000000000000000 ) ;
#30182 = DIRECTION ( 'NONE',  ( -0.000000000000000000, -0.000000000000000000, -1.000000000000000000 ) ) ;
#30183 = DIRECTION ( 'NONE',  ( -0.000000000000000000, -0.000000000000000000, 1.000000000000000000 ) ) ;
#30184 = EDGE_CURVE ( 'NONE', #19467, #22374, #22527, .T. ) ;
#30185 = CARTESIAN_POINT ( 'NONE',  ( -0.6883321258581104329, 8.884323311075791096, 21.50000000000000000 ) ) ;
#30186 = AXIS2_PLACEMENT_3D ( 'NONE', #19523, #29035, #12517 ) ;
#30187 = CARTESIAN_POINT ( 'NONE',  ( 16.17735844207722806, -3.336236224685152685, 1.500000000000000000 ) ) ;
#30188 = DIRECTION ( 'NONE',  ( 0.9898214418809327952, -0.1423148382732850048, 0.000000000000000000 ) ) ;
#30189 = LINE ( 'NONE', #27236, #17010 ) ;
#30190 = CARTESIAN_POINT ( 'NONE',  ( 19.62935297797556089, -3.832558109936518687, 24.50000000000000000 ) ) ;
#30191 = CARTESIAN_POINT ( 'NONE',  ( -18.29014699721057724, -8.135908015825712880, 20.19668224736330941 ) ) ;
#30192 = CARTESIAN_POINT ( 'NONE',  ( -9.069887158720549181, -14.41355491440999437, 18.54473042795394377 ) ) ;
#30193 = VECTOR ( 'NONE', #14285, 1000.000000000000000 ) ;
#30194 = ORIENTED_EDGE ( 'NONE', *, *, #23991, .T. ) ;
#30195 = ORIENTED_EDGE ( 'NONE', *, *, #19817, .F. ) ;
#30196 = DIRECTION ( 'NONE',  ( 0.000000000000000000, 1.000000000000000000, 1.193512090021232842E-16 ) ) ;
#30197 = CARTESIAN_POINT ( 'NONE',  ( -5.374868878256215510, -44.10336124695545124, -19.50000000000000355 ) ) ;
#30198 = EDGE_CURVE ( 'NONE', #14669, #584, #22987, .T. ) ;
#30199 = CARTESIAN_POINT ( 'NONE',  ( -1.438332125858111432, 8.884323311075791096, -1.500000000000000888 ) ) ;
#30200 = VERTEX_POINT ( 'NONE', #11155 ) ;
#30201 =( NAMED_UNIT ( * ) PLANE_ANGLE_UNIT ( ) SI_UNIT ( $, .RADIAN. ) );
#30202 = EDGE_CURVE ( 'NONE', #19910, #23254, #9839, .T. ) ;
#30203 = DIRECTION ( 'NONE',  ( 1.000000000000000000, 0.000000000000000000, -0.000000000000000000 ) ) ;
#30204 = DIRECTION ( 'NONE',  ( 1.000000000000000000, 0.000000000000000000, 0.000000000000000000 ) ) ;
#30205 = CIRCLE ( 'NONE', #23701, 7.500000000000013323 ) ;
#30206 = ORIENTED_EDGE ( 'NONE', *, *, #25241, .F. ) ;
#30207 = CARTESIAN_POINT ( 'NONE',  ( -11.33851205691660979, -16.47545820588254273, 19.60917204426170457 ) ) ;
#30208 = AXIS2_PLACEMENT_3D ( 'NONE', #25656, #4275, #11008 ) ;
#30209 = AXIS2_PLACEMENT_3D ( 'NONE', #24373, #2556, #5047 ) ;
#30210 = CARTESIAN_POINT ( 'NONE',  ( -10.80882669148404851, -16.84912922860908679, 18.39701043959520987 ) ) ;
#30211 = CARTESIAN_POINT ( 'NONE',  ( -10.00384078742051663, 41.10499445384696315, 34.57841144790000953 ) ) ;
#30212 = ORIENTED_EDGE ( 'NONE', *, *, #19663, .T. ) ;
#30213 = ORIENTED_EDGE ( 'NONE', *, *, #4955, .F. ) ;
#30214 = CARTESIAN_POINT ( 'NONE',  ( -14.70309389971832204, -8.688337726274227180, 6.783738457429057789 ) ) ;
#30215 = CARTESIAN_POINT ( 'NONE',  ( -14.76283269969004230, 13.49301113316031042, 7.156831654632813233 ) ) ;
#30216 = AXIS2_PLACEMENT_3D ( 'NONE', #3966, #1626, #13772 ) ;
#30217 = EDGE_LOOP ( 'NONE', ( #29210, #3426, #29341 ) ) ;
#30218 = LINE ( 'NONE', #14130, #7871 ) ;
#30219 = CARTESIAN_POINT ( 'NONE',  ( 24.44496207165490631, -7.595930209050163029, 45.15942333309103418 ) ) ;
#30220 = DIRECTION ( 'NONE',  ( 0.000000000000000000, 0.000000000000000000, -1.000000000000000000 ) ) ;
#30221 = CARTESIAN_POINT ( 'NONE',  ( 0.7788148826605766351, -17.02744010918315709, 7.652108011868850035 ) ) ;
#30222 = VECTOR ( 'NONE', #3522, 1000.000000000000000 ) ;
#30223 = CARTESIAN_POINT ( 'NONE',  ( -39.52380524536136619, -7.028748154183644736, -11.49999999999999645 ) ) ;
#30224 = AXIS2_PLACEMENT_3D ( 'NONE', #2522, #11722, #167 ) ;
#30225 = CARTESIAN_POINT ( 'NONE',  ( -17.05621956093628810, 0.7704973847275167209, 19.85459532544247097 ) ) ;
#30226 = LINE ( 'NONE', #6374, #10029 ) ;
#30227 = CARTESIAN_POINT ( 'NONE',  ( -2.352830851074180440, -9.185733585337901630, 13.00000000000000178 ) ) ;
#30228 = ORIENTED_EDGE ( 'NONE', *, *, #4646, .T. ) ;
#30229 = AXIS2_PLACEMENT_3D ( 'NONE', #6812, #1681, #20695 ) ;
#30230 = CARTESIAN_POINT ( 'NONE',  ( 10.05214800432092304, -13.77402237313446420, 18.37415474056476938 ) ) ;
#30231 = AXIS2_PLACEMENT_3D ( 'NONE', #8610, #18439, #9061 ) ;
#30232 = CARTESIAN_POINT ( 'NONE',  ( 23.69412710310942316, 29.84645176427128277, 27.50000000000000355 ) ) ;
#30233 = ORIENTED_EDGE ( 'NONE', *, *, #4224, .F. ) ;
#30234 = EDGE_LOOP ( 'NONE', ( #28542, #4671 ) ) ;
#30235 = DIRECTION ( 'NONE',  ( -0.000000000000000000, 0.000000000000000000, 1.000000000000000000 ) ) ;
#30236 = B_SPLINE_CURVE_WITH_KNOTS ( 'NONE', 3,
 ( #30035, #9272, #20662, #13667 ),
 .UNSPECIFIED., .F., .F.,
 ( 4, 4 ),
 ( 2.143643656964903906E-07, 0.003421830178490235450 ),
 .UNSPECIFIED. ) ;
#30237 = CARTESIAN_POINT ( 'NONE',  ( -5.655446062488478809, 19.20259930434394491, 5.701226463332907279 ) ) ;
#30238 = ORIENTED_EDGE ( 'NONE', *, *, #11693, .T. ) ;
#30239 = LINE ( 'NONE', #11954, #18566 ) ;
#30240 = VECTOR ( 'NONE', #4866, 1000.000000000000000 ) ;
#30241 = CARTESIAN_POINT ( 'NONE',  ( -13.37849590498012908, 10.56201291617988147, 7.652108011868850923 ) ) ;
#30242 = CARTESIAN_POINT ( 'NONE',  ( 23.44138668973443984, 12.68271180600415882, 48.34797144684549863 ) ) ;
#30243 = VERTEX_POINT ( 'NONE', #17700 ) ;
#30244 = DIRECTION ( 'NONE',  ( -0.000000000000000000, -0.000000000000000000, -1.000000000000000000 ) ) ;
#30245 = CARTESIAN_POINT ( 'NONE',  ( 19.76052160831509852, 3.198927888535953112, 5.652196082367002994 ) ) ;
#30246 = ORIENTED_EDGE ( 'NONE', *, *, #24041, .T. ) ;
#30247 = CIRCLE ( 'NONE', #27268, 0.7500000000000015543 ) ;
#30248 = DIRECTION ( 'NONE',  ( -0.000000000000000000, -0.000000000000000000, 1.000000000000000000 ) ) ;
#30249 = EDGE_LOOP ( 'NONE', ( #20554, #1217, #25351, #3332 ) ) ;
#30250 = ORIENTED_EDGE ( 'NONE', *, *, #10939, .F. ) ;
#30251 = ORIENTED_EDGE ( 'NONE', *, *, #1710, .T. ) ;
#30252 = AXIS2_PLACEMENT_3D ( 'NONE', #246, #16168, #25845 ) ;
#30253 = LINE ( 'NONE', #3447, #22540 ) ;
#30254 = DIRECTION ( 'NONE',  ( 0.000000000000000000, 0.000000000000000000, -1.000000000000000000 ) ) ;
#30255 = VECTOR ( 'NONE', #21535, 1000.000000000000000 ) ;
#30256 = VERTEX_POINT ( 'NONE', #20186 ) ;
#30257 = CIRCLE ( 'NONE', #18341, 9.482273699623480212 ) ;
#30258 = LINE ( 'NONE', #8824, #24772 ) ;
#30259 = CARTESIAN_POINT ( 'NONE',  ( 9.496768069075219643, -14.14083042221133368, 18.44501272782439827 ) ) ;
#30260 = CARTESIAN_POINT ( 'NONE',  ( 19.79689803950977378, 2.967719242317201633, 20.32842677360128292 ) ) ;
#30261 = VERTEX_POINT ( 'NONE', #24885 ) ;
#30262 = CIRCLE ( 'NONE', #16815, 0.7441270634457181066 ) ;
#30263 = DIRECTION ( 'NONE',  ( 0.000000000000000000, 0.000000000000000000, -1.000000000000000000 ) ) ;
#30264 = CARTESIAN_POINT ( 'NONE',  ( 15.42605794595427682, -7.198932956632624780, 7.080843742048788414 ) ) ;
#30265 = CIRCLE ( 'NONE', #13820, 20.00000000000000000 ) ;
#30266 = CARTESIAN_POINT ( 'NONE',  ( -15.98738144660409866, 12.04609795553196960, 6.672349528511551497 ) ) ;
#30267 = CARTESIAN_POINT ( 'NONE',  ( 4.365174083970718932, 19.53587658871429156, 19.03762469184452755 ) ) ;
#30268 = ORIENTED_EDGE ( 'NONE', *, *, #7292, .F. ) ;
#30269 = VERTEX_POINT ( 'NONE', #20651 ) ;
#30270 = CIRCLE ( 'NONE', #15821, 9.482273699623480212 ) ;
#30271 = CARTESIAN_POINT ( 'NONE',  ( 0.000000000000000000, 0.000000000000000000, 1.500000000000001332 ) ) ;
#30272 = DIRECTION ( 'NONE',  ( -1.000000000000000000, 0.000000000000000000, 0.000000000000000000 ) ) ;
#30273 = DIRECTION ( 'NONE',  ( 0.000000000000000000, -1.000000000000000000, 0.000000000000000000 ) ) ;
#30274 =( NAMED_UNIT ( * ) PLANE_ANGLE_UNIT ( ) SI_UNIT ( $, .RADIAN. ) );
#30275 = CARTESIAN_POINT ( 'NONE',  ( 6.899999999999999467, 9.000000000000000000, 0.000000000000000000 ) ) ;
#30276 = FACE_OUTER_BOUND ( 'NONE', #18685, .T. ) ;
#30277 = CARTESIAN_POINT ( 'NONE',  ( 24.35970437652574816, -13.37404834226503958, 42.96778633356033339 ) ) ;
#30278 = VECTOR ( 'NONE', #2650, 1000.000000000000000 ) ;
#30279 = VERTEX_POINT ( 'NONE', #6160 ) ;
#30280 = VECTOR ( 'NONE', #25395, 1000.000000000000114 ) ;
#30281 = CARTESIAN_POINT ( 'NONE',  ( -17.02496544227784980, 1.117683430491698271, 7.500147780736496017 ) ) ;
#30282 = AXIS2_PLACEMENT_3D ( 'NONE', #23036, #22894, #8570 ) ;
#30283 = FACE_OUTER_BOUND ( 'NONE', #8450, .T. ) ;
#30284 = CARTESIAN_POINT ( 'NONE',  ( 48.64405085385529759, -18.29172496293579542, 24.50000000000000355 ) ) ;
#30285 = ORIENTED_EDGE ( 'NONE', *, *, #7466, .T. ) ;
#30286 = DIRECTION ( 'NONE',  ( 1.000000000000000000, 0.000000000000000000, 0.000000000000000000 ) ) ;
#30287 = EDGE_LOOP ( 'NONE', ( #6474, #14553, #4891, #24413 ) ) ;
#30288 = DIRECTION ( 'NONE',  ( -1.156482317317873105E-15, 1.000000000000000000, 0.000000000000000000 ) ) ;
#30289 = AXIS2_PLACEMENT_3D ( 'NONE', #8701, #20540, #18827 ) ;
#30290 = DIRECTION ( 'NONE',  ( 1.000000000000000000, 0.000000000000000000, 0.000000000000000000 ) ) ;
#30291 = ORIENTED_EDGE ( 'NONE', *, *, #25987, .F. ) ;
#30292 = CARTESIAN_POINT ( 'NONE',  ( -0.6312581325461305015, -19.99009984789270433, 6.913388067999412634 ) ) ;
#30293 = VECTOR ( 'NONE', #11607, 1000.000000000000000 ) ;
#30294 = CARTESIAN_POINT ( 'NONE',  ( 12.19428753565139090, 48.49100318506136631, -63.74847735431697515 ) ) ;
#30295 = DIRECTION ( 'NONE',  ( -1.000000000000000000, 0.000000000000000000, 0.000000000000000000 ) ) ;
#30296 = CARTESIAN_POINT ( 'NONE',  ( -20.71335220384823117, -27.86167394782616213, -16.50000000000000000 ) ) ;
#30297 = FACE_OUTER_BOUND ( 'NONE', #3696, .T. ) ;
#30298 = LINE ( 'NONE', #13632, #12840 ) ;
#30299 = CARTESIAN_POINT ( 'NONE',  ( 0.9279538312821420387, -17.02439129904410819, 7.643931100913408550 ) ) ;
#30300 = EDGE_LOOP ( 'NONE', ( #21971, #14437, #10938, #6896 ) ) ;
#30301 = CIRCLE ( 'NONE', #16855, 27.70876437800068359 ) ;
#30302 = CIRCLE ( 'NONE', #21319, 0.7441270634456903510 ) ;
#30303 = CARTESIAN_POINT ( 'NONE',  ( 8.197313248159948884, -3.914781618004724795, 21.50000000000000000 ) ) ;
#30304 = CARTESIAN_POINT ( 'NONE',  ( 24.03057240117691862, -26.57182937991349903, 1.500000000000000000 ) ) ;
#30305 = ADVANCED_FACE ( 'NONE', ( #3524 ), #27388, .T. ) ;
#30306 = DIRECTION ( 'NONE',  ( -0.000000000000000000, -0.000000000000000000, 1.000000000000000000 ) ) ;
#30307 = CARTESIAN_POINT ( 'NONE',  ( -17.96015518819251255, -8.839856506746547993, 18.37415474056476938 ) ) ;
#30308 = CARTESIAN_POINT ( 'NONE',  ( -31.18700685316100163, -26.11823559932341610, -1.500000000000000000 ) ) ;
#30309 = PLANE ( 'NONE',  #13623 ) ;
#30310 = AXIS2_PLACEMENT_3D ( 'NONE', #23297, #1940, #2984 ) ;
#30311 = ORIENTED_EDGE ( 'NONE', *, *, #10108, .F. ) ;
#30312 = CARTESIAN_POINT ( 'NONE',  ( 7.730328572437743517, -4.608906612435629491, 1.500000000000001332 ) ) ;
#30313 = CARTESIAN_POINT ( 'NONE',  ( 49.99999999999998579, 70.00000000000000000, -34.50000000000000000 ) ) ;
#30314 = CARTESIAN_POINT ( 'NONE',  ( 21.45876801738695860, -30.77697269628944809, 37.49999999998526334 ) ) ;
#30315 = ADVANCED_FACE ( 'NONE', ( #5855 ), #13037, .F. ) ;
#30316 = DIRECTION ( 'NONE',  ( -0.4154150130018840481, 0.9096319953545194403, 0.000000000000000000 ) ) ;
#30317 = ORIENTED_EDGE ( 'NONE', *, *, #27178, .F. ) ;
#30318 = FACE_OUTER_BOUND ( 'NONE', #21575, .T. ) ;
#30319 = CARTESIAN_POINT ( 'NONE',  ( -23.96732207939035675, 33.98584080153585774, -1.500000000000000000 ) ) ;
#30320 = CARTESIAN_POINT ( 'NONE',  ( 49.99999999999998579, -50.00000000000000000, -92.50000000000000000 ) ) ;
#30321 = AXIS2_PLACEMENT_3D ( 'NONE', #2432, #30497, #21447 ) ;
#30322 = VERTEX_POINT ( 'NONE', #20502 ) ;
#30323 = B_SPLINE_SURFACE_WITH_KNOTS ( 'NONE', 3, 1, ( 
 ( #11048, #30221 ),
 ( #2136, #6520 ),
 ( #6979, #11514 ),
 ( #1538, #6663 ),
 ( #28182, #16030 ),
 ( #25547, #20855 ),
 ( #30381, #4487 ),
 ( #11654, #18837 ),
 ( #28355, #16490 ),
 ( #26007, #13402 ),
 ( #9019, #18531 ),
 ( #28034, #25694 ),
 ( #4322, #18991 ),
 ( #14283, #12123 ),
 ( #29110, #560 ),
 ( #21776, #28959 ),
 ( #24271, #7594 ),
 ( #24112, #16792 ),
 ( #19286, #17255 ),
 ( #10080, #30828 ),
 ( #9625, #19136 ),
 ( #21623, #106 ),
 ( #28501, #12274 ),
 ( #9474, #28652 ),
 ( #415, #21465 ),
 ( #23958, #7751 ),
 ( #7444, #16644 ),
 ( #26466, #5098 ),
 ( #17099, #19442 ),
 ( #7133, #19593 ),
 ( #9933, #14456 ) ),
 .UNSPECIFIED., .F., .F., .F.,
 ( 4, 3, 3, 3, 3, 3, 3, 3, 3, 3, 4 ),
 ( 2, 2 ),
 ( 0.000000000000000000, 0.05425176834609633791, 0.1085332949128352958, 0.1623767749169382768, 0.2157504826133063158, 0.2688657508888171455, 0.3218907763505476360, 0.3749548578363336993, 0.4282048033836242107, 0.4818374082110501444, 0.4999999999131654604 ),
 ( 0.000000000000000000, 1.000000000000000000 ),
 .UNSPECIFIED. ) ;
#30324 = VECTOR ( 'NONE', #10622, 1000.000000000000000 ) ;
#30325 = EDGE_CURVE ( 'NONE', #3241, #19329, #6168, .T. ) ;
#30326 = VECTOR ( 'NONE', #12683, 1000.000000000000000 ) ;
#30327 = CARTESIAN_POINT ( 'NONE',  ( 19.63503467057052632, 3.804509661152922106, 20.15039051365864253 ) ) ;
#30328 = VERTEX_POINT ( 'NONE', #22474 ) ;
#30329 = CARTESIAN_POINT ( 'NONE',  ( -31.76816150360384228, 26.51947378168403091, -11.49999299997503499 ) ) ;
#30330 = EDGE_CURVE ( 'NONE', #16378, #16205, #7264, .T. ) ;
#30331 = CARTESIAN_POINT ( 'NONE',  ( -8.353478261420262285, -14.86569112999328901, 5.678370764302467677 ) ) ;
#30332 = LINE ( 'NONE', #8672, #25311 ) ;
#30333 = VECTOR ( 'NONE', #11780, 1000.000000000000227 ) ;
#30334 = CARTESIAN_POINT ( 'NONE',  ( 6.899999999999999467, 5.196152422706634688, -9.000000000000001776 ) ) ;
#30335 = ORIENTED_EDGE ( 'NONE', *, *, #26718, .F. ) ;
#30336 = DIRECTION ( 'NONE',  ( 1.000000000000000000, 0.000000000000000000, 0.000000000000000000 ) ) ;
#30337 = DIRECTION ( 'NONE',  ( 1.000000000000000000, 0.000000000000000000, 0.000000000000000000 ) ) ;
#30338 = CARTESIAN_POINT ( 'NONE',  ( 39.99999999999998579, 87.00000000000001421, 52.49999999999999289 ) ) ;
#30339 = LINE ( 'NONE', #28150, #10297 ) ;
#30340 = CIRCLE ( 'NONE', #11, 1.000000000000000888 ) ;
#30341 = CARTESIAN_POINT ( 'NONE',  ( -15.56507824124931894, -6.890134373242267962, 19.60617949693493145 ) ) ;
#30342 = CARTESIAN_POINT ( 'NONE',  ( 32.24119435725080507, -26.76047165977712794, -16.50000600000000262 ) ) ;
#30343 = LINE ( 'NONE', #21113, #20983 ) ;
#30344 = CARTESIAN_POINT ( 'NONE',  ( 3.062151163506447116, 16.80153468414596674, 19.28454053338348828 ) ) ;
#30345 = DIRECTION ( 'NONE',  ( 0.000000000000000000, 0.000000000000000000, 1.000000000000000000 ) ) ;
#30346 = EDGE_CURVE ( 'NONE', #26457, #14352, #25784, .T. ) ;
#30347 = EDGE_CURVE ( 'NONE', #23472, #23537, #24189, .T. ) ;
#30348 = DIRECTION ( 'NONE',  ( 0.000000000000000000, 0.000000000000000000, 1.000000000000000000 ) ) ;
#30349 = CARTESIAN_POINT ( 'NONE',  ( -2.107417972768699244E-15, 8.236864015571832454, -3.733333029993799013 ) ) ;
#30350 = AXIS2_PLACEMENT_3D ( 'NONE', #7412, #24824, #10629 ) ;
#30351 = ORIENTED_EDGE ( 'NONE', *, *, #15480, .F. ) ;
#30352 = ORIENTED_EDGE ( 'NONE', *, *, #16543, .T. ) ;
#30353 = DIRECTION ( 'NONE',  ( -0.000000000000000000, 1.000000000000000000, -0.000000000000000000 ) ) ;
#30354 = CARTESIAN_POINT ( 'NONE',  ( 34.07766914598172292, -21.40380666527112652, -1.500000000000000000 ) ) ;
#30355 = DIRECTION ( 'NONE',  ( 0.000000000000000000, -0.000000000000000000, -1.000000000000000000 ) ) ;
#30356 = EDGE_CURVE ( 'NONE', #606, #10785, #28281, .T. ) ;
#30357 = EDGE_LOOP ( 'NONE', ( #19000, #16881 ) ) ;
#30358 = SHAPE_REPRESENTATION_RELATIONSHIP ( 'NONE' , 'NONE' ,  #10307, #2065 ) ;
#30359 = CIRCLE ( 'NONE', #24884, 0.6002263538043630664 ) ;
#30360 = CARTESIAN_POINT ( 'NONE',  ( -37.99999999999999289, 70.00000000000000000, -28.49999999999998934 ) ) ;
#30361 = CYLINDRICAL_SURFACE ( 'NONE', #13183, 3.559164065751841743 ) ;
#30362 = ADVANCED_FACE ( 'NONE', ( #7685 ), #17183, .F. ) ;
#30363 = EDGE_CURVE ( 'NONE', #27143, #8558, #2873, .T. ) ;
#30364 = ORIENTED_EDGE ( 'NONE', *, *, #27256, .T. ) ;
#30365 = CARTESIAN_POINT ( 'NONE',  ( -16.89118935510124331, 2.183074208216230883, 5.796888747622817029 ) ) ;
#30366 = B_SPLINE_CURVE_WITH_KNOTS ( 'NONE', 3,
 ( #26691, #12815, #3288, #5946, #22005, #639 ),
 .UNSPECIFIED., .F., .F.,
 ( 4, 2, 4 ),
 ( 0.01057608626846272791, 0.01589305904739927652, 0.02121003182633582687 ),
 .UNSPECIFIED. ) ;
#30367 = VECTOR ( 'NONE', #15952, 1000.000000000000000 ) ;
#30368 = B_SPLINE_CURVE_WITH_KNOTS ( 'NONE', 3,
 ( #2673, #17017, #23714, #24, #12188, #4857 ),
 .UNSPECIFIED., .F., .F.,
 ( 4, 2, 4 ),
 ( 0.03045342003272953624, 0.03308352805739835090, 0.03571363608206717249 ),
 .UNSPECIFIED. ) ;
#30369 = DIRECTION ( 'NONE',  ( -0.000000000000000000, -0.000000000000000000, 1.000000000000000000 ) ) ;
#30370 = LINE ( 'NONE', #1528, #23436 ) ;
#30371 = EDGE_LOOP ( 'NONE', ( #723, #1850 ) ) ;
#30372 = CARTESIAN_POINT ( 'NONE',  ( -40.00000000000002842, 80.00000000000001421, 52.50000000000014921 ) ) ;
#30373 = EDGE_CURVE ( 'NONE', #6658, #2444, #20310, .T. ) ;
#30374 = VERTEX_POINT ( 'NONE', #650 ) ;
#30375 = CARTESIAN_POINT ( 'NONE',  ( 2.599508007902112006, -14.29059753516471964, 1.500000000000000000 ) ) ;
#30376 = CARTESIAN_POINT ( 'NONE',  ( -6.587096388939656322, -18.88412458026101604, 1.500000000000001332 ) ) ;
#30377 = VERTEX_POINT ( 'NONE', #22172 ) ;
#30378 = DIRECTION ( 'NONE',  ( -1.000000000000000000, 0.000000000000000000, 0.000000000000000000 ) ) ;
#30379 = CYLINDRICAL_SURFACE ( 'NONE', #1346, 0.7441270634456903510 ) ;
#30380 = CARTESIAN_POINT ( 'NONE',  ( 14.28398042828922421, -41.31607170670246632, -16.50000000000000000 ) ) ;
#30381 = CARTESIAN_POINT ( 'NONE',  ( -0.2861250491275375563, -20.01582202454545723, 7.429667576816606278 ) ) ;
#30382 = AXIS2_PLACEMENT_3D ( 'NONE', #4426, #16732, #23742 ) ;
#30383 = DIRECTION ( 'NONE',  ( -0.000000000000000000, -0.000000000000000000, -1.000000000000000000 ) ) ;
#30384 = DIRECTION ( 'NONE',  ( 0.000000000000000000, -1.132880637372608986E-16, 1.000000000000000000 ) ) ;
#30385 = LINE ( 'NONE', #9316, #29945 ) ;
#30386 = CARTESIAN_POINT ( 'NONE',  ( 35.37867965644032608, 1.387778780781445676E-14, 35.37867965644034740 ) ) ;
#30387 = EDGE_LOOP ( 'NONE', ( #28171, #3718, #4880, #8386 ) ) ;
#30388 = EDGE_CURVE ( 'NONE', #24914, #14826, #17344, .T. ) ;
#30389 = ADVANCED_FACE ( 'NONE', ( #800 ), #22331, .F. ) ;
#30390 = CARTESIAN_POINT ( 'NONE',  ( 10.45210396439253842, -13.49311571392156495, 20.06253562465620632 ) ) ;
#30391 = CARTESIAN_POINT ( 'NONE',  ( 9.268856789657281325, -38.25380398711768493, 34.80090346875808649 ) ) ;
#30392 = ORIENTED_EDGE ( 'NONE', *, *, #1570, .T. ) ;
#30393 = EDGE_CURVE ( 'NONE', #21089, #17934, #19837, .T. ) ;
#30394 = ORIENTED_EDGE ( 'NONE', *, *, #11301, .T. ) ;
#30395 = DIRECTION ( 'NONE',  ( 1.000000000000000000, 0.000000000000000000, 0.000000000000000000 ) ) ;
#30396 = DIRECTION ( 'NONE',  ( 0.000000000000000000, 0.000000000000000000, 1.000000000000000000 ) ) ;
#30397 = VERTEX_POINT ( 'NONE', #17503 ) ;
#30398 = CARTESIAN_POINT ( 'NONE',  ( -11.64054540341807353, 16.26338533980437262, 24.50000000000000000 ) ) ;
#30399 = DIRECTION ( 'NONE',  ( -0.000000000000000000, -1.000000000000000000, -0.000000000000000000 ) ) ;
#30400 = ORIENTED_EDGE ( 'NONE', *, *, #18143, .T. ) ;
#30401 = CARTESIAN_POINT ( 'NONE',  ( 0.000000000000000000, 1.699320956058915452E-16, -1.500000000000001776 ) ) ;
#30402 = VECTOR ( 'NONE', #18133, 1000.000000000000000 ) ;
#30403 = DIRECTION ( 'NONE',  ( 0.000000000000000000, 1.000000000000000000, 0.000000000000000000 ) ) ;
#30404 = ORIENTED_EDGE ( 'NONE', *, *, #29793, .T. ) ;
#30405 = CARTESIAN_POINT ( 'NONE',  ( 13.93942108199810193, -16.65122935894600076, 1.500000000000000000 ) ) ;
#30406 = VERTEX_POINT ( 'NONE', #27023 ) ;
#30407 = DIRECTION ( 'NONE',  ( 0.000000000000000000, 1.000000000000000000, 0.000000000000000000 ) ) ;
#30408 = ORIENTED_EDGE ( 'NONE', *, *, #27295, .F. ) ;
#30409 = EDGE_LOOP ( 'NONE', ( #27925, #14229, #22712, #29062 ) ) ;
#30410 = EDGE_CURVE ( 'NONE', #23733, #9215, #15435, .T. ) ;
#30411 = LINE ( 'NONE', #18564, #18635 ) ;
#30412 = CARTESIAN_POINT ( 'NONE',  ( -15.34618562042307310, 12.82554431217321245, 5.652196082369965069 ) ) ;
#30413 = EDGE_CURVE ( 'NONE', #25485, #18996, #23785, .T. ) ;
#30414 = CARTESIAN_POINT ( 'NONE',  ( 9.263624429760991319, -14.28705663139043125, 18.63641924841378028 ) ) ;
#30415 = FACE_OUTER_BOUND ( 'NONE', #11894, .T. ) ;
#30416 = VERTEX_POINT ( 'NONE', #18273 ) ;
#30417 = CARTESIAN_POINT ( 'NONE',  ( -19.83108769839776997, 2.729924941536435945, 20.32842677360128292 ) ) ;
#30418 = CARTESIAN_POINT ( 'NONE',  ( 37.99999999999999289, 209.2686044187655909, -40.50000000000000711 ) ) ;
#30419 = CIRCLE ( 'NONE', #23933, 9.084132297865673777 ) ;
#30420 = CARTESIAN_POINT ( 'NONE',  ( -13.91614452448631667, 9.890357823660679060, 7.196036389296800451 ) ) ;
#30421 = CARTESIAN_POINT ( 'NONE',  ( 3.718735505629739091, 16.64535199026475709, 18.39992786714538298 ) ) ;
#30422 = ORIENTED_EDGE ( 'NONE', *, *, #27340, .F. ) ;
#30423 = ORIENTED_EDGE ( 'NONE', *, *, #23477, .F. ) ;
#30424 = PLANE ( 'NONE',  #30231 ) ;
#30425 = CARTESIAN_POINT ( 'NONE',  ( 10.58714538947712924, -13.39479915612166572, 7.158811349119582168 ) ) ;
#30426 = B_SPLINE_CURVE_WITH_KNOTS ( 'NONE', 3,
 ( #26186, #16677, #21034, #14025, #4668, #23987, #28217, #14331, #30557, #23842, #19167, #25886, #7166, #23527, #137, #28385 ),
 .UNSPECIFIED., .F., .F.,
 ( 4, 2, 2, 2, 2, 2, 2, 4 ),
 ( 0.4999999999999999445, 0.6250000000000008882, 0.6875000000000015543, 0.7187500000000019984, 0.7500000000000022204, 0.8125000000000013323, 0.8750000000000004441, 1.000000000000000000 ),
 .UNSPECIFIED. ) ;
#30427 = CARTESIAN_POINT ( 'NONE',  ( -5.762218391735197898, 19.17087124927422792, 18.36582235739946611 ) ) ;
#30428 = CARTESIAN_POINT ( 'NONE',  ( 0.000000000000000000, -9.742773481404436396E-15, -1.500000000000001332 ) ) ;
#30429 = CARTESIAN_POINT ( 'NONE',  ( 27.86235613436988245, -14.72519157938688927, 39.24389099736748676 ) ) ;
#30430 = CARTESIAN_POINT ( 'NONE',  ( 23.11727550875142612, -11.99039815441031465, 48.95928115119115631 ) ) ;
#30431 = ORIENTED_EDGE ( 'NONE', *, *, #27879, .T. ) ;
#30432 = CARTESIAN_POINT ( 'NONE',  ( -17.06456206750265281, 0.6636403356599883674, 6.892848776733236704 ) ) ;
#30433 = CARTESIAN_POINT ( 'NONE',  ( 14.27394986618626582, 14.00917565527016073, 18.84486140012299771 ) ) ;
#30434 = CARTESIAN_POINT ( 'NONE',  ( 19.87925100141002233, 2.194397331962204767, 19.21471108562414543 ) ) ;
#30435 = VERTEX_POINT ( 'NONE', #13742 ) ;
#30436 = CARTESIAN_POINT ( 'NONE',  ( -37.16608720827707657, -65.00000000000000000, 97.07879600563551037 ) ) ;
#30437 = ORIENTED_EDGE ( 'NONE', *, *, #26181, .F. ) ;
#30438 = CARTESIAN_POINT ( 'NONE',  ( 18.63200854944940232, -7.318485330915429188, 5.951255046771932733 ) ) ;
#30439 = AXIS2_PLACEMENT_3D ( 'NONE', #20538, #29917, #17912 ) ;
#30440 = CARTESIAN_POINT ( 'NONE',  ( -7.730328572437709767, 4.608906612435681005, -3.621320343559650379 ) ) ;
#30441 = ORIENTED_EDGE ( 'NONE', *, *, #22907, .F. ) ;
#30442 = DIRECTION ( 'NONE',  ( -1.000000000000000000, 0.000000000000000000, 0.000000000000000000 ) ) ;
#30443 = CARTESIAN_POINT ( 'NONE',  ( 3.424950581212853784, 49.88489954546552951, -40.38796021397682523 ) ) ;
#30444 = FACE_OUTER_BOUND ( 'NONE', #13878, .T. ) ;
#30445 = DIRECTION ( 'NONE',  ( 0.1423148382732851158, 0.9898214418809327952, 0.000000000000000000 ) ) ;
#30446 = CARTESIAN_POINT ( 'NONE',  ( -5.861334694664002143, 16.01657976118487881, 20.29915277494337644 ) ) ;
#30447 = DIRECTION ( 'NONE',  ( 1.000000000000000000, 0.000000000000000000, 0.000000000000000000 ) ) ;
#30448 = VERTEX_POINT ( 'NONE', #23084 ) ;
#30449 = CARTESIAN_POINT ( 'NONE',  ( -35.00000000000000000, 0.000000000000000000, 0.000000000000000000 ) ) ;
#30450 = B_SPLINE_CURVE_WITH_KNOTS ( 'NONE', 3,
 ( #26619, #16942, #14745, #4935, #28645, #14450, #5246, #26300, #9619, #14603, #23952, #24264, #4627, #25999 ),
 .UNSPECIFIED., .F., .F.,
 ( 4, 2, 2, 2, 2, 2, 4 ),
 ( 0.0007411796533686788348, 0.001115232222424166831, 0.001489284791479654826, 0.001863337360535142822, 0.002237389929590630818, 0.002985495067701606810, 0.003733600205812582801 ),
 .UNSPECIFIED. ) ;
#30451 = DIRECTION ( 'NONE',  ( -1.000000000000000000, 0.000000000000000000, 0.000000000000000000 ) ) ;
#30452 = ORIENTED_EDGE ( 'NONE', *, *, #10521, .T. ) ;
#30453 = CARTESIAN_POINT ( 'NONE',  ( 19.74250593591595049, 3.198927889078816644, 18.34798005863227388 ) ) ;
#30454 = CARTESIAN_POINT ( 'NONE',  ( 0.000000000000000000, -7.794228634059943595, 4.500000000000005329 ) ) ;
#30455 = VECTOR ( 'NONE', #19814, 1000.000000000000000 ) ;
#30456 = CARTESIAN_POINT ( 'NONE',  ( 2.185336383880204014, -8.817355867515821899, 13.22130136205108641 ) ) ;
#30457 = EDGE_LOOP ( 'NONE', ( #8714, #29529, #7078, #28691, #1771, #12785 ) ) ;
#30458 = CYLINDRICAL_SURFACE ( 'NONE', #12924, 20.00000000000000000 ) ;
#30459 = FACE_OUTER_BOUND ( 'NONE', #16042, .T. ) ;
#30460 = CARTESIAN_POINT ( 'NONE',  ( 24.13122067046371910, -33.41988417744658335, 34.50846293216257266 ) ) ;
#30461 = CYLINDRICAL_SURFACE ( 'NONE', #22539, 20.00000000000000000 ) ;
#30462 = EDGE_LOOP ( 'NONE', ( #22809, #21150, #10954, #8422 ) ) ;
#30463 = CARTESIAN_POINT ( 'NONE',  ( -3.196529495465446402, -8.413215745754985875, 21.50000000000000000 ) ) ;
#30464 = CARTESIAN_POINT ( 'NONE',  ( -12.56641067637752229, 40.32935944495016400, -1.500000000000000000 ) ) ;
#30465 = DIRECTION ( 'NONE',  ( -1.000000000000000000, 0.000000000000000000, 0.000000000000000000 ) ) ;
#30466 = VERTEX_POINT ( 'NONE', #3774 ) ;
#30467 = VECTOR ( 'NONE', #9869, 1000.000000000000000 ) ;
#30468 = DIRECTION ( 'NONE',  ( -0.000000000000000000, -0.000000000000000000, 1.000000000000000000 ) ) ;
#30469 = ORIENTED_EDGE ( 'NONE', *, *, #18705, .T. ) ;
#30470 = CARTESIAN_POINT ( 'NONE',  ( 0.000000000000000000, 0.000000000000000000, 12.49999999999998401 ) ) ;
#30471 = AXIS2_PLACEMENT_3D ( 'NONE', #1030, #20046, #10539 ) ;
#30472 = CARTESIAN_POINT ( 'NONE',  ( 30.74201181684196982, -15.50830195949553492, 40.56825029441215236 ) ) ;
#30473 = LINE ( 'NONE', #30334, #27798 ) ;
#30474 = ORIENTED_EDGE ( 'NONE', *, *, #16757, .F. ) ;
#30475 = LINE ( 'NONE', #15673, #12826 ) ;
#30476 = ADVANCED_FACE ( 'NONE', ( #13294 ), #21096, .T. ) ;
#30477 = DIRECTION ( 'NONE',  ( 0.000000000000000000, 0.000000000000000000, 1.000000000000000000 ) ) ;
#30478 = CARTESIAN_POINT ( 'NONE',  ( -4.163336342344337027E-14, 1.387778780781445676E-14, 1.500000000000000000 ) ) ;
#30479 = DIRECTION ( 'NONE',  ( 1.000000000000000000, 0.000000000000000000, 0.000000000000000000 ) ) ;
#30480 = ORIENTED_EDGE ( 'NONE', *, *, #22660, .T. ) ;
#30481 = EDGE_CURVE ( 'NONE', #2772, #11709, #21048, .T. ) ;
#30482 = CARTESIAN_POINT ( 'NONE',  ( -10.51513057463695233, -17.01270198993486460, 7.652108011868850035 ) ) ;
#30483 = CARTESIAN_POINT ( 'NONE',  ( 19.18576292979354747, 22.55620591602726677, 24.50000000000000000 ) ) ;
#30484 = CARTESIAN_POINT ( 'NONE',  ( -13.21131958021068087, 10.75991052173289120, 18.37259980046033547 ) ) ;
#30485 = DIRECTION ( 'NONE',  ( -0.000000000000000000, -0.000000000000000000, -1.000000000000000000 ) ) ;
#30486 = CARTESIAN_POINT ( 'NONE',  ( 3.540451764476295171, 16.69076635156335797, 20.24143955528809258 ) ) ;
#30487 = DIRECTION ( 'NONE',  ( 0.000000000000000000, 0.000000000000000000, 1.000000000000000000 ) ) ;
#30488 = VECTOR ( 'NONE', #1767, 1000.000000000000000 ) ;
#30489 = CARTESIAN_POINT ( 'NONE',  ( -18.43827498451963365, -7.794211480880301579, 19.77662771831109367 ) ) ;
#30490 = CARTESIAN_POINT ( 'NONE',  ( 19.64114023396309960, -37.13592150529014191, -1.500000000000000000 ) ) ;
#30491 = VERTEX_POINT ( 'NONE', #4830 ) ;
#30492 = ORIENTED_EDGE ( 'NONE', *, *, #18362, .F. ) ;
#30493 = FACE_OUTER_BOUND ( 'NONE', #29924, .T. ) ;
#30494 = CARTESIAN_POINT ( 'NONE',  ( 31.18700685317022803, -26.11823559933272421, -1.500000000000000000 ) ) ;
#30495 = DIRECTION ( 'NONE',  ( -1.000000000000000000, -1.224646799147308341E-16, 0.000000000000000000 ) ) ;
#30496 = VERTEX_POINT ( 'NONE', #30718 ) ;
#30497 = DIRECTION ( 'NONE',  ( 0.000000000000000000, 0.000000000000000000, 1.000000000000000000 ) ) ;
#30498 = CARTESIAN_POINT ( 'NONE',  ( 15.76678477342441020, -6.469363178373285450, 20.34789198813115263 ) ) ;
#30499 = CARTESIAN_POINT ( 'NONE',  ( 4.049916830765392994, 16.55712665160099561, 7.652108011868850035 ) ) ;
#30500 = ORIENTED_EDGE ( 'NONE', *, *, #10484, .T. ) ;
#30501 = CARTESIAN_POINT ( 'NONE',  ( -10.51513057463694523, -17.01270198993485394, 20.34789198813115263 ) ) ;
#30502 = CARTESIAN_POINT ( 'NONE',  ( -33.03787111873038640, -23.27353416640910311, -4.833238796522825176 ) ) ;
#30503 = EDGE_CURVE ( 'NONE', #28482, #9112, #18887, .T. ) ;
#30504 = CARTESIAN_POINT ( 'NONE',  ( -28.80398144066251831, 28.69005184980560230, 34.54961338325146869 ) ) ;
#30505 = ORIENTED_EDGE ( 'NONE', *, *, #29018, .T. ) ;
#30506 = CARTESIAN_POINT ( 'NONE',  ( 0.000000000000000000, 0.000000000000000000, 1.500000000000001332 ) ) ;
#30507 = VECTOR ( 'NONE', #7537, 1000.000000000000000 ) ;
#30508 = AXIS2_PLACEMENT_3D ( 'NONE', #16708, #7041, #2671 ) ;
#30509 = ADVANCED_FACE ( 'NONE', ( #4528 ), #26050, .T. ) ;
#30510 = EDGE_CURVE ( 'NONE', #6357, #386, #6713, .T. ) ;
#30511 = CIRCLE ( 'NONE', #19050, 9.482273699623480212 ) ;
#30512 = CARTESIAN_POINT ( 'NONE',  ( -26.81381729043377504, 6.366069288663346093, 43.19821070580857025 ) ) ;
#30513 = DIRECTION ( 'NONE',  ( 1.000000000000000000, 0.000000000000000000, 0.000000000000000000 ) ) ;
#30514 = EDGE_LOOP ( 'NONE', ( #4986, #1566, #13431, #24874 ) ) ;
#30515 = ADVANCED_FACE ( 'NONE', ( #14346 ), #16383, .T. ) ;
#30516 = CARTESIAN_POINT ( 'NONE',  ( 0.4564504349074266498, -9.471281197126616647, 1.500000000000001332 ) ) ;
#30517 = EDGE_CURVE ( 'NONE', #23101, #2292, #14184, .T. ) ;
#30518 = CARTESIAN_POINT ( 'NONE',  ( 39.99999999999998579, 87.00000000000001421, 15.49999999999999289 ) ) ;
#30519 = CARTESIAN_POINT ( 'NONE',  ( 1.837104849652355830E-15, 50.00000000000000000, -70.00000000000000000 ) ) ;
#30520 = FACE_OUTER_BOUND ( 'NONE', #29137, .T. ) ;
#30521 = DIRECTION ( 'NONE',  ( -0.000000000000000000, -0.000000000000000000, 1.000000000000000000 ) ) ;
#30522 = CARTESIAN_POINT ( 'NONE',  ( 28.34828976096172681, -29.18752572968383419, -1.500000000000000000 ) ) ;
#30523 = DIRECTION ( 'NONE',  ( -0.000000000000000000, -0.000000000000000000, 1.000000000000000000 ) ) ;
#30524 = VERTEX_POINT ( 'NONE', #21509 ) ;
#30525 = EDGE_CURVE ( 'NONE', #24284, #17232, #16346, .T. ) ;
#30526 = CARTESIAN_POINT ( 'NONE',  ( -6.312773474750901670, 15.86096687812979233, 7.269896094239230777 ) ) ;
#30527 = B_SPLINE_CURVE_WITH_KNOTS ( 'NONE', 3,
 ( #12307, #5444, #15091, #21809, #285, #911, #14481 ),
 .UNSPECIFIED., .F., .F.,
 ( 4, 3, 4 ),
 ( 0.000000000000000000, 0.005028111721449823532, 0.01005622344637598607 ),
 .UNSPECIFIED. ) ;
#30528 = DIRECTION ( 'NONE',  ( 0.000000000000000000, 1.000000000000000000, 0.000000000000000000 ) ) ;
#30529 = EDGE_CURVE ( 'NONE', #5002, #24171, #23541, .T. ) ;
#30530 = EDGE_LOOP ( 'NONE', ( #1912, #26259, #24054, #16610 ) ) ;
#30531 = EDGE_LOOP ( 'NONE', ( #15270, #15746, #73, #3021 ) ) ;
#30532 = EDGE_CURVE ( 'NONE', #7638, #10722, #2402, .T. ) ;
#30533 = B_SPLINE_CURVE_WITH_KNOTS ( 'NONE', 3,
 ( #9881, #29064, #24681, #24529, #24379, #2864, #22190, #3322, #519, #21887, #824, #21721, #12853, #22351, #17519, #26891, #19858, #8018, #28917, #17203, #29531, #12698, #10040, #19549, #26579, #10347, #12385, #5358, #989, #7708, #10500, #29378 ),
 .UNSPECIFIED., .F., .F.,
 ( 4, 2, 2, 2, 2, 2, 2, 2, 2, 2, 2, 2, 2, 2, 2, 4 ),
 ( 0.1181738554856288231, 0.1242296842490394210, 0.1257436414398920843, 0.1272575986307447338, 0.1302855130124500327, 0.1363413417758606305, 0.1378552989667132800, 0.1393692561575659017, 0.1423971705392711729, 0.1484529993026817429, 0.1514809136843869863, 0.1545088280660922853, 0.1605646568295027998, 0.1620786140203554493, 0.1635925712112080710, 0.1666204855929133422 ),
 .UNSPECIFIED. ) ;
#30534 = AXIS2_PLACEMENT_3D ( 'NONE', #27821, #3962, #1910 ) ;
#30535 = DIRECTION ( 'NONE',  ( 1.224646799147353207E-16, 1.000000000000000000, -0.000000000000000000 ) ) ;
#30536 = VECTOR ( 'NONE', #19567, 1000.000000000000000 ) ;
#30537 = DIRECTION ( 'NONE',  ( 1.000000000000000000, 0.000000000000000000, -0.000000000000000000 ) ) ;
#30538 = ORIENTED_EDGE ( 'NONE', *, *, #25270, .T. ) ;
#30539 = CARTESIAN_POINT ( 'NONE',  ( 15.12016594919360557, 13.11846484362264498, 20.29090034784956131 ) ) ;
#30540 = FACE_OUTER_BOUND ( 'NONE', #29912, .T. ) ;
#30541 = ORIENTED_EDGE ( 'NONE', *, *, #10348, .T. ) ;
#30542 = CARTESIAN_POINT ( 'NONE',  ( -26.36764545593177544, 31.31467416275353344, -1.500000000000000000 ) ) ;
#30543 = DIRECTION ( 'NONE',  ( 0.000000000000000000, 1.132880637372608986E-16, -1.000000000000000000 ) ) ;
#30544 = EDGE_LOOP ( 'NONE', ( #11184, #12062 ) ) ;
#30545 = DIRECTION ( 'NONE',  ( -0.000000000000000000, -0.000000000000000000, -1.000000000000000000 ) ) ;
#30546 = EDGE_CURVE ( 'NONE', #25524, #4513, #17341, .T. ) ;
#30547 = ORIENTED_EDGE ( 'NONE', *, *, #16891, .F. ) ;
#30548 = DIRECTION ( 'NONE',  ( -1.000000000000000000, 0.000000000000000000, 0.000000000000000000 ) ) ;
#30549 = EDGE_CURVE ( 'NONE', #4276, #22425, #1689, .T. ) ;
#30550 = ORIENTED_EDGE ( 'NONE', *, *, #25180, .F. ) ;
#30551 = EDGE_CURVE ( 'NONE', #977, #29639, #30781, .T. ) ;
#30552 = VERTEX_POINT ( 'NONE', #17469 ) ;
#30553 = CONICAL_SURFACE ( 'NONE', #21585, 9.000000000000000000, 1.047197551196600296 ) ;
#30554 = ADVANCED_FACE ( 'NONE', ( #26991, #19491, #17147 ), #26667, .T. ) ;
#30555 = CARTESIAN_POINT ( 'NONE',  ( -57.50000000000001421, 50.00000000000000000, 52.07879600563550326 ) ) ;
#30556 = CARTESIAN_POINT ( 'NONE',  ( 6.587096388939653657, -18.88412458026098406, 1.500000000000001332 ) ) ;
#30557 = CARTESIAN_POINT ( 'NONE',  ( -14.70303524442681642, -8.688445896238670585, 19.28454053338348473 ) ) ;
#30558 = CARTESIAN_POINT ( 'NONE',  ( 1.307979816482770286, -17.01201364160834117, 18.45571264222803975 ) ) ;
#30559 = CARTESIAN_POINT ( 'NONE',  ( 16.79398274391851942, 2.865066961627989350, 18.39701043959520987 ) ) ;
#30560 = ORIENTED_EDGE ( 'NONE', *, *, #11661, .F. ) ;
#30561 = EDGE_CURVE ( 'NONE', #4972, #6254, #28814, .T. ) ;
#30562 = CARTESIAN_POINT ( 'NONE',  ( -16.87659098782771494, 2.276273425076630552, 18.55820869691756769 ) ) ;
#30563 = CARTESIAN_POINT ( 'NONE',  ( 9.980880902826429590, -37.95465284280806628, 34.49999999999999289 ) ) ;
#30564 = CARTESIAN_POINT ( 'NONE',  ( -13.37849590052435289, 10.56201291103764284, 20.34789198813115263 ) ) ;
#30565 = CARTESIAN_POINT ( 'NONE',  ( 3.436936369909011635, 16.71530215271315711, 20.13759033520874908 ) ) ;
#30566 = ORIENTED_EDGE ( 'NONE', *, *, #5575, .F. ) ;
#30567 = ORIENTED_EDGE ( 'NONE', *, *, #14717, .T. ) ;
#30568 = CARTESIAN_POINT ( 'NONE',  ( 39.87350638640253919, -4.706224724400470016, -6.500000000000000888 ) ) ;
#30569 = FACE_BOUND ( 'NONE', #12255, .T. ) ;
#30570 = CARTESIAN_POINT ( 'NONE',  ( -5.439684697860717399, 16.15075171424583900, 18.35377592296120497 ) ) ;
#30571 = DIRECTION ( 'NONE',  ( 0.000000000000000000, 0.000000000000000000, -1.000000000000000000 ) ) ;
#30572 = CARTESIAN_POINT ( 'NONE',  ( -9.746783745056944781, 38.02984302254633064, 27.50000000000000711 ) ) ;
#30573 = AXIS2_PLACEMENT_3D ( 'NONE', #4719, #28437, #18619 ) ;
#30574 = DIRECTION ( 'NONE',  ( 0.000000000000000000, 0.000000000000000000, -1.000000000000000000 ) ) ;
#30575 = EDGE_CURVE ( 'NONE', #22188, #8257, #611, .T. ) ;
#30576 = EDGE_LOOP ( 'NONE', ( #4380, #23198, #14068, #19091 ) ) ;
#30577 = CIRCLE ( 'NONE', #27546, 0.7500000000000004441 ) ;
#30578 = EDGE_CURVE ( 'NONE', #4691, #22613, #7892, .T. ) ;
#30579 = CARTESIAN_POINT ( 'NONE',  ( -17.04940614979728508, 0.8516807413325234721, 6.041646659195333058 ) ) ;
#30580 = CARTESIAN_POINT ( 'NONE',  ( 32.98805937973593672, 0.000000000000000000, 8.000000000000003553 ) ) ;
#30581 = CARTESIAN_POINT ( 'NONE',  ( 19.86493687747362102, 2.320961355260791059, 19.85261563089511938 ) ) ;
#30582 = ORIENTED_EDGE ( 'NONE', *, *, #16791, .F. ) ;
#30583 = CARTESIAN_POINT ( 'NONE',  ( 24.03057240117691862, 26.57182937991349903, 24.50000000000000000 ) ) ;
#30584 = ORIENTED_EDGE ( 'NONE', *, *, #12202, .T. ) ;
#30585 = LINE ( 'NONE', #7034, #1978 ) ;
#30586 = CARTESIAN_POINT ( 'NONE',  ( -3.661196020523152406, 43.90033885078650400, -16.50000000000000000 ) ) ;
#30587 = ORIENTED_EDGE ( 'NONE', *, *, #12250, .T. ) ;
#30588 = CARTESIAN_POINT ( 'NONE',  ( 32.64610052339413926, -16.83154060456821810, 27.50000000000001421 ) ) ;
#30589 = LINE ( 'NONE', #9229, #6314 ) ;
#30590 = DIRECTION ( 'NONE',  ( -0.000000000000000000, 1.132880637372608986E-16, -1.000000000000000000 ) ) ;
#30591 = PLANE ( 'NONE',  #2395 ) ;
#30592 = CARTESIAN_POINT ( 'NONE',  ( -5.544451646083596863, 16.11829163520481956, 20.34789198813115263 ) ) ;
#30593 = LINE ( 'NONE', #28421, #20781 ) ;
#30594 = LINE ( 'NONE', #11728, #16833 ) ;
#30595 = ORIENTED_EDGE ( 'NONE', *, *, #6521, .T. ) ;
#30596 = CARTESIAN_POINT ( 'NONE',  ( 15.70758541206079428, -6.601999697740968287, 5.676815824193229609 ) ) ;
#30597 = DIRECTION ( 'NONE',  ( 0.000000000000000000, 0.000000000000000000, 1.000000000000000000 ) ) ;
#30598 = DIRECTION ( 'NONE',  ( 0.000000000000000000, 0.000000000000000000, -1.000000000000000000 ) ) ;
#30599 = ORIENTED_EDGE ( 'NONE', *, *, #9565, .F. ) ;
#30600 = FACE_OUTER_BOUND ( 'NONE', #9531, .T. ) ;
#30601 = CARTESIAN_POINT ( 'NONE',  ( -14.96594037876677596, -8.187306180225535357, 18.44527579819791185 ) ) ;
#30602 = CARTESIAN_POINT ( 'NONE',  ( -37.98493438988128901, 11.12428508575241004, -1.500000000000000000 ) ) ;
#30603 = CARTESIAN_POINT ( 'NONE',  ( 2.687479363073301819, 44.39187623479102740, -19.50000000000000355 ) ) ;
#30604 = EDGE_LOOP ( 'NONE', ( #26343, #17325, #17311 ) ) ;
#30605 = DIRECTION ( 'NONE',  ( -0.000000000000000000, -0.000000000000000000, 1.000000000000000000 ) ) ;
#30606 = CARTESIAN_POINT ( 'NONE',  ( -50.00000000000000000, -50.00000000000000000, 12.49999999999999112 ) ) ;
#30607 = CARTESIAN_POINT ( 'NONE',  ( 15.21181506329994804, -34.29657048623970894, 37.49999999996318678 ) ) ;
#30608 = CARTESIAN_POINT ( 'NONE',  ( -6.453144054752231185, 18.93070788617552580, 7.528076282304596134 ) ) ;
#30609 = EDGE_LOOP ( 'NONE', ( #11290, #12301, #30023, #23012 ) ) ;
#30610 = ORIENTED_EDGE ( 'NONE', *, *, #13063, .F. ) ;
#30611 = DIRECTION ( 'NONE',  ( 0.5406408174555974444, 0.8412535328311813165, 0.000000000000000000 ) ) ;
#30612 = CARTESIAN_POINT ( 'NONE',  ( -4.163336342344337027E-14, 1.387778780781445676E-14, 24.50000000000000000 ) ) ;
#30613 = EDGE_LOOP ( 'NONE', ( #21187, #26882, #2600, #22604, #12531, #22408, #30400, #12187, #26418, #16585, #15863, #30500 ) ) ;
#30614 = AXIS2_PLACEMENT_3D ( 'NONE', #21558, #195, #29207 ) ;
#30615 = EDGE_LOOP ( 'NONE', ( #17318, #28869, #60, #10243 ) ) ;
#30616 = CARTESIAN_POINT ( 'NONE',  ( 0.000000000000000000, 0.000000000000000000, 9.000000000000000000 ) ) ;
#30617 = ORIENTED_EDGE ( 'NONE', *, *, #14115, .F. ) ;
#30618 = CARTESIAN_POINT ( 'NONE',  ( -0.01062192699083570196, -17.02590662965304347, 18.71435384576123440 ) ) ;
#30619 = CARTESIAN_POINT ( 'NONE',  ( -10.46366670609033100, -17.06541516851461182, 7.652108011868850035 ) ) ;
#30620 = VECTOR ( 'NONE', #2550, 1000.000000000000000 ) ;
#30621 = DIRECTION ( 'NONE',  ( 0.000000000000000000, 1.000000000000000000, 0.000000000000000000 ) ) ;
#30622 = CARTESIAN_POINT ( 'NONE',  ( 1.230359340266123702, -17.01462811240319795, 18.44527579819791185 ) ) ;
#30623 = ORIENTED_EDGE ( 'NONE', *, *, #11683, .T. ) ;
#30624 = CARTESIAN_POINT ( 'NONE',  ( 5.105024945674004222, 42.22604126506330857, -1.500000000000003997 ) ) ;
#30625 = CARTESIAN_POINT ( 'NONE',  ( 16.70106355290778666, 3.455140589294515063, 7.652108011868851811 ) ) ;
#30626 = CARTESIAN_POINT ( 'NONE',  ( -24.35970437652574105, 13.37404834226503247, -16.55003854064094426 ) ) ;
#30627 = CARTESIAN_POINT ( 'NONE',  ( -25.23756106473024730, -11.43858098102957577, -1.500000000000000000 ) ) ;
#30628 = VERTEX_POINT ( 'NONE', #2972 ) ;
#30629 = CARTESIAN_POINT ( 'NONE',  ( -40.00000000000000000, 67.32050807568877815, 12.49999999999999112 ) ) ;
#30630 = B_SPLINE_CURVE_WITH_KNOTS ( 'NONE', 3,
 ( #3109, #19481, #24465, #22276 ),
 .UNSPECIFIED., .F., .F.,
 ( 4, 4 ),
 ( 3.018024802580205417E-07, 0.007932103453629119755 ),
 .UNSPECIFIED. ) ;
#30631 = CARTESIAN_POINT ( 'NONE',  ( -15.49717968187447603, -7.050617358802334422, 18.72771030977187579 ) ) ;
#30632 = DIRECTION ( 'NONE',  ( -0.000000000000000000, -1.000000000000000000, -0.000000000000000000 ) ) ;
#30633 = AXIS2_PLACEMENT_3D ( 'NONE', #9522, #16092, #4228 ) ;
#30634 = LINE ( 'NONE', #20961, #16015 ) ;
#30635 = CARTESIAN_POINT ( 'NONE',  ( 39.70095622559083637, -7.028748154384818925, -13.16666434783602924 ) ) ;
#30636 = CARTESIAN_POINT ( 'NONE',  ( -18.45576848551221616, -7.706141034055812966, 19.21471108562414898 ) ) ;
#30637 = LINE ( 'NONE', #4750, #21532 ) ;
#30638 = ORIENTED_EDGE ( 'NONE', *, *, #13745, .F. ) ;
#30639 = ORIENTED_EDGE ( 'NONE', *, *, #19013, .F. ) ;
#30640 = CARTESIAN_POINT ( 'NONE',  ( 33.03787111873281646, 23.27353416641277661, -4.833238796522779879 ) ) ;
#30641 = CARTESIAN_POINT ( 'NONE',  ( 37.98493438989863336, -11.12428508576153341, -1.500000000000000000 ) ) ;
#30642 = CARTESIAN_POINT ( 'NONE',  ( -3.662523238938586001, -12.47340865698848056, 1.500000000000001332 ) ) ;
#30643 = ORIENTED_EDGE ( 'NONE', *, *, #17740, .T. ) ;
#30644 = CARTESIAN_POINT ( 'NONE',  ( 15.54925513364909406, -6.943479002078025708, 20.12545155307891065 ) ) ;
#30645 = MECHANICAL_DESIGN_GEOMETRIC_PRESENTATION_REPRESENTATION (  '', ( #9803 ), #28231 ) ;
#30646 = CARTESIAN_POINT ( 'NONE',  ( 4.971436688744669041, 16.28007576866362882, 6.974106381145714018 ) ) ;
#30647 = ORIENTED_EDGE ( 'NONE', *, *, #9922, .F. ) ;
#30648 = CARTESIAN_POINT ( 'NONE',  ( 6.218621694205434203, 19.02754758079138853, 19.00652017443069752 ) ) ;
#30649 = CARTESIAN_POINT ( 'NONE',  ( -33.25198511595942819, -23.59839678289454667, -8.166573069426220854 ) ) ;
#30650 = CARTESIAN_POINT ( 'NONE',  ( -50.00000000000000000, 50.00000000000000000, 12.49999999999999112 ) ) ;
#30651 = CARTESIAN_POINT ( 'NONE',  ( -38.44186125115789565, 7.193762128604462625, 32.05965621367656837 ) ) ;
#30652 = ORIENTED_EDGE ( 'NONE', *, *, #17459, .T. ) ;
#30653 = FACE_OUTER_BOUND ( 'NONE', #21104, .T. ) ;
#30654 = CIRCLE ( 'NONE', #23674, 4.999999999999997335 ) ;
#30655 = CARTESIAN_POINT ( 'NONE',  ( 0.000000000000000000, -2.435693370351110282E-15, 21.50000000000000355 ) ) ;
#30656 = VECTOR ( 'NONE', #11401, 1000.000000000000227 ) ;
#30657 = DIRECTION ( 'NONE',  ( -1.000000000000000000, 0.000000000000000000, 0.000000000000000000 ) ) ;
#30658 = ORIENTED_EDGE ( 'NONE', *, *, #14265, .T. ) ;
#30659 = DIRECTION ( 'NONE',  ( 0.000000000000000000, 0.000000000000000000, -1.000000000000000000 ) ) ;
#30660 = CARTESIAN_POINT ( 'NONE',  ( 16.78337223357198482, 2.938206247954857631, 18.37259980046034258 ) ) ;
#30661 = FACE_OUTER_BOUND ( 'NONE', #18865, .T. ) ;
#30662 = CARTESIAN_POINT ( 'NONE',  ( 1.836970198721029589E-15, 90.00000000000001421, -70.00000000000000000 ) ) ;
#30664 = B_SPLINE_CURVE_WITH_KNOTS ( 'NONE', 3,
 ( #2689, #24359, #5335, #21400, #4872, #16724, #21547, #40, #2540, #28433, #21868, #341, #28583, #4715, #17032, #183, #14687, #10022, #14216, #17184 ),
 .UNSPECIFIED., .F., .F.,
 ( 4, 2, 2, 2, 2, 2, 2, 2, 2, 4 ),
 ( 0.000000000000000000, 0.06249999999999988898, 0.1249999999999997780, 0.1874999999999996669, 0.2187499999999995282, 0.2499999999999993339, 0.3124999999999994449, 0.3749999999999995559, 0.4374999999999996669, 0.4999999999999997780 ),
 .UNSPECIFIED. ) ;
#30663 = DIRECTION ( 'NONE',  ( -0.000000000000000000, 1.000000000000000000, -0.000000000000000000 ) ) ;
#30665 = MECHANICAL_DESIGN_GEOMETRIC_PRESENTATION_REPRESENTATION (  '', ( #17719 ), #30172 ) ;
#30666 = DIRECTION ( 'NONE',  ( 0.000000000000000000, -0.000000000000000000, 1.000000000000000000 ) ) ;
#30667 = CARTESIAN_POINT ( 'NONE',  ( -50.00000000000000000, 50.00000000000000000, 52.07879600563550326 ) ) ;
#30668 = CARTESIAN_POINT ( 'NONE',  ( 8.743977807160073112, 3.668292057956029861, 13.00000000000000178 ) ) ;
#30669 = CYLINDRICAL_SURFACE ( 'NONE', #16877, 0.7500000000000006661 ) ;
#30670 = ORIENTED_EDGE ( 'NONE', *, *, #7813, .F. ) ;
#30671 = ADVANCED_BREP_SHAPE_REPRESENTATION ( '', ( #12830, #7396 ), #3406 ) ;
#30672 = PLANE ( 'NONE',  #9762 ) ;
#30673 = DIRECTION ( 'NONE',  ( -0.2817325568414292825, -0.9594929736144974797, 0.000000000000000000 ) ) ;
#30674 = ORIENTED_EDGE ( 'NONE', *, *, #21356, .T. ) ;
#30675 = VERTEX_POINT ( 'NONE', #26836 ) ;
#30676 = AXIS2_PLACEMENT_3D ( 'NONE', #19026, #30706, #16376 ) ;
#30677 = CARTESIAN_POINT ( 'NONE',  ( -47.14142842854255377, 69.79466010243307039, 59.50000000000029843 ) ) ;
#30678 = CIRCLE ( 'NONE', #21207, 3.000000000000002665 ) ;
#30679 = CARTESIAN_POINT ( 'NONE',  ( 12.72536390617885438, -2.839914339433650348, 1.500000000000001332 ) ) ;
#30680 = ORIENTED_EDGE ( 'NONE', *, *, #6527, .F. ) ;
#30681 = CIRCLE ( 'NONE', #2823, 1.447898107987198646 ) ;
#30682 = ADVANCED_FACE ( 'NONE', ( #24322 ), #19959, .F. ) ;
#30683 = CARTESIAN_POINT ( 'NONE',  ( 12.58124959699792456, 11.48680237977196228, 20.29090034784956131 ) ) ;
#30684 =( LENGTH_UNIT ( ) NAMED_UNIT ( * ) SI_UNIT ( .MILLI., .METRE. ) );
#30685 = ORIENTED_EDGE ( 'NONE', *, *, #22919, .T. ) ;
#30686 = EDGE_CURVE ( 'NONE', #17274, #4954, #12884, .T. ) ;
#30687 = CARTESIAN_POINT ( 'NONE',  ( -7.538175180318456903, -5.069257791428354309, -1.500000000000002442 ) ) ;
#30688 = AXIS2_PLACEMENT_3D ( 'NONE', #24309, #12476, #21966 ) ;
#30689 = DIRECTION ( 'NONE',  ( 0.000000000000000000, 0.000000000000000000, -1.000000000000000000 ) ) ;
#30690 = ORIENTED_EDGE ( 'NONE', *, *, #26381, .T. ) ;
#30691 = ORIENTED_EDGE ( 'NONE', *, *, #17028, .F. ) ;
#30692 = ORIENTED_EDGE ( 'NONE', *, *, #9738, .F. ) ;
#30693 = EDGE_CURVE ( 'NONE', #8468, #29572, #29479, .T. ) ;
#30694 = ORIENTED_EDGE ( 'NONE', *, *, #2427, .F. ) ;
#30696 = EDGE_CURVE ( 'NONE', #19427, #12321, #10280, .T. ) ;
#30695 = AXIS2_PLACEMENT_3D ( 'NONE', #18142, #27355, #6277 ) ;
#30697 = VECTOR ( 'NONE', #14752, 1000.000000000000000 ) ;
#30698 = DIRECTION ( 'NONE',  ( 1.000000000000000000, 0.000000000000000000, -0.000000000000000000 ) ) ;
#30699 = CARTESIAN_POINT ( 'NONE',  ( -17.64259547893121649, -9.420269215336073643, 6.149077423860703995 ) ) ;
#30700 = AXIS2_PLACEMENT_3D ( 'NONE', #24975, #29511, #15456 ) ;
#30701 = CARTESIAN_POINT ( 'NONE',  ( 15.41296542101254552, 5.939519782021115191, 1.500000000000000000 ) ) ;
#30702 = CARTESIAN_POINT ( 'NONE',  ( 0.7788148816922458861, -17.02744011591804707, 20.34789198813115263 ) ) ;
#30703 = DIRECTION ( 'NONE',  ( 1.000000000000000000, 0.000000000000000000, 0.000000000000000000 ) ) ;
#30704 = EDGE_LOOP ( 'NONE', ( #3193, #4190, #27064, #12339 ) ) ;
#30705 = CARTESIAN_POINT ( 'NONE',  ( -19.72724879956887278, 3.398799651952296053, 18.90679857307105749 ) ) ;
#30706 = DIRECTION ( 'NONE',  ( 0.000000000000000000, 0.000000000000000000, 1.000000000000000000 ) ) ;
#30707 = FACE_OUTER_BOUND ( 'NONE', #513, .T. ) ;
#30708 = AXIS2_PLACEMENT_3D ( 'NONE', #17683, #22505, #13015 ) ;
#30709 = PLANE ( 'NONE',  #25761 ) ;
#30710 = ORIENTED_EDGE ( 'NONE', *, *, #26501, .F. ) ;
#30711 = ORIENTED_EDGE ( 'NONE', *, *, #25839, .F. ) ;
#30712 = CARTESIAN_POINT ( 'NONE',  ( 24.03057240117691862, 26.57182937991349903, 26.54355021145562787 ) ) ;
#30713 = AXIS2_PLACEMENT_3D ( 'NONE', #12933, #27269, #8093 ) ;
#30714 = ADVANCED_FACE ( 'NONE', ( #14653 ), #14135, .T. ) ;
#30715 = CARTESIAN_POINT ( 'NONE',  ( 0.000000000000000000, 0.000000000000000000, 27.50000000000000355 ) ) ;
#30716 = EDGE_CURVE ( 'NONE', #8853, #10182, #19344, .T. ) ;
#30717 = CARTESIAN_POINT ( 'NONE',  ( 1.808288630848430056, -42.50000000000000711, 19.72227980406325898 ) ) ;
#30718 = CARTESIAN_POINT ( 'NONE',  ( -52.16608720827707657, 36.86186943028246787, 12.49999999999999112 ) ) ;
#30719 = EDGE_CURVE ( 'NONE', #438, #22753, #28099, .T. ) ;
#30720 = DIRECTION ( 'NONE',  ( -0.000000000000000000, 1.132880637372608986E-16, -1.000000000000000000 ) ) ;
#30721 = AXIS2_PLACEMENT_3D ( 'NONE', #14204, #7518, #325 ) ;
#30722 = CARTESIAN_POINT ( 'NONE',  ( 35.45878215871448447, 7.046087300365224237, 34.64822579837520777 ) ) ;
#30723 = AXIS2_PLACEMENT_3D ( 'NONE', #14453, #23956, #16486 ) ;
#30724 = CYLINDRICAL_SURFACE ( 'NONE', #10937, 0.7500000000000006661 ) ;
#30725 = VERTEX_POINT ( 'NONE', #3580 ) ;
#30726 = ADVANCED_FACE ( 'NONE', ( #17769 ), #13103, .F. ) ;
#30727 = AXIS2_PLACEMENT_3D ( 'NONE', #4526, #23851, #14036 ) ;
#30728 = CARTESIAN_POINT ( 'NONE',  ( -17.05537006572908609, 0.7816414089123764342, 6.131018562779544823 ) ) ;
#30729 = CARTESIAN_POINT ( 'NONE',  ( 14.70074466696773996, 13.56107787884953630, 18.37545668562166412 ) ) ;
#30730 = CARTESIAN_POINT ( 'NONE',  ( -5.881244434206279514, -6.812559277181949646, 21.50000000000000000 ) ) ;
#30731 = EDGE_CURVE ( 'NONE', #29639, #22904, #18844, .T. ) ;
#30732 = VERTEX_POINT ( 'NONE', #23046 ) ;
#30733 = CYLINDRICAL_SURFACE ( 'NONE', #3872, 1.000000000000007772 ) ;
#30734 = ORIENTED_EDGE ( 'NONE', *, *, #9001, .T. ) ;
#30735 = EDGE_CURVE ( 'NONE', #6045, #23454, #15853, .T. ) ;
#30736 = CARTESIAN_POINT ( 'NONE',  ( -0.8633855750855333744, -42.50000000000000000, 28.83974596215560737 ) ) ;
#30737 = CIRCLE ( 'NONE', #21266, 50.00000000000000000 ) ;
#30738 = DIRECTION ( 'NONE',  ( 1.000000000000000000, 0.000000000000000000, 0.000000000000000000 ) ) ;
#30739 = AXIS2_PLACEMENT_3D ( 'NONE', #23724, #19206, #12195 ) ;
#30740 = ORIENTED_EDGE ( 'NONE', *, *, #29385, .T. ) ;
#30741 = CARTESIAN_POINT ( 'NONE',  ( 35.89013898050658469, 3.144164291784017795, 27.50000000000000000 ) ) ;
#30742 = CIRCLE ( 'NONE', #12326, 20.00000000000000355 ) ;
#30743 = CARTESIAN_POINT ( 'NONE',  ( 9.994988777600744001E-16, -0.8794428697894486335, 9.000000000000001776 ) ) ;
#30744 = CARTESIAN_POINT ( 'NONE',  ( 10.29773160325293979, -13.60426929937658436, 18.45571264222803975 ) ) ;
#30745 = CARTESIAN_POINT ( 'NONE',  ( 14.36006998371584054, 17.26937953831785677, -1.500000000000000000 ) ) ;
#30746 = CARTESIAN_POINT ( 'NONE',  ( -4.163336342344337027E-14, 1.387778780781445676E-14, 24.50000000000000000 ) ) ;
#30747 = AXIS2_PLACEMENT_3D ( 'NONE', #22424, #3403, #13235 ) ;
#30748 = CARTESIAN_POINT ( 'NONE',  ( 0.000000000000000000, 9.084132297865666672, 65.52304386563415051 ) ) ;
#30749 = CARTESIAN_POINT ( 'NONE',  ( -0.1262659238204836554, -8.999114229549588728, -1.500000000000002665 ) ) ;
#30750 = CARTESIAN_POINT ( 'NONE',  ( -31.79271162922631078, 14.90794587988477637, 39.88583012296479779 ) ) ;
#30751 = ORIENTED_EDGE ( 'NONE', *, *, #21958, .T. ) ;
#30752 = ADVANCED_FACE ( 'NONE', ( #14298 ), #14841, .F. ) ;
#30753 = CARTESIAN_POINT ( 'NONE',  ( 23.17581250239729940, 34.50630206824671120, 1.499999999999999778 ) ) ;
#30754 = AXIS2_PLACEMENT_3D ( 'NONE', #12857, #22356, #15325 ) ;
#30755 = CARTESIAN_POINT ( 'NONE',  ( 32.74775157612609178, -27.21557300919356948, -19.50000000000000355 ) ) ;
#30756 = DIRECTION ( 'NONE',  ( 0.000000000000000000, -0.000000000000000000, -1.000000000000000000 ) ) ;
#30757 = ORIENTED_EDGE ( 'NONE', *, *, #18588, .F. ) ;
#30758 = CYLINDRICAL_SURFACE ( 'NONE', #3606, 7.500000000000007994 ) ;
#30759 = CARTESIAN_POINT ( 'NONE',  ( -14.73262409220165203, -8.633676228711859579, 19.69140814234746273 ) ) ;
#30760 = EDGE_CURVE ( 'NONE', #5874, #6566, #11820, .T. ) ;
#30761 = AXIS2_PLACEMENT_3D ( 'NONE', #14996, #12679, #29043 ) ;
#30762 = DIRECTION ( 'NONE',  ( -0.000000000000000000, -0.000000000000000000, 1.000000000000000000 ) ) ;
#30763 = EDGE_CURVE ( 'NONE', #9112, #16844, #9370, .T. ) ;
#30764 = CARTESIAN_POINT ( 'NONE',  ( 0.09252763182292053634, 8.674330214978047238, 2.975619346028167911 ) ) ;
#30765 = DIRECTION ( 'NONE',  ( 1.000000000000000000, 0.000000000000000000, -0.000000000000000000 ) ) ;
#30766 = AXIS2_PLACEMENT_3D ( 'NONE', #1655, #8211, #17889 ) ;
#30767 = ORIENTED_EDGE ( 'NONE', *, *, #9944, .T. ) ;
#30768 = DIRECTION ( 'NONE',  ( -0.000000000000000000, -0.000000000000000000, 1.000000000000000000 ) ) ;
#30769 = CARTESIAN_POINT ( 'NONE',  ( -23.96732207939035675, 33.98584080153585774, -1.500000000000000000 ) ) ;
#30770 = CARTESIAN_POINT ( 'NONE',  ( 37.50556493705014560, -0.1197015986419610323, 37.50000000002331291 ) ) ;
#30771 = CARTESIAN_POINT ( 'NONE',  ( -6.962021646281573162, -6.437683520590147701, 21.50000000000000000 ) ) ;
#30772 = DIRECTION ( 'NONE',  ( 0.000000000000000000, 0.000000000000000000, 1.000000000000000000 ) ) ;
#30773 = AXIS2_PLACEMENT_3D ( 'NONE', #2597, #11966, #21456 ) ;
#30774 = CARTESIAN_POINT ( 'NONE',  ( 7.869584159753955532, 10.39565510934977333, 1.500000000000001332 ) ) ;
#30775 = DIRECTION ( 'NONE',  ( 0.000000000000000000, 0.000000000000000000, 1.000000000000000000 ) ) ;
#30776 = ORIENTED_EDGE ( 'NONE', *, *, #9609, .F. ) ;
#30777 = VERTEX_POINT ( 'NONE', #2467 ) ;
#30778 = DIRECTION ( 'NONE',  ( 1.000000000000000000, 0.000000000000000000, 0.000000000000000000 ) ) ;
#30779 = ORIENTED_EDGE ( 'NONE', *, *, #19079, .T. ) ;
#30780 = CARTESIAN_POINT ( 'NONE',  ( 0.6691466709101893118, -17.02906906675068299, 18.35377592296120497 ) ) ;
#30781 = CIRCLE ( 'NONE', #27305, 3.000000000000002665 ) ;
#30782 = CARTESIAN_POINT ( 'NONE',  ( 9.406652940105985294, -1.195154792889423057, 13.00000000000000178 ) ) ;
#30783 = AXIS2_PLACEMENT_3D ( 'NONE', #18185, #6322, #13514 ) ;
#30784 = DIRECTION ( 'NONE',  ( 1.000000000000000000, 0.000000000000000000, 0.000000000000000000 ) ) ;
#30785 = CARTESIAN_POINT ( 'NONE',  ( 0.3493067888074719574, -20.01473451864463371, 20.34789198813115263 ) ) ;
#30786 = AXIS2_PLACEMENT_3D ( 'NONE', #9815, #26980, #26500 ) ;
#30787 = ORIENTED_EDGE ( 'NONE', *, *, #21635, .F. ) ;
#30788 = DIRECTION ( 'NONE',  ( 0.000000000000000000, 0.000000000000000000, 1.000000000000000000 ) ) ;
#30789 = DIRECTION ( 'NONE',  ( -0.1423148382732853101, 0.9898214418809327952, 0.000000000000000000 ) ) ;
#30790 = CARTESIAN_POINT ( 'NONE',  ( 14.20930976959225589, 14.09970620734104862, 19.14333282897057842 ) ) ;
#30791 = CARTESIAN_POINT ( 'NONE',  ( 19.74250593591594694, 3.198927889078816644, 5.652196082369963293 ) ) ;
#30792 = ORIENTED_EDGE ( 'NONE', *, *, #8786, .T. ) ;
#30793 = ADVANCED_FACE ( 'NONE', ( #7299 ), #16354, .F. ) ;
#30794 = CIRCLE ( 'NONE', #924, 1.447898107987198646 ) ;
#30795 = LINE ( 'NONE', #16752, #8319 ) ;
#30796 = CARTESIAN_POINT ( 'NONE',  ( -13.05132497920497237, 10.94401179279849323, 18.47056384035244037 ) ) ;
#30797 = LINE ( 'NONE', #25667, #21975 ) ;
#30798 = CARTESIAN_POINT ( 'NONE',  ( -23.08991993893192785, -11.27014480227852644, 49.30668222215589225 ) ) ;
#30799 = CARTESIAN_POINT ( 'NONE',  ( 0.000000000000000000, 1.699320956058915452E-16, -1.500000000000001776 ) ) ;
#30800 = PLANE ( 'NONE',  #6141 ) ;
#30801 = ORIENTED_EDGE ( 'NONE', *, *, #16048, .T. ) ;
#30802 = ORIENTED_EDGE ( 'NONE', *, *, #25632, .T. ) ;
#30803 = CARTESIAN_POINT ( 'NONE',  ( 33.35889462893408819, 23.76060431982160281, -9.833271596736157250 ) ) ;
#30804 = CARTESIAN_POINT ( 'NONE',  ( 23.96732207937828463, 33.98584080152456011, -1.500000000000000000 ) ) ;
#30805 = AXIS2_PLACEMENT_3D ( 'NONE', #25529, #11783, #18364 ) ;
#30806 = LINE ( 'NONE', #11337, #16887 ) ;
#30807 = FACE_OUTER_BOUND ( 'NONE', #6038, .T. ) ;
#30808 = EDGE_LOOP ( 'NONE', ( #5950, #1180 ) ) ;
#30809 =( NAMED_UNIT ( * ) SI_UNIT ( $, .STERADIAN. ) SOLID_ANGLE_UNIT ( ) );
#30810 = AXIS2_PLACEMENT_3D ( 'NONE', #5065, #75, #24390 ) ;
#30811 = CARTESIAN_POINT ( 'NONE',  ( 15.67520293387195807, -6.672517015027191967, 20.29090034784956131 ) ) ;
#30812 = VECTOR ( 'NONE', #29729, 1000.000000000000000 ) ;
#30813 = CARTESIAN_POINT ( 'NONE',  ( 4.654893560761754756, 16.38086414125081802, 5.862424720655265098 ) ) ;
#30814 = ORIENTED_EDGE ( 'NONE', *, *, #1000, .F. ) ;
#30815 = CARTESIAN_POINT ( 'NONE',  ( 11.73047935159229915, 12.40726572549740325, 7.098451512883313441 ) ) ;
#30816 = VECTOR ( 'NONE', #23011, 1000.000000000000000 ) ;
#30817 = CARTESIAN_POINT ( 'NONE',  ( -11.29700601561300743, -42.33790872007643458, -16.50000000000000355 ) ) ;
#30818 = CARTESIAN_POINT ( 'NONE',  ( -35.03120574897558726, 13.44240695278457309, 37.49999999996620659 ) ) ;
#30819 = EDGE_LOOP ( 'NONE', ( #4904, #18939, #10846, #26634, #20029, #13074 ) ) ;
#30820 = DIRECTION ( 'NONE',  ( 0.7557495743542582689, -0.6548607339452851006, 0.000000000000000000 ) ) ;
#30821 = DIRECTION ( 'NONE',  ( -0.000000000000000000, -0.000000000000000000, -1.000000000000000000 ) ) ;
#30822 = CIRCLE ( 'NONE', #4007, 0.7499999999999997780 ) ;
#30823 = FACE_OUTER_BOUND ( 'NONE', #5072, .T. ) ;
#30824 = VERTEX_POINT ( 'NONE', #4186 ) ;
#30825 = CARTESIAN_POINT ( 'NONE',  ( -18.15888143814677136, -8.424936462863948705, 7.632642797338977658 ) ) ;
#30826 = CARTESIAN_POINT ( 'NONE',  ( 16.74328841314636662, 3.194145055459935545, 20.34789198813115263 ) ) ;
#30827 = PRODUCT_DEFINITION_SHAPE ( 'NONE', 'NONE',  #14665 ) ;
#30828 = CARTESIAN_POINT ( 'NONE',  ( -0.07785784566753103930, -17.02422498921964689, 6.111214848085761986 ) ) ;
#30829 = CIRCLE ( 'NONE', #10928, 0.7500000000000006661 ) ;
#30830 = CARTESIAN_POINT ( 'NONE',  ( -8.999114229549592281, 0.1262659238205133538, 1.500000000000001332 ) ) ;
#30831 = FACE_OUTER_BOUND ( 'NONE', #14747, .T. ) ;
#30832 = CARTESIAN_POINT ( 'NONE',  ( -19.95437879344081011, 1.590546279198205237, 19.79423548914561692 ) ) ;
#30833 = LINE ( 'NONE', #11810, #22357 ) ;
#30834 = ORIENTED_EDGE ( 'NONE', *, *, #26547, .F. ) ;
#30835 = CARTESIAN_POINT ( 'NONE',  ( 11.11463800144301928, -16.64861661464430398, 20.34789198813115263 ) ) ;
#30836 = VECTOR ( 'NONE', #22946, 1000.000000000000000 ) ;
#30837 = DIRECTION ( 'NONE',  ( 0.000000000000000000, 0.000000000000000000, -1.000000000000000000 ) ) ;
#30838 = ORIENTED_EDGE ( 'NONE', *, *, #6483, .F. ) ;
#30839 = VERTEX_POINT ( 'NONE', #21156 ) ;
#30840 = DIRECTION ( 'NONE',  ( -1.000000000000000000, 1.224646799147351975E-16, 0.000000000000000000 ) ) ;
#30841 = EDGE_LOOP ( 'NONE', ( #9440, #30117 ) ) ;
#30842 = VECTOR ( 'NONE', #16364, 1000.000000000000000 ) ;
#30843 = CARTESIAN_POINT ( 'NONE',  ( -8.884323311075783991, -1.438332125858144295, 21.50000000000000000 ) ) ;
#30844 = CARTESIAN_POINT ( 'NONE',  ( -4.163336342344337027E-14, -1.387778780781445676E-14, 1.500000000000000000 ) ) ;
#30845 = ORIENTED_EDGE ( 'NONE', *, *, #23433, .T. ) ;
#30846 = CARTESIAN_POINT ( 'NONE',  ( 18.65775367615955460, -7.252215724661033036, 18.73743063545763121 ) ) ;
#30847 = CARTESIAN_POINT ( 'NONE',  ( 19.60273500773784860, 4.055073576757204812, 18.82680253904184298 ) ) ;
#30848 = DIRECTION ( 'NONE',  ( -0.000000000000000000, 1.132880637372608986E-16, -1.000000000000000000 ) ) ;
#30849 = EDGE_LOOP ( 'NONE', ( #8609, #1737, #27578, #30801 ) ) ;
#30850 = CYLINDRICAL_SURFACE ( 'NONE', #20766, 21.71568325578202163 ) ;
#30851 = ORIENTED_EDGE ( 'NONE', *, *, #29199, .F. ) ;
#30852 = VECTOR ( 'NONE', #16279, 1000.000000000000000 ) ;
#30853 = VERTEX_POINT ( 'NONE', #11985 ) ;
#30854 = EDGE_CURVE ( 'NONE', #24660, #19294, #27331, .T. ) ;
#30855 = FACE_OUTER_BOUND ( 'NONE', #21240, .T. ) ;
#30856 = CARTESIAN_POINT ( 'NONE',  ( -0.2239719228509424731, -17.01994463034878891, 19.47784884541372818 ) ) ;
#30857 = VECTOR ( 'NONE', #29588, 1000.000000000000000 ) ;
#30858 = CARTESIAN_POINT ( 'NONE',  ( 0.000000000000000000, -7.794228634059943595, 4.500000000000005329 ) ) ;
#30859 = NEXT_ASSEMBLY_USAGE_OCCURRENCE ( 'NAUO1', ' ', ' ', #18311, #6845, $ ) ;
#30860 = NEXT_ASSEMBLY_USAGE_OCCURRENCE ( 'NAUO2', ' ', ' ', #18311, #2093, $ ) ;
#30861 = NEXT_ASSEMBLY_USAGE_OCCURRENCE ( 'NAUO3', ' ', ' ', #18311, #7631, $ ) ;
#30862 = NEXT_ASSEMBLY_USAGE_OCCURRENCE ( 'NAUO4', ' ', ' ', #18311, #12777, $ ) ;
#30863 = NEXT_ASSEMBLY_USAGE_OCCURRENCE ( 'NAUO5', ' ', ' ', #18311, #14665, $ ) ;
#30864 = NEXT_ASSEMBLY_USAGE_OCCURRENCE ( 'NAUO6', ' ', ' ', #18311, #7631, $ ) ;
#30865 = NEXT_ASSEMBLY_USAGE_OCCURRENCE ( 'NAUO7', ' ', ' ', #18311, #24773, $ ) ;
#30866 = NEXT_ASSEMBLY_USAGE_OCCURRENCE ( 'NAUO8', ' ', ' ', #18311, #22874, $ ) ;
#30867 = NEXT_ASSEMBLY_USAGE_OCCURRENCE ( 'NAUO9', ' ', ' ', #18311, #3621, $ ) ;
#30868 = NEXT_ASSEMBLY_USAGE_OCCURRENCE ( 'NAUO10', ' ', ' ', #18311, #10487, $ ) ;
#30869 = NEXT_ASSEMBLY_USAGE_OCCURRENCE ( 'NAUO11', ' ', ' ', #18311, #21923, $ ) ;
#30870 = NEXT_ASSEMBLY_USAGE_OCCURRENCE ( 'NAUO12', ' ', ' ', #18311, #21923, $ ) ;
#30871 = NEXT_ASSEMBLY_USAGE_OCCURRENCE ( 'NAUO13', ' ', ' ', #18311, #21923, $ ) ;
#30872 = NEXT_ASSEMBLY_USAGE_OCCURRENCE ( 'NAUO14', ' ', ' ', #18311, #21923, $ ) ;
#30873=COLOUR_RGB('Dark Blue',0.08,0.2,0.34);
#30874=FILL_AREA_STYLE_COLOUR('',#30873);
#30875=FILL_AREA_STYLE('',(#30874));
#30876=SURFACE_STYLE_FILL_AREA(#30875);
#30877=SURFACE_SIDE_STYLE('',(#30876));
#30878=SURFACE_STYLE_USAGE(.BOTH.,#30877);
#30879=PRESENTATION_STYLE_ASSIGNMENT((#30878));
#30880=COLOUR_RGB('Light Blue',0.38,0.62,0.78);
#30881=FILL_AREA_STYLE_COLOUR('',#30880);
#30882=FILL_AREA_STYLE('',(#30881));
#30883=SURFACE_STYLE_FILL_AREA(#30882);
#30884=SURFACE_SIDE_STYLE('',(#30883));
#30885=SURFACE_STYLE_USAGE(.BOTH.,#30884);
#30886=PRESENTATION_STYLE_ASSIGNMENT((#30885));
#30887=COLOUR_RGB('Sky Blue',0.24,0.69,0.87);
#30888=FILL_AREA_STYLE_COLOUR('',#30887);
#30889=FILL_AREA_STYLE('',(#30888));
#30890=SURFACE_STYLE_FILL_AREA(#30889);
#30891=SURFACE_SIDE_STYLE('',(#30890));
#30892=SURFACE_STYLE_USAGE(.BOTH.,#30891);
#30893=PRESENTATION_STYLE_ASSIGNMENT((#30892));
#30894=COLOUR_RGB('Grey',0.48,0.52,0.57);
#30895=FILL_AREA_STYLE_COLOUR('',#30894);
#30896=FILL_AREA_STYLE('',(#30895));
#30897=SURFACE_STYLE_FILL_AREA(#30896);
#30898=SURFACE_SIDE_STYLE('',(#30897));
#30899=SURFACE_STYLE_USAGE(.BOTH.,#30898);
#30900=PRESENTATION_STYLE_ASSIGNMENT((#30899));
#30901=COLOUR_RGB('Black',0.12,0.14,0.17);
#30902=FILL_AREA_STYLE_COLOUR('',#30901);
#30903=FILL_AREA_STYLE('',(#30902));
#30904=SURFACE_STYLE_FILL_AREA(#30903);
#30905=SURFACE_SIDE_STYLE('',(#30904));
#30906=SURFACE_STYLE_USAGE(.BOTH.,#30905);
#30907=PRESENTATION_STYLE_ASSIGNMENT((#30906));
#30908=COLOUR_RGB('Off White',0.89,0.88,0.83);
#30909=FILL_AREA_STYLE_COLOUR('',#30908);
#30910=FILL_AREA_STYLE('',(#30909));
#30911=SURFACE_STYLE_FILL_AREA(#30910);
#30912=SURFACE_SIDE_STYLE('',(#30911));
#30913=SURFACE_STYLE_USAGE(.BOTH.,#30912);
#30914=PRESENTATION_STYLE_ASSIGNMENT((#30913));
ENDSEC;
END-ISO-10303-21;
